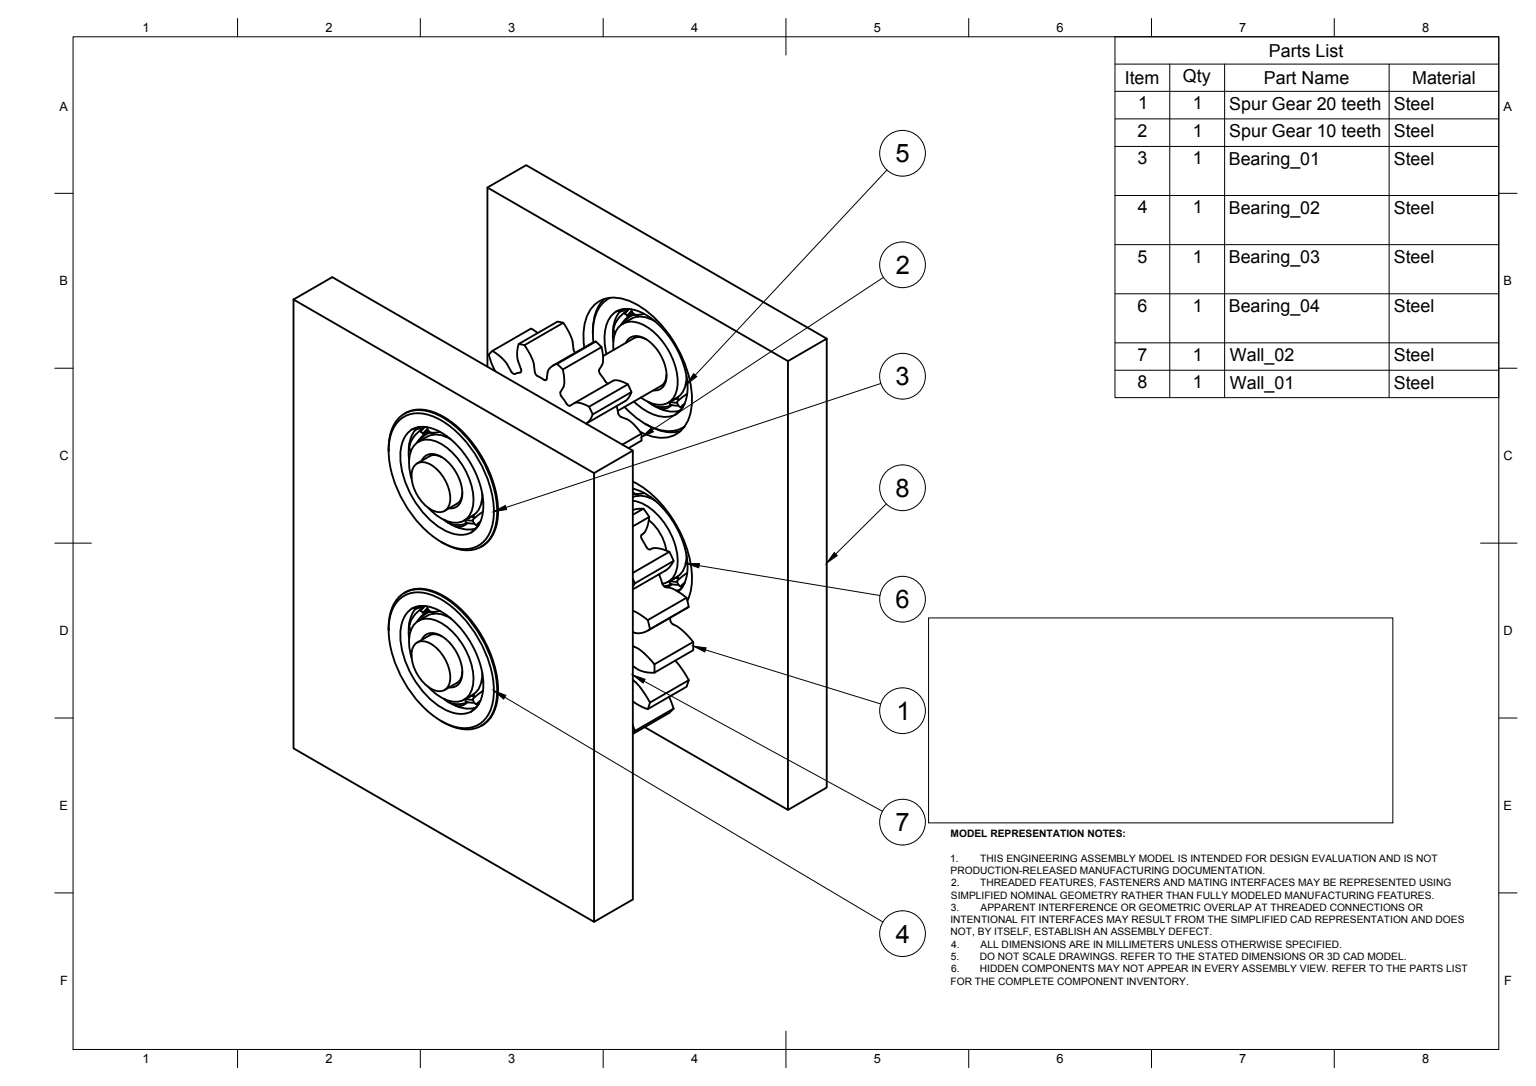
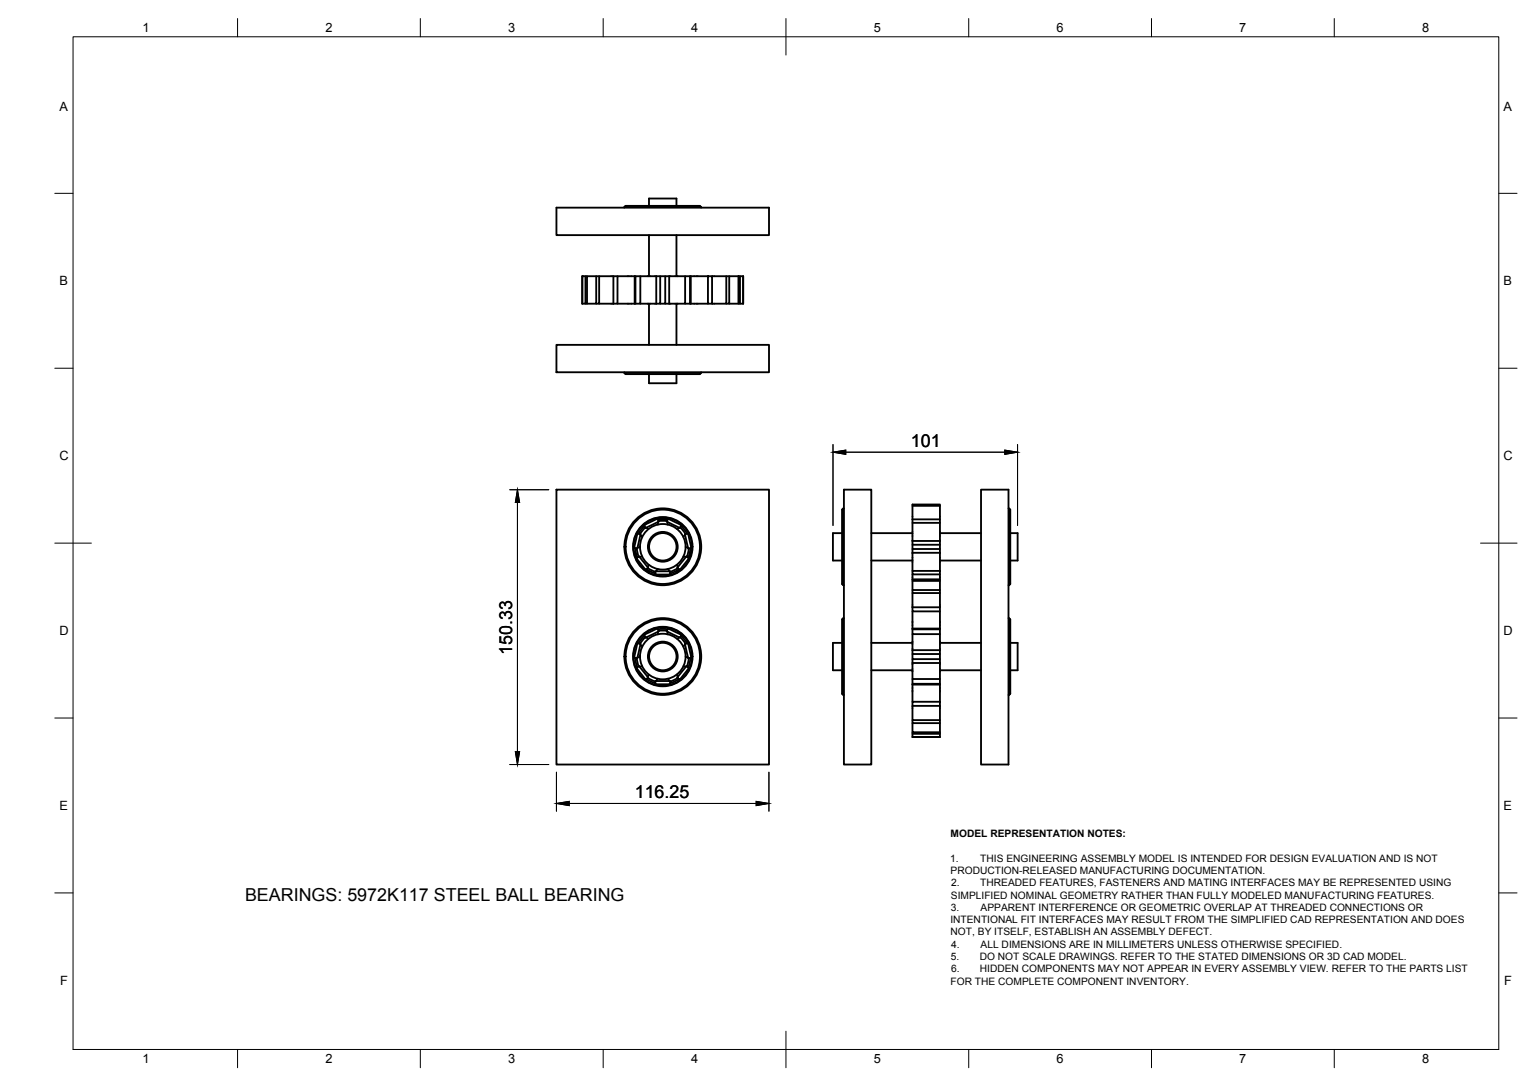
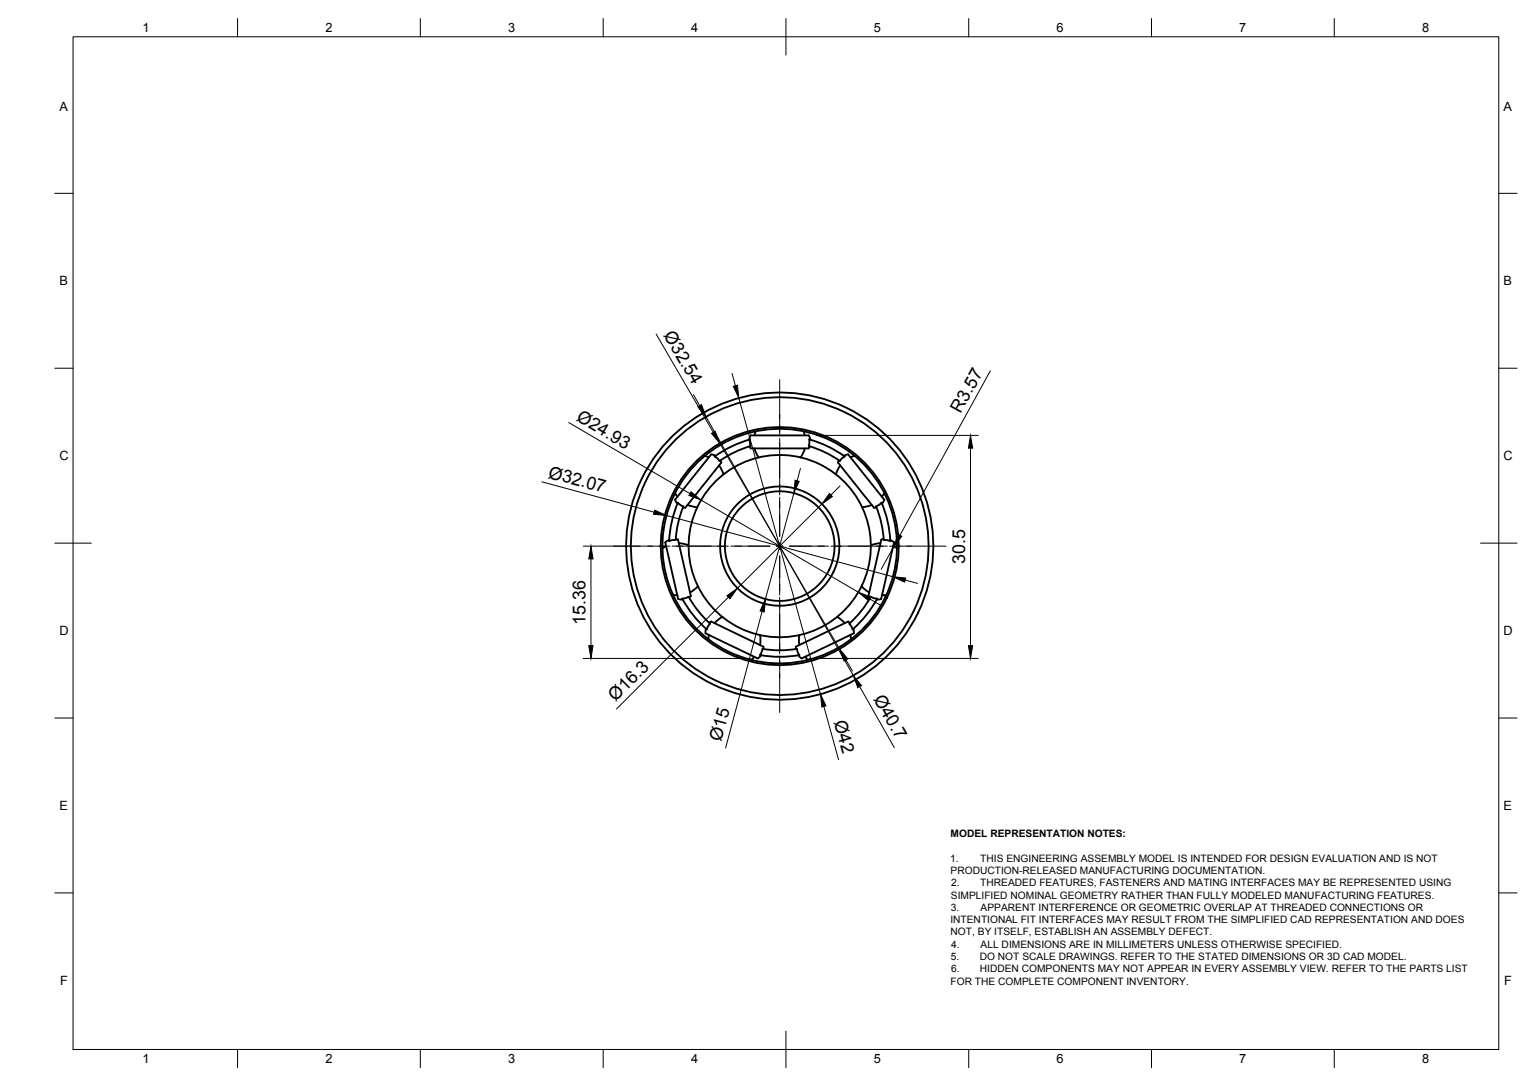
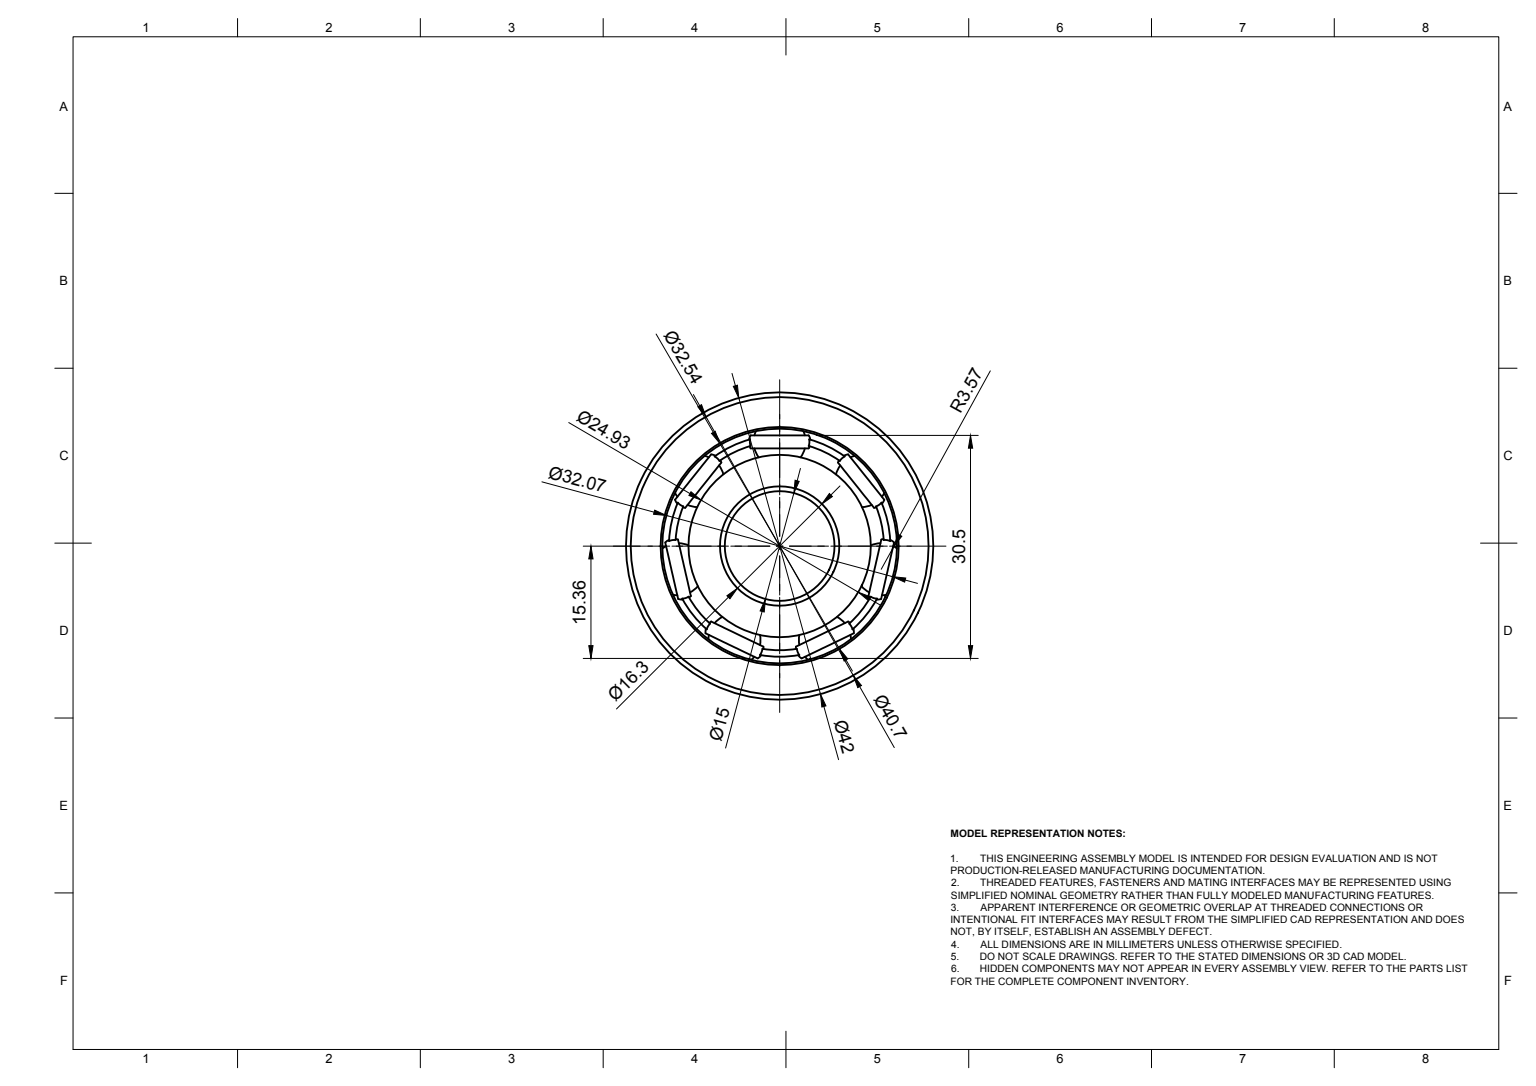
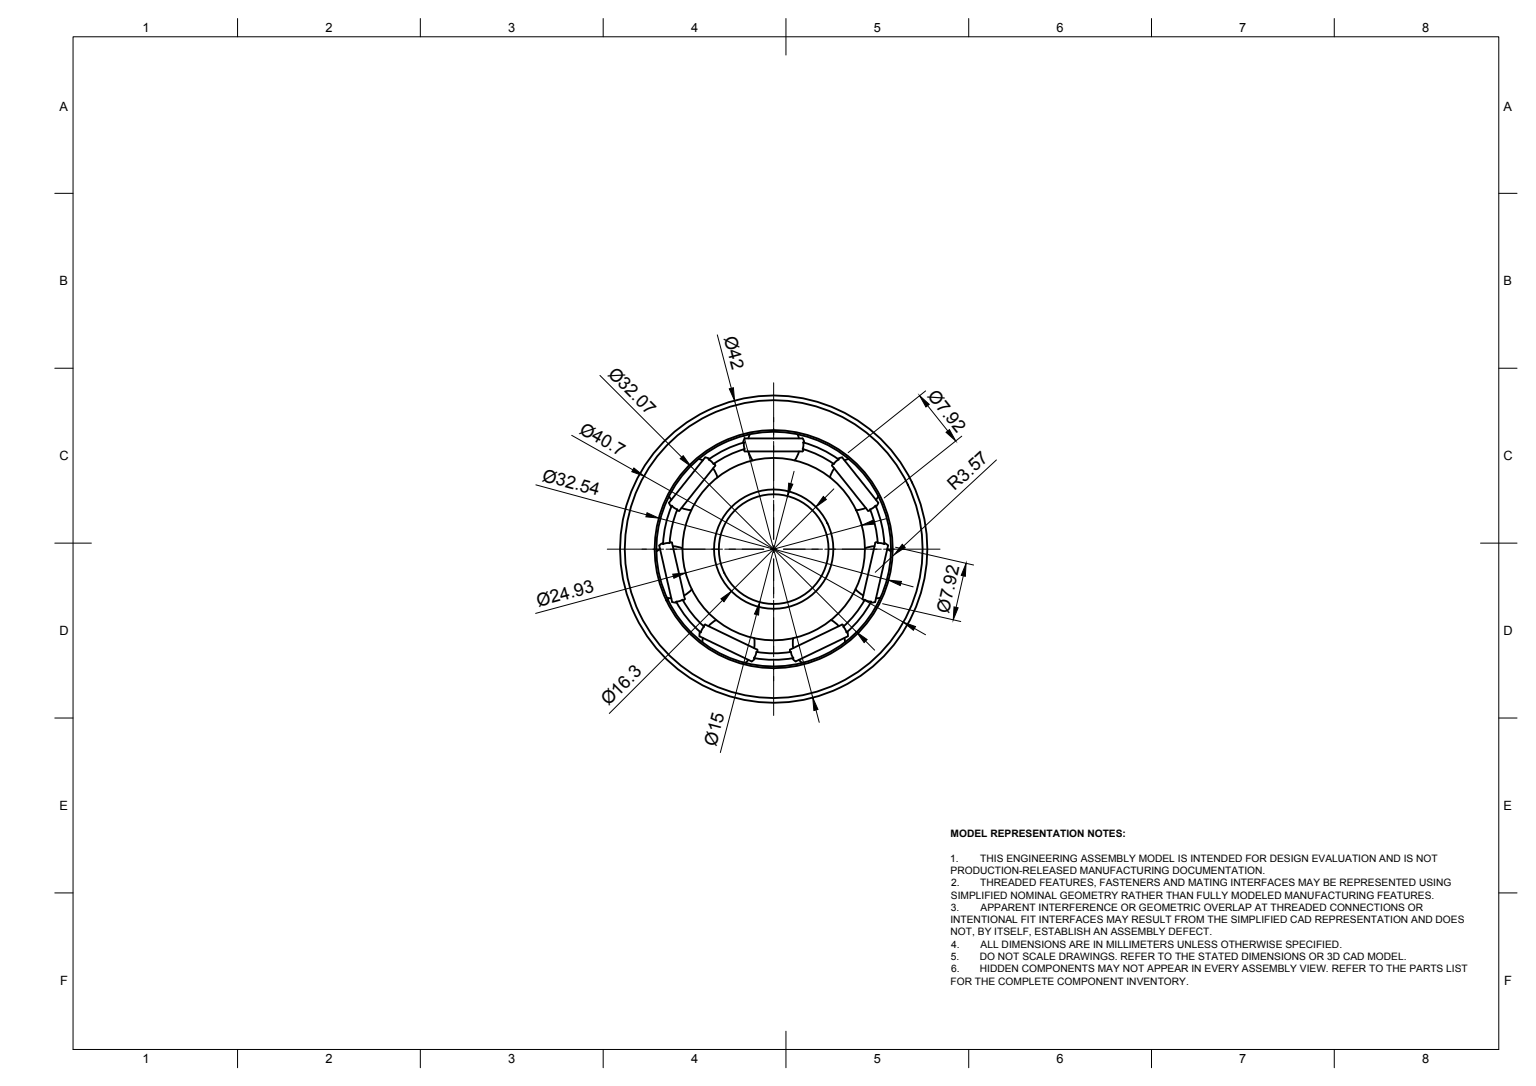
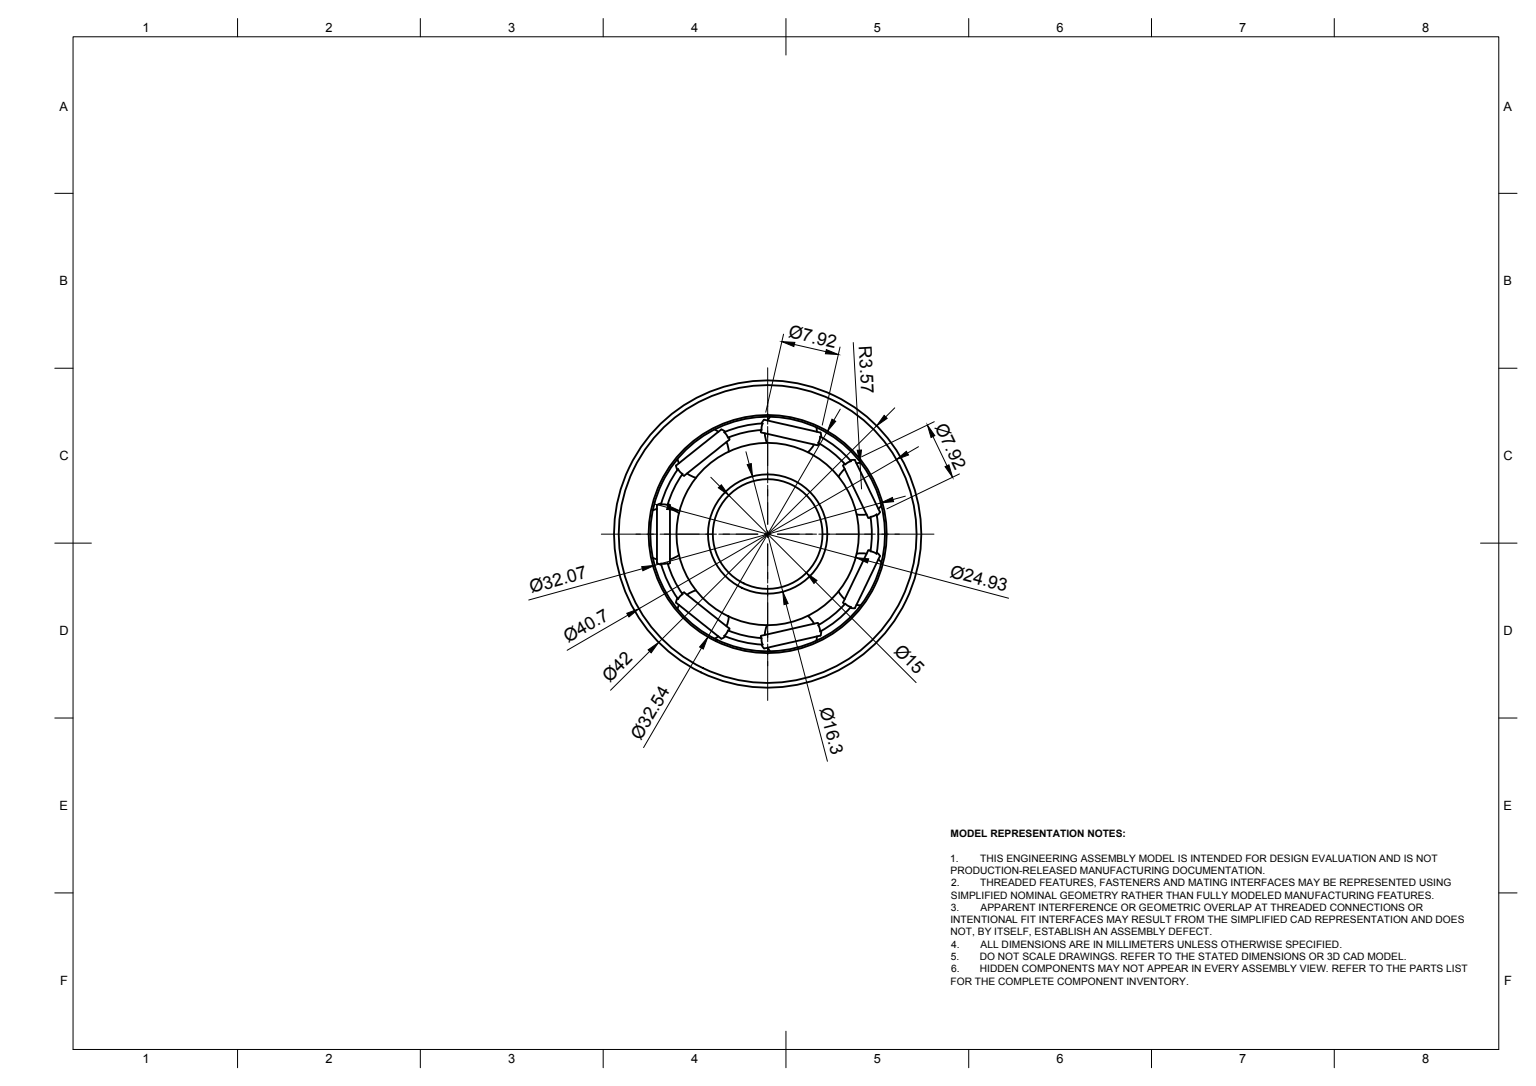
ISO-10303-21;
HEADER;
/* Generated by software containing ST-Developer
 * from STEP Tools, Inc. (www.steptools.com) 
 */

FILE_DESCRIPTION(
/* description */ (''),
/* implementation_level */ '2;1');

FILE_NAME(
/* name */ 'BR-258',
/* time_stamp */ '2026-10-05T21:54:13-07:00',
/* author */ (''),
/* organization */ (''),
/* preprocessor_version */ 'ST-DEVELOPER v20.2',
/* originating_system */ 'Autodesk Translation Framework v15.15.0.0',
/* authorisation */ '');

FILE_SCHEMA (('AUTOMOTIVE_DESIGN { 1 0 10303 214 3 1 1 }'));
ENDSEC;

DATA;
#10=MECHANICAL_DESIGN_GEOMETRIC_PRESENTATION_REPRESENTATION('',(#191,#192,
#193,#194,#195,#196,#197,#198,#199,#200,#201,#202,#203,#204,#205,#206,#207,
#208,#209,#210,#211,#212,#213,#214,#215,#216,#217,#218,#219,#220,#221,#222,
#223,#224,#225,#226,#227,#228,#229,#230,#231,#232,#233,#234),#43781);
#11=ITEM_DEFINED_TRANSFORMATION($,$,#13185,#14905);
#12=ITEM_DEFINED_TRANSFORMATION($,$,#13476,#14906);
#13=ITEM_DEFINED_TRANSFORMATION($,$,#13627,#14907);
#14=ITEM_DEFINED_TRANSFORMATION($,$,#13940,#14908);
#15=ITEM_DEFINED_TRANSFORMATION($,$,#14253,#14909);
#16=ITEM_DEFINED_TRANSFORMATION($,$,#14566,#14910);
#17=ITEM_DEFINED_TRANSFORMATION($,$,#14879,#14911);
#18=ITEM_DEFINED_TRANSFORMATION($,$,#14892,#14912);
#19=(
REPRESENTATION_RELATIONSHIP($,$,#43813,#43812)
REPRESENTATION_RELATIONSHIP_WITH_TRANSFORMATION(#11)
SHAPE_REPRESENTATION_RELATIONSHIP()
);
#20=(
REPRESENTATION_RELATIONSHIP($,$,#43814,#43812)
REPRESENTATION_RELATIONSHIP_WITH_TRANSFORMATION(#12)
SHAPE_REPRESENTATION_RELATIONSHIP()
);
#21=(
REPRESENTATION_RELATIONSHIP($,$,#43815,#43812)
REPRESENTATION_RELATIONSHIP_WITH_TRANSFORMATION(#13)
SHAPE_REPRESENTATION_RELATIONSHIP()
);
#22=(
REPRESENTATION_RELATIONSHIP($,$,#43816,#43812)
REPRESENTATION_RELATIONSHIP_WITH_TRANSFORMATION(#14)
SHAPE_REPRESENTATION_RELATIONSHIP()
);
#23=(
REPRESENTATION_RELATIONSHIP($,$,#43817,#43812)
REPRESENTATION_RELATIONSHIP_WITH_TRANSFORMATION(#15)
SHAPE_REPRESENTATION_RELATIONSHIP()
);
#24=(
REPRESENTATION_RELATIONSHIP($,$,#43818,#43812)
REPRESENTATION_RELATIONSHIP_WITH_TRANSFORMATION(#16)
SHAPE_REPRESENTATION_RELATIONSHIP()
);
#25=(
REPRESENTATION_RELATIONSHIP($,$,#43819,#43812)
REPRESENTATION_RELATIONSHIP_WITH_TRANSFORMATION(#17)
SHAPE_REPRESENTATION_RELATIONSHIP()
);
#26=(
REPRESENTATION_RELATIONSHIP($,$,#43820,#43812)
REPRESENTATION_RELATIONSHIP_WITH_TRANSFORMATION(#18)
SHAPE_REPRESENTATION_RELATIONSHIP()
);
#27=CONTEXT_DEPENDENT_SHAPE_REPRESENTATION(#19,#43804);
#28=CONTEXT_DEPENDENT_SHAPE_REPRESENTATION(#20,#43805);
#29=CONTEXT_DEPENDENT_SHAPE_REPRESENTATION(#21,#43806);
#30=CONTEXT_DEPENDENT_SHAPE_REPRESENTATION(#22,#43807);
#31=CONTEXT_DEPENDENT_SHAPE_REPRESENTATION(#23,#43808);
#32=CONTEXT_DEPENDENT_SHAPE_REPRESENTATION(#24,#43809);
#33=CONTEXT_DEPENDENT_SHAPE_REPRESENTATION(#25,#43810);
#34=CONTEXT_DEPENDENT_SHAPE_REPRESENTATION(#26,#43811);
#35=NEXT_ASSEMBLY_USAGE_OCCURRENCE('Spur Gear 20 teeth:1',
'Spur Gear 20 teeth:1','Spur Gear 20 teeth:1',#43822,#43823,
'Spur Gear 20 teeth:1');
#36=NEXT_ASSEMBLY_USAGE_OCCURRENCE('Spur Gear 10 teeth:1',
'Spur Gear 10 teeth:1','Spur Gear 10 teeth:1',#43822,#43824,
'Spur Gear 10 teeth:1');
#37=NEXT_ASSEMBLY_USAGE_OCCURRENCE('Bearing_01:1','Bearing_01:1',
'Bearing_01:1',#43822,#43825,'Bearing_01:1');
#38=NEXT_ASSEMBLY_USAGE_OCCURRENCE('Bearing_02:1','Bearing_02:1',
'Bearing_02:1',#43822,#43826,'Bearing_02:1');
#39=NEXT_ASSEMBLY_USAGE_OCCURRENCE('Bearing_03:1','Bearing_03:1',
'Bearing_03:1',#43822,#43827,'Bearing_03:1');
#40=NEXT_ASSEMBLY_USAGE_OCCURRENCE('Bearing_04:1','Bearing_04:1',
'Bearing_04:1',#43822,#43828,'Bearing_04:1');
#41=NEXT_ASSEMBLY_USAGE_OCCURRENCE('Wall_02:1','Wall_02:1','Wall_02:1',
#43822,#43829,'Wall_02:1');
#42=NEXT_ASSEMBLY_USAGE_OCCURRENCE('Wall_01:1','Wall_01:1','Wall_01:1',
#43822,#43830,'Wall_01:1');
#43=SPHERICAL_SURFACE('',#13654,3.56616156686793);
#44=SPHERICAL_SURFACE('',#13656,3.56616156686793);
#45=SPHERICAL_SURFACE('',#13658,3.56616156686793);
#46=SPHERICAL_SURFACE('',#13660,3.56616156686793);
#47=SPHERICAL_SURFACE('',#13662,3.56616156686793);
#48=SPHERICAL_SURFACE('',#13664,3.56616156686793);
#49=SPHERICAL_SURFACE('',#13666,3.56616156686793);
#50=SPHERICAL_SURFACE('',#13720,3.56616156686792);
#51=SPHERICAL_SURFACE('',#13734,3.56616156686792);
#52=SPHERICAL_SURFACE('',#13748,3.56616156686792);
#53=SPHERICAL_SURFACE('',#13762,3.56616156686792);
#54=SPHERICAL_SURFACE('',#13776,3.56616156686792);
#55=SPHERICAL_SURFACE('',#13790,3.56616156686792);
#56=SPHERICAL_SURFACE('',#13800,3.56616156686792);
#57=SPHERICAL_SURFACE('',#13967,3.56616156686793);
#58=SPHERICAL_SURFACE('',#13969,3.56616156686793);
#59=SPHERICAL_SURFACE('',#13971,3.56616156686793);
#60=SPHERICAL_SURFACE('',#13973,3.56616156686793);
#61=SPHERICAL_SURFACE('',#13975,3.56616156686793);
#62=SPHERICAL_SURFACE('',#13977,3.56616156686793);
#63=SPHERICAL_SURFACE('',#13979,3.56616156686793);
#64=SPHERICAL_SURFACE('',#14033,3.56616156686792);
#65=SPHERICAL_SURFACE('',#14047,3.56616156686792);
#66=SPHERICAL_SURFACE('',#14061,3.56616156686792);
#67=SPHERICAL_SURFACE('',#14075,3.56616156686792);
#68=SPHERICAL_SURFACE('',#14089,3.56616156686792);
#69=SPHERICAL_SURFACE('',#14103,3.56616156686792);
#70=SPHERICAL_SURFACE('',#14113,3.56616156686792);
#71=SPHERICAL_SURFACE('',#14280,3.56616156686793);
#72=SPHERICAL_SURFACE('',#14282,3.56616156686793);
#73=SPHERICAL_SURFACE('',#14284,3.56616156686793);
#74=SPHERICAL_SURFACE('',#14286,3.56616156686793);
#75=SPHERICAL_SURFACE('',#14288,3.56616156686793);
#76=SPHERICAL_SURFACE('',#14290,3.56616156686793);
#77=SPHERICAL_SURFACE('',#14292,3.56616156686793);
#78=SPHERICAL_SURFACE('',#14346,3.56616156686792);
#79=SPHERICAL_SURFACE('',#14360,3.56616156686792);
#80=SPHERICAL_SURFACE('',#14374,3.56616156686792);
#81=SPHERICAL_SURFACE('',#14388,3.56616156686792);
#82=SPHERICAL_SURFACE('',#14402,3.56616156686792);
#83=SPHERICAL_SURFACE('',#14416,3.56616156686792);
#84=SPHERICAL_SURFACE('',#14426,3.56616156686792);
#85=SPHERICAL_SURFACE('',#14593,3.56616156686793);
#86=SPHERICAL_SURFACE('',#14595,3.56616156686793);
#87=SPHERICAL_SURFACE('',#14597,3.56616156686793);
#88=SPHERICAL_SURFACE('',#14599,3.56616156686793);
#89=SPHERICAL_SURFACE('',#14601,3.56616156686793);
#90=SPHERICAL_SURFACE('',#14603,3.56616156686793);
#91=SPHERICAL_SURFACE('',#14605,3.56616156686793);
#92=SPHERICAL_SURFACE('',#14659,3.56616156686792);
#93=SPHERICAL_SURFACE('',#14673,3.56616156686792);
#94=SPHERICAL_SURFACE('',#14687,3.56616156686792);
#95=SPHERICAL_SURFACE('',#14701,3.56616156686792);
#96=SPHERICAL_SURFACE('',#14715,3.56616156686792);
#97=SPHERICAL_SURFACE('',#14729,3.56616156686792);
#98=SPHERICAL_SURFACE('',#14739,3.56616156686792);
#99=CONICAL_SURFACE('',#13643,8.14999999999999,0.785398163397436);
#100=CONICAL_SURFACE('',#13646,7.5,0.785398163397437);
#101=CONICAL_SURFACE('',#13702,20.35,0.785398163397442);
#102=CONICAL_SURFACE('',#13705,21.,0.785398163397442);
#103=CONICAL_SURFACE('',#13956,8.14999999999999,0.785398163397436);
#104=CONICAL_SURFACE('',#13959,7.5,0.785398163397437);
#105=CONICAL_SURFACE('',#14015,20.35,0.785398163397442);
#106=CONICAL_SURFACE('',#14018,21.,0.785398163397442);
#107=CONICAL_SURFACE('',#14269,8.14999999999999,0.785398163397436);
#108=CONICAL_SURFACE('',#14272,7.5,0.785398163397437);
#109=CONICAL_SURFACE('',#14328,20.35,0.785398163397442);
#110=CONICAL_SURFACE('',#14331,21.,0.785398163397442);
#111=CONICAL_SURFACE('',#14582,8.14999999999999,0.785398163397436);
#112=CONICAL_SURFACE('',#14585,7.5,0.785398163397437);
#113=CONICAL_SURFACE('',#14641,20.35,0.785398163397442);
#114=CONICAL_SURFACE('',#14644,21.,0.785398163397442);
#115=TOROIDAL_SURFACE('',#13628,14.25,3.56616156686793);
#116=TOROIDAL_SURFACE('',#13632,7.9875,0.4875);
#117=TOROIDAL_SURFACE('',#13638,7.9875,0.4875);
#118=TOROIDAL_SURFACE('',#13668,16.3271153846154,0.0585);
#119=TOROIDAL_SURFACE('',#13673,16.0931153846154,0.0585);
#120=TOROIDAL_SURFACE('',#13677,16.3271153846154,0.0585);
#121=TOROIDAL_SURFACE('',#13681,16.0931153846154,0.0585);
#122=TOROIDAL_SURFACE('',#13693,14.25,3.56616156686793);
#123=TOROIDAL_SURFACE('',#13716,2.5198520116158,1.69469015025);
#124=TOROIDAL_SURFACE('',#13730,2.5198520116158,1.69469015025);
#125=TOROIDAL_SURFACE('',#13744,2.5198520116158,1.69469015025);
#126=TOROIDAL_SURFACE('',#13758,2.5198520116158,1.69469015025);
#127=TOROIDAL_SURFACE('',#13772,2.5198520116158,1.69469015025);
#128=TOROIDAL_SURFACE('',#13786,2.5198520116158,1.69469015025);
#129=TOROIDAL_SURFACE('',#13810,2.5198520116158,1.69469015025);
#130=TOROIDAL_SURFACE('',#13941,14.25,3.56616156686793);
#131=TOROIDAL_SURFACE('',#13945,7.9875,0.4875);
#132=TOROIDAL_SURFACE('',#13951,7.9875,0.4875);
#133=TOROIDAL_SURFACE('',#13981,16.3271153846154,0.0585);
#134=TOROIDAL_SURFACE('',#13986,16.0931153846154,0.0585);
#135=TOROIDAL_SURFACE('',#13990,16.3271153846154,0.0585);
#136=TOROIDAL_SURFACE('',#13994,16.0931153846154,0.0585);
#137=TOROIDAL_SURFACE('',#14006,14.25,3.56616156686793);
#138=TOROIDAL_SURFACE('',#14029,2.5198520116158,1.69469015025);
#139=TOROIDAL_SURFACE('',#14043,2.5198520116158,1.69469015025);
#140=TOROIDAL_SURFACE('',#14057,2.5198520116158,1.69469015025);
#141=TOROIDAL_SURFACE('',#14071,2.5198520116158,1.69469015025);
#142=TOROIDAL_SURFACE('',#14085,2.5198520116158,1.69469015025);
#143=TOROIDAL_SURFACE('',#14099,2.5198520116158,1.69469015025);
#144=TOROIDAL_SURFACE('',#14123,2.5198520116158,1.69469015025);
#145=TOROIDAL_SURFACE('',#14254,14.25,3.56616156686793);
#146=TOROIDAL_SURFACE('',#14258,7.9875,0.4875);
#147=TOROIDAL_SURFACE('',#14264,7.9875,0.4875);
#148=TOROIDAL_SURFACE('',#14294,16.3271153846154,0.0585);
#149=TOROIDAL_SURFACE('',#14299,16.0931153846154,0.0585);
#150=TOROIDAL_SURFACE('',#14303,16.3271153846154,0.0585);
#151=TOROIDAL_SURFACE('',#14307,16.0931153846154,0.0585);
#152=TOROIDAL_SURFACE('',#14319,14.25,3.56616156686793);
#153=TOROIDAL_SURFACE('',#14342,2.5198520116158,1.69469015025);
#154=TOROIDAL_SURFACE('',#14356,2.5198520116158,1.69469015025);
#155=TOROIDAL_SURFACE('',#14370,2.5198520116158,1.69469015025);
#156=TOROIDAL_SURFACE('',#14384,2.5198520116158,1.69469015025);
#157=TOROIDAL_SURFACE('',#14398,2.5198520116158,1.69469015025);
#158=TOROIDAL_SURFACE('',#14412,2.5198520116158,1.69469015025);
#159=TOROIDAL_SURFACE('',#14436,2.5198520116158,1.69469015025);
#160=TOROIDAL_SURFACE('',#14567,14.25,3.56616156686793);
#161=TOROIDAL_SURFACE('',#14571,7.9875,0.4875);
#162=TOROIDAL_SURFACE('',#14577,7.9875,0.4875);
#163=TOROIDAL_SURFACE('',#14607,16.3271153846154,0.0585);
#164=TOROIDAL_SURFACE('',#14612,16.0931153846154,0.0585);
#165=TOROIDAL_SURFACE('',#14616,16.3271153846154,0.0585);
#166=TOROIDAL_SURFACE('',#14620,16.0931153846154,0.0585);
#167=TOROIDAL_SURFACE('',#14632,14.25,3.56616156686793);
#168=TOROIDAL_SURFACE('',#14655,2.5198520116158,1.69469015025);
#169=TOROIDAL_SURFACE('',#14669,2.5198520116158,1.69469015025);
#170=TOROIDAL_SURFACE('',#14683,2.5198520116158,1.69469015025);
#171=TOROIDAL_SURFACE('',#14697,2.5198520116158,1.69469015025);
#172=TOROIDAL_SURFACE('',#14711,2.5198520116158,1.69469015025);
#173=TOROIDAL_SURFACE('',#14725,2.5198520116158,1.69469015025);
#174=TOROIDAL_SURFACE('',#14749,2.5198520116158,1.69469015025);
#175=SHAPE_REPRESENTATION_RELATIONSHIP('SRR','None',#43813,#183);
#176=SHAPE_REPRESENTATION_RELATIONSHIP('SRR','None',#43814,#184);
#177=SHAPE_REPRESENTATION_RELATIONSHIP('SRR','None',#43815,#185);
#178=SHAPE_REPRESENTATION_RELATIONSHIP('SRR','None',#43816,#186);
#179=SHAPE_REPRESENTATION_RELATIONSHIP('SRR','None',#43817,#187);
#180=SHAPE_REPRESENTATION_RELATIONSHIP('SRR','None',#43818,#188);
#181=SHAPE_REPRESENTATION_RELATIONSHIP('SRR','None',#43819,#189);
#182=SHAPE_REPRESENTATION_RELATIONSHIP('SRR','None',#43820,#190);
#183=ADVANCED_BREP_SHAPE_REPRESENTATION('',(#235),#43773);
#184=ADVANCED_BREP_SHAPE_REPRESENTATION('',(#236),#43774);
#185=ADVANCED_BREP_SHAPE_REPRESENTATION('',(#237,#238,#239,#240,#241,#242,
#243,#244,#245,#246),#43775);
#186=ADVANCED_BREP_SHAPE_REPRESENTATION('',(#247,#248,#249,#250,#251,#252,
#253,#254,#255,#256),#43776);
#187=ADVANCED_BREP_SHAPE_REPRESENTATION('',(#257,#258,#259,#260,#261,#262,
#263,#264,#265,#266),#43777);
#188=ADVANCED_BREP_SHAPE_REPRESENTATION('',(#267,#268,#269,#270,#271,#272,
#273,#274,#275,#276),#43778);
#189=ADVANCED_BREP_SHAPE_REPRESENTATION('',(#277),#43779);
#190=ADVANCED_BREP_SHAPE_REPRESENTATION('',(#278),#43780);
#191=STYLED_ITEM('',(#43862),#235);
#192=STYLED_ITEM('',(#43862),#236);
#193=STYLED_ITEM('',(#43863),#237);
#194=STYLED_ITEM('',(#43863),#238);
#195=STYLED_ITEM('',(#43863),#239);
#196=STYLED_ITEM('',(#43863),#240);
#197=STYLED_ITEM('',(#43863),#241);
#198=STYLED_ITEM('',(#43863),#242);
#199=STYLED_ITEM('',(#43863),#243);
#200=STYLED_ITEM('',(#43863),#244);
#201=STYLED_ITEM('',(#43863),#245);
#202=STYLED_ITEM('',(#43863),#246);
#203=STYLED_ITEM('',(#43863),#247);
#204=STYLED_ITEM('',(#43863),#248);
#205=STYLED_ITEM('',(#43863),#249);
#206=STYLED_ITEM('',(#43863),#250);
#207=STYLED_ITEM('',(#43863),#251);
#208=STYLED_ITEM('',(#43863),#252);
#209=STYLED_ITEM('',(#43863),#253);
#210=STYLED_ITEM('',(#43863),#254);
#211=STYLED_ITEM('',(#43863),#255);
#212=STYLED_ITEM('',(#43863),#256);
#213=STYLED_ITEM('',(#43863),#257);
#214=STYLED_ITEM('',(#43863),#258);
#215=STYLED_ITEM('',(#43863),#259);
#216=STYLED_ITEM('',(#43863),#260);
#217=STYLED_ITEM('',(#43863),#261);
#218=STYLED_ITEM('',(#43863),#262);
#219=STYLED_ITEM('',(#43863),#263);
#220=STYLED_ITEM('',(#43863),#264);
#221=STYLED_ITEM('',(#43863),#265);
#222=STYLED_ITEM('',(#43863),#266);
#223=STYLED_ITEM('',(#43863),#267);
#224=STYLED_ITEM('',(#43863),#268);
#225=STYLED_ITEM('',(#43863),#269);
#226=STYLED_ITEM('',(#43863),#270);
#227=STYLED_ITEM('',(#43863),#271);
#228=STYLED_ITEM('',(#43863),#272);
#229=STYLED_ITEM('',(#43863),#273);
#230=STYLED_ITEM('',(#43863),#274);
#231=STYLED_ITEM('',(#43863),#275);
#232=STYLED_ITEM('',(#43863),#276);
#233=STYLED_ITEM('',(#43863),#277);
#234=STYLED_ITEM('',(#43863),#278);
#235=MANIFOLD_SOLID_BREP('Body1',#13051);
#236=MANIFOLD_SOLID_BREP('Body1',#13052);
#237=MANIFOLD_SOLID_BREP('Body1',#13053);
#238=MANIFOLD_SOLID_BREP('Body2',#13054);
#239=MANIFOLD_SOLID_BREP('Body3',#13055);
#240=MANIFOLD_SOLID_BREP('Body4',#13056);
#241=MANIFOLD_SOLID_BREP('Body5',#13057);
#242=MANIFOLD_SOLID_BREP('Body6',#13058);
#243=MANIFOLD_SOLID_BREP('Body7',#13059);
#244=MANIFOLD_SOLID_BREP('Body8',#13060);
#245=MANIFOLD_SOLID_BREP('Body9',#13061);
#246=MANIFOLD_SOLID_BREP('Body10',#13062);
#247=MANIFOLD_SOLID_BREP('Body1',#13063);
#248=MANIFOLD_SOLID_BREP('Body2',#13064);
#249=MANIFOLD_SOLID_BREP('Body3',#13065);
#250=MANIFOLD_SOLID_BREP('Body4',#13066);
#251=MANIFOLD_SOLID_BREP('Body5',#13067);
#252=MANIFOLD_SOLID_BREP('Body6',#13068);
#253=MANIFOLD_SOLID_BREP('Body7',#13069);
#254=MANIFOLD_SOLID_BREP('Body8',#13070);
#255=MANIFOLD_SOLID_BREP('Body9',#13071);
#256=MANIFOLD_SOLID_BREP('Body10',#13072);
#257=MANIFOLD_SOLID_BREP('Body1',#13073);
#258=MANIFOLD_SOLID_BREP('Body2',#13074);
#259=MANIFOLD_SOLID_BREP('Body3',#13075);
#260=MANIFOLD_SOLID_BREP('Body4',#13076);
#261=MANIFOLD_SOLID_BREP('Body5',#13077);
#262=MANIFOLD_SOLID_BREP('Body6',#13078);
#263=MANIFOLD_SOLID_BREP('Body7',#13079);
#264=MANIFOLD_SOLID_BREP('Body8',#13080);
#265=MANIFOLD_SOLID_BREP('Body9',#13081);
#266=MANIFOLD_SOLID_BREP('Body10',#13082);
#267=MANIFOLD_SOLID_BREP('Body1',#13083);
#268=MANIFOLD_SOLID_BREP('Body2',#13084);
#269=MANIFOLD_SOLID_BREP('Body3',#13085);
#270=MANIFOLD_SOLID_BREP('Body4',#13086);
#271=MANIFOLD_SOLID_BREP('Body5',#13087);
#272=MANIFOLD_SOLID_BREP('Body6',#13088);
#273=MANIFOLD_SOLID_BREP('Body7',#13089);
#274=MANIFOLD_SOLID_BREP('Body8',#13090);
#275=MANIFOLD_SOLID_BREP('Body9',#13091);
#276=MANIFOLD_SOLID_BREP('Body10',#13092);
#277=MANIFOLD_SOLID_BREP('Body1',#13093);
#278=MANIFOLD_SOLID_BREP('Body1',#13094);
#279=FACE_BOUND('',#2177,.T.);
#280=FACE_BOUND('',#2179,.T.);
#281=FACE_BOUND('',#2275,.T.);
#282=FACE_BOUND('',#2277,.T.);
#283=FACE_BOUND('',#2304,.T.);
#284=FACE_BOUND('',#2306,.T.);
#285=FACE_BOUND('',#2329,.T.);
#286=FACE_BOUND('',#2331,.T.);
#287=FACE_BOUND('',#2333,.T.);
#288=FACE_BOUND('',#2335,.T.);
#289=FACE_BOUND('',#2337,.T.);
#290=FACE_BOUND('',#2339,.T.);
#291=FACE_BOUND('',#2341,.T.);
#292=FACE_BOUND('',#2342,.T.);
#293=FACE_BOUND('',#2344,.T.);
#294=FACE_BOUND('',#2345,.T.);
#295=FACE_BOUND('',#2347,.T.);
#296=FACE_BOUND('',#2348,.T.);
#297=FACE_BOUND('',#2350,.T.);
#298=FACE_BOUND('',#2351,.T.);
#299=FACE_BOUND('',#2353,.T.);
#300=FACE_BOUND('',#2354,.T.);
#301=FACE_BOUND('',#2356,.T.);
#302=FACE_BOUND('',#2357,.T.);
#303=FACE_BOUND('',#2359,.T.);
#304=FACE_BOUND('',#2360,.T.);
#305=FACE_BOUND('',#2362,.T.);
#306=FACE_BOUND('',#2363,.T.);
#307=FACE_BOUND('',#2365,.T.);
#308=FACE_BOUND('',#2366,.T.);
#309=FACE_BOUND('',#2368,.T.);
#310=FACE_BOUND('',#2369,.T.);
#311=FACE_BOUND('',#2371,.T.);
#312=FACE_BOUND('',#2372,.T.);
#313=FACE_BOUND('',#2374,.T.);
#314=FACE_BOUND('',#2375,.T.);
#315=FACE_BOUND('',#2377,.T.);
#316=FACE_BOUND('',#2378,.T.);
#317=FACE_BOUND('',#2380,.T.);
#318=FACE_BOUND('',#2381,.T.);
#319=FACE_BOUND('',#2387,.T.);
#320=FACE_BOUND('',#2389,.T.);
#321=FACE_BOUND('',#2395,.T.);
#322=FACE_BOUND('',#2397,.T.);
#323=FACE_BOUND('',#2407,.T.);
#324=FACE_BOUND('',#2409,.T.);
#325=FACE_BOUND('',#2419,.T.);
#326=FACE_BOUND('',#2421,.T.);
#327=FACE_BOUND('',#2431,.T.);
#328=FACE_BOUND('',#2433,.T.);
#329=FACE_BOUND('',#2443,.T.);
#330=FACE_BOUND('',#2445,.T.);
#331=FACE_BOUND('',#2455,.T.);
#332=FACE_BOUND('',#2457,.T.);
#333=FACE_BOUND('',#2475,.T.);
#334=FACE_BOUND('',#2477,.T.);
#335=FACE_BOUND('',#2500,.T.);
#336=FACE_BOUND('',#2502,.T.);
#337=FACE_BOUND('',#2504,.T.);
#338=FACE_BOUND('',#2506,.T.);
#339=FACE_BOUND('',#2508,.T.);
#340=FACE_BOUND('',#2510,.T.);
#341=FACE_BOUND('',#2512,.T.);
#342=FACE_BOUND('',#2513,.T.);
#343=FACE_BOUND('',#2515,.T.);
#344=FACE_BOUND('',#2516,.T.);
#345=FACE_BOUND('',#2518,.T.);
#346=FACE_BOUND('',#2519,.T.);
#347=FACE_BOUND('',#2521,.T.);
#348=FACE_BOUND('',#2522,.T.);
#349=FACE_BOUND('',#2524,.T.);
#350=FACE_BOUND('',#2525,.T.);
#351=FACE_BOUND('',#2527,.T.);
#352=FACE_BOUND('',#2528,.T.);
#353=FACE_BOUND('',#2530,.T.);
#354=FACE_BOUND('',#2531,.T.);
#355=FACE_BOUND('',#2533,.T.);
#356=FACE_BOUND('',#2534,.T.);
#357=FACE_BOUND('',#2536,.T.);
#358=FACE_BOUND('',#2537,.T.);
#359=FACE_BOUND('',#2539,.T.);
#360=FACE_BOUND('',#2540,.T.);
#361=FACE_BOUND('',#2542,.T.);
#362=FACE_BOUND('',#2543,.T.);
#363=FACE_BOUND('',#2545,.T.);
#364=FACE_BOUND('',#2546,.T.);
#365=FACE_BOUND('',#2548,.T.);
#366=FACE_BOUND('',#2549,.T.);
#367=FACE_BOUND('',#2551,.T.);
#368=FACE_BOUND('',#2552,.T.);
#369=FACE_BOUND('',#2558,.T.);
#370=FACE_BOUND('',#2560,.T.);
#371=FACE_BOUND('',#2566,.T.);
#372=FACE_BOUND('',#2568,.T.);
#373=FACE_BOUND('',#2578,.T.);
#374=FACE_BOUND('',#2580,.T.);
#375=FACE_BOUND('',#2590,.T.);
#376=FACE_BOUND('',#2592,.T.);
#377=FACE_BOUND('',#2602,.T.);
#378=FACE_BOUND('',#2604,.T.);
#379=FACE_BOUND('',#2614,.T.);
#380=FACE_BOUND('',#2616,.T.);
#381=FACE_BOUND('',#2626,.T.);
#382=FACE_BOUND('',#2628,.T.);
#383=FACE_BOUND('',#2646,.T.);
#384=FACE_BOUND('',#2648,.T.);
#385=FACE_BOUND('',#2671,.T.);
#386=FACE_BOUND('',#2673,.T.);
#387=FACE_BOUND('',#2675,.T.);
#388=FACE_BOUND('',#2677,.T.);
#389=FACE_BOUND('',#2679,.T.);
#390=FACE_BOUND('',#2681,.T.);
#391=FACE_BOUND('',#2683,.T.);
#392=FACE_BOUND('',#2684,.T.);
#393=FACE_BOUND('',#2686,.T.);
#394=FACE_BOUND('',#2687,.T.);
#395=FACE_BOUND('',#2689,.T.);
#396=FACE_BOUND('',#2690,.T.);
#397=FACE_BOUND('',#2692,.T.);
#398=FACE_BOUND('',#2693,.T.);
#399=FACE_BOUND('',#2695,.T.);
#400=FACE_BOUND('',#2696,.T.);
#401=FACE_BOUND('',#2698,.T.);
#402=FACE_BOUND('',#2699,.T.);
#403=FACE_BOUND('',#2701,.T.);
#404=FACE_BOUND('',#2702,.T.);
#405=FACE_BOUND('',#2704,.T.);
#406=FACE_BOUND('',#2705,.T.);
#407=FACE_BOUND('',#2707,.T.);
#408=FACE_BOUND('',#2708,.T.);
#409=FACE_BOUND('',#2710,.T.);
#410=FACE_BOUND('',#2711,.T.);
#411=FACE_BOUND('',#2713,.T.);
#412=FACE_BOUND('',#2714,.T.);
#413=FACE_BOUND('',#2716,.T.);
#414=FACE_BOUND('',#2717,.T.);
#415=FACE_BOUND('',#2719,.T.);
#416=FACE_BOUND('',#2720,.T.);
#417=FACE_BOUND('',#2722,.T.);
#418=FACE_BOUND('',#2723,.T.);
#419=FACE_BOUND('',#2729,.T.);
#420=FACE_BOUND('',#2731,.T.);
#421=FACE_BOUND('',#2737,.T.);
#422=FACE_BOUND('',#2739,.T.);
#423=FACE_BOUND('',#2749,.T.);
#424=FACE_BOUND('',#2751,.T.);
#425=FACE_BOUND('',#2761,.T.);
#426=FACE_BOUND('',#2763,.T.);
#427=FACE_BOUND('',#2773,.T.);
#428=FACE_BOUND('',#2775,.T.);
#429=FACE_BOUND('',#2785,.T.);
#430=FACE_BOUND('',#2787,.T.);
#431=FACE_BOUND('',#2797,.T.);
#432=FACE_BOUND('',#2799,.T.);
#433=FACE_BOUND('',#2817,.T.);
#434=FACE_BOUND('',#2819,.T.);
#435=FACE_BOUND('',#2842,.T.);
#436=FACE_BOUND('',#2844,.T.);
#437=FACE_BOUND('',#2846,.T.);
#438=FACE_BOUND('',#2848,.T.);
#439=FACE_BOUND('',#2850,.T.);
#440=FACE_BOUND('',#2852,.T.);
#441=FACE_BOUND('',#2854,.T.);
#442=FACE_BOUND('',#2855,.T.);
#443=FACE_BOUND('',#2857,.T.);
#444=FACE_BOUND('',#2858,.T.);
#445=FACE_BOUND('',#2860,.T.);
#446=FACE_BOUND('',#2861,.T.);
#447=FACE_BOUND('',#2863,.T.);
#448=FACE_BOUND('',#2864,.T.);
#449=FACE_BOUND('',#2866,.T.);
#450=FACE_BOUND('',#2867,.T.);
#451=FACE_BOUND('',#2869,.T.);
#452=FACE_BOUND('',#2870,.T.);
#453=FACE_BOUND('',#2872,.T.);
#454=FACE_BOUND('',#2873,.T.);
#455=FACE_BOUND('',#2875,.T.);
#456=FACE_BOUND('',#2876,.T.);
#457=FACE_BOUND('',#2878,.T.);
#458=FACE_BOUND('',#2879,.T.);
#459=FACE_BOUND('',#2881,.T.);
#460=FACE_BOUND('',#2882,.T.);
#461=FACE_BOUND('',#2884,.T.);
#462=FACE_BOUND('',#2885,.T.);
#463=FACE_BOUND('',#2887,.T.);
#464=FACE_BOUND('',#2888,.T.);
#465=FACE_BOUND('',#2890,.T.);
#466=FACE_BOUND('',#2891,.T.);
#467=FACE_BOUND('',#2893,.T.);
#468=FACE_BOUND('',#2894,.T.);
#469=FACE_BOUND('',#2900,.T.);
#470=FACE_BOUND('',#2902,.T.);
#471=FACE_BOUND('',#2908,.T.);
#472=FACE_BOUND('',#2910,.T.);
#473=FACE_BOUND('',#2920,.T.);
#474=FACE_BOUND('',#2922,.T.);
#475=FACE_BOUND('',#2932,.T.);
#476=FACE_BOUND('',#2934,.T.);
#477=FACE_BOUND('',#2944,.T.);
#478=FACE_BOUND('',#2946,.T.);
#479=FACE_BOUND('',#2956,.T.);
#480=FACE_BOUND('',#2958,.T.);
#481=FACE_BOUND('',#2968,.T.);
#482=FACE_BOUND('',#2970,.T.);
#483=FACE_BOUND('',#2981,.T.);
#484=FACE_BOUND('',#2982,.T.);
#485=FACE_BOUND('',#2985,.T.);
#486=FACE_BOUND('',#2986,.T.);
#487=FACE_BOUND('',#2994,.T.);
#488=FACE_BOUND('',#2995,.T.);
#489=FACE_BOUND('',#3001,.T.);
#490=FACE_BOUND('',#3002,.T.);
#491=B_SPLINE_CURVE_WITH_KNOTS('',5,(#19556,#19557,#19558,#19559,#19560,
#19561,#19562,#19563,#19564,#19565,#19566,#19567,#19568,#19569,#19570,#19571,
#19572,#19573,#19574,#19575,#19576,#19577,#19578,#19579,#19580,#19581,#19582,
#19583,#19584,#19585,#19586,#19587,#19588,#19589,#19590,#19591,#19592,#19593,
#19594,#19595,#19596,#19597,#19598,#19599,#19600,#19601,#19602,#19603,#19604,
#19605,#19606,#19607,#19608,#19609,#19610,#19611,#19612,#19613,#19614,#19615,
#19616,#19617,#19618,#19619,#19620,#19621,#19622,#19623,#19624,#19625,#19626,
#19627,#19628,#19629),.UNSPECIFIED.,.F.,.F.,(6,1,1,1,1,1,1,1,1,1,1,1,1,
1,1,1,1,1,1,1,1,1,1,1,1,1,1,1,1,1,1,1,1,1,1,1,1,1,1,1,1,1,1,1,1,1,1,1,1,
1,1,1,1,1,1,1,1,1,1,1,1,1,1,1,1,1,1,1,1,6),(0.,0.0142857142857143,0.0285714285714286,
0.0428571428571429,0.0571428571428571,0.0714285714285714,0.0857142857142857,
0.1,0.114285714285714,0.128571428571429,0.142857142857143,0.157142857142857,
0.171428571428571,0.185714285714286,0.2,0.214285714285714,0.228571428571429,
0.242857142857143,0.257142857142857,0.271428571428571,0.285714285714286,
0.3,0.314285714285714,0.328571428571429,0.342857142857143,0.357142857142857,
0.371428571428571,0.385714285714286,0.4,0.414285714285714,0.428571428571429,
0.442857142857143,0.457142857142857,0.471428571428572,0.485714285714286,
0.5,0.514285714285714,0.528571428571429,0.542857142857143,0.557142857142857,
0.571428571428571,0.585714285714286,0.6,0.614285714285714,0.628571428571428,
0.642857142857142,0.657142857142857,0.671428571428571,0.685714285714285,
0.699999999999999,0.714285714285714,0.728571428571428,0.742857142857142,
0.757142857142856,0.771428571428571,0.785714285714285,0.799999999999999,
0.814285714285713,0.828571428571428,0.842857142857142,0.857142857142856,
0.87142857142857,0.885714285714284,0.899999999999999,0.914285714285713,
0.928571428571427,0.942857142857141,0.957142857142856,0.97142857142857,
1.),.UNSPECIFIED.);
#492=B_SPLINE_CURVE_WITH_KNOTS('',5,(#19631,#19632,#19633,#19634,#19635,
#19636,#19637,#19638,#19639,#19640,#19641,#19642,#19643,#19644,#19645,#19646,
#19647,#19648,#19649,#19650,#19651,#19652,#19653,#19654,#19655,#19656,#19657,
#19658,#19659,#19660,#19661,#19662,#19663,#19664,#19665,#19666,#19667,#19668,
#19669,#19670,#19671,#19672,#19673,#19674,#19675,#19676,#19677,#19678,#19679,
#19680,#19681,#19682,#19683,#19684,#19685,#19686,#19687,#19688,#19689,#19690,
#19691,#19692,#19693,#19694,#19695,#19696,#19697,#19698,#19699,#19700,#19701,
#19702,#19703,#19704,#19705),.UNSPECIFIED.,.F.,.F.,(6,1,1,1,1,1,1,1,1,1,
1,1,1,1,1,1,1,1,1,1,1,1,1,1,1,1,1,1,1,1,1,1,1,1,1,1,1,1,1,1,1,1,1,1,1,1,
1,1,1,1,1,1,1,1,1,1,1,1,1,1,1,1,1,1,1,1,1,1,1,1,6),(-1.,-0.985714285714284,
-0.97142857142857,-0.957142857142856,-0.942857142857141,-0.928571428571427,
-0.914285714285713,-0.899999999999999,-0.885714285714284,-0.87142857142857,
-0.857142857142856,-0.842857142857142,-0.828571428571428,-0.814285714285713,
-0.799999999999999,-0.785714285714285,-0.771428571428571,-0.757142857142856,
-0.742857142857142,-0.728571428571428,-0.714285714285714,-0.699999999999999,
-0.685714285714285,-0.671428571428571,-0.657142857142857,-0.642857142857142,
-0.628571428571428,-0.614285714285714,-0.6,-0.585714285714286,-0.571428571428571,
-0.557142857142857,-0.542857142857143,-0.528571428571429,-0.514285714285714,
-0.5,-0.485714285714286,-0.471428571428572,-0.457142857142857,-0.442857142857143,
-0.428571428571429,-0.414285714285714,-0.4,-0.385714285714286,-0.371428571428571,
-0.357142857142857,-0.342857142857143,-0.328571428571429,-0.314285714285714,
-0.3,-0.285714285714286,-0.271428571428571,-0.257142857142857,-0.242857142857143,
-0.228571428571429,-0.214285714285714,-0.2,-0.185714285714286,-0.171428571428571,
-0.157142857142857,-0.142857142857143,-0.128571428571429,-0.114285714285714,
-0.1,-0.0857142857142857,-0.0714285714285714,-0.0571428571428571,-0.0428571428571429,
-0.0285714285714286,-0.0142857142857143,0.),.UNSPECIFIED.);
#493=B_SPLINE_CURVE_WITH_KNOTS('',5,(#19863,#19864,#19865,#19866,#19867,
#19868,#19869,#19870,#19871,#19872,#19873,#19874,#19875,#19876,#19877,#19878,
#19879,#19880,#19881,#19882,#19883,#19884,#19885,#19886,#19887,#19888,#19889,
#19890,#19891,#19892,#19893,#19894,#19895,#19896,#19897,#19898,#19899,#19900,
#19901,#19902,#19903,#19904,#19905,#19906,#19907,#19908,#19909,#19910,#19911,
#19912,#19913,#19914,#19915,#19916,#19917,#19918,#19919,#19920,#19921,#19922,
#19923,#19924,#19925,#19926,#19927,#19928,#19929,#19930,#19931,#19932,#19933,
#19934,#19935,#19936),.UNSPECIFIED.,.F.,.F.,(6,1,1,1,1,1,1,1,1,1,1,1,1,
1,1,1,1,1,1,1,1,1,1,1,1,1,1,1,1,1,1,1,1,1,1,1,1,1,1,1,1,1,1,1,1,1,1,1,1,
1,1,1,1,1,1,1,1,1,1,1,1,1,1,1,1,1,1,1,1,6),(0.,0.0142857142857143,0.0285714285714286,
0.0428571428571429,0.0571428571428571,0.0714285714285714,0.0857142857142857,
0.1,0.114285714285714,0.128571428571429,0.142857142857143,0.157142857142857,
0.171428571428571,0.185714285714286,0.2,0.214285714285714,0.228571428571429,
0.242857142857143,0.257142857142857,0.271428571428571,0.285714285714286,
0.3,0.314285714285714,0.328571428571429,0.342857142857143,0.357142857142857,
0.371428571428571,0.385714285714286,0.4,0.414285714285714,0.428571428571429,
0.442857142857143,0.457142857142857,0.471428571428572,0.485714285714286,
0.5,0.514285714285714,0.528571428571429,0.542857142857143,0.557142857142857,
0.571428571428571,0.585714285714286,0.6,0.614285714285714,0.628571428571428,
0.642857142857142,0.657142857142857,0.671428571428571,0.685714285714285,
0.699999999999999,0.714285714285714,0.728571428571428,0.742857142857142,
0.757142857142856,0.771428571428571,0.785714285714285,0.799999999999999,
0.814285714285713,0.828571428571428,0.842857142857142,0.857142857142856,
0.87142857142857,0.885714285714284,0.899999999999999,0.914285714285713,
0.928571428571427,0.942857142857141,0.957142857142856,0.97142857142857,
1.),.UNSPECIFIED.);
#494=B_SPLINE_CURVE_WITH_KNOTS('',5,(#19937,#19938,#19939,#19940,#19941,
#19942,#19943,#19944,#19945,#19946,#19947,#19948,#19949,#19950,#19951,#19952,
#19953,#19954,#19955,#19956,#19957,#19958,#19959,#19960,#19961,#19962,#19963,
#19964,#19965,#19966,#19967,#19968,#19969,#19970,#19971,#19972,#19973,#19974,
#19975,#19976,#19977,#19978,#19979,#19980,#19981,#19982,#19983,#19984,#19985,
#19986,#19987,#19988,#19989,#19990,#19991,#19992,#19993,#19994,#19995,#19996,
#19997,#19998,#19999,#20000,#20001,#20002,#20003,#20004,#20005,#20006,#20007,
#20008,#20009,#20010),.UNSPECIFIED.,.F.,.F.,(6,1,1,1,1,1,1,1,1,1,1,1,1,
1,1,1,1,1,1,1,1,1,1,1,1,1,1,1,1,1,1,1,1,1,1,1,1,1,1,1,1,1,1,1,1,1,1,1,1,
1,1,1,1,1,1,1,1,1,1,1,1,1,1,1,1,1,1,1,1,6),(0.,0.0142857142857143,0.0285714285714286,
0.0428571428571429,0.0571428571428571,0.0714285714285714,0.0857142857142857,
0.1,0.114285714285714,0.128571428571429,0.142857142857143,0.157142857142857,
0.171428571428571,0.185714285714286,0.2,0.214285714285714,0.228571428571429,
0.242857142857143,0.257142857142857,0.271428571428571,0.285714285714286,
0.3,0.314285714285714,0.328571428571429,0.342857142857143,0.357142857142857,
0.371428571428571,0.385714285714286,0.4,0.414285714285714,0.428571428571429,
0.442857142857143,0.457142857142857,0.471428571428572,0.485714285714286,
0.5,0.514285714285714,0.528571428571429,0.542857142857143,0.557142857142857,
0.571428571428571,0.585714285714286,0.6,0.614285714285714,0.628571428571428,
0.642857142857142,0.657142857142857,0.671428571428571,0.685714285714285,
0.699999999999999,0.714285714285714,0.728571428571428,0.742857142857142,
0.757142857142856,0.771428571428571,0.785714285714285,0.799999999999999,
0.814285714285713,0.828571428571428,0.842857142857142,0.857142857142856,
0.87142857142857,0.885714285714284,0.899999999999999,0.914285714285713,
0.928571428571427,0.942857142857141,0.957142857142856,0.97142857142857,
1.),.UNSPECIFIED.);
#495=B_SPLINE_CURVE_WITH_KNOTS('',5,(#20162,#20163,#20164,#20165,#20166,
#20167,#20168,#20169,#20170,#20171,#20172,#20173,#20174,#20175,#20176,#20177,
#20178,#20179,#20180,#20181,#20182,#20183,#20184,#20185,#20186,#20187,#20188,
#20189,#20190,#20191,#20192,#20193,#20194,#20195,#20196,#20197,#20198,#20199,
#20200,#20201,#20202,#20203,#20204,#20205,#20206,#20207,#20208,#20209,#20210,
#20211,#20212,#20213,#20214,#20215,#20216,#20217,#20218,#20219,#20220,#20221,
#20222,#20223,#20224,#20225,#20226,#20227,#20228,#20229,#20230,#20231,#20232,
#20233,#20234,#20235),.UNSPECIFIED.,.F.,.F.,(6,1,1,1,1,1,1,1,1,1,1,1,1,
1,1,1,1,1,1,1,1,1,1,1,1,1,1,1,1,1,1,1,1,1,1,1,1,1,1,1,1,1,1,1,1,1,1,1,1,
1,1,1,1,1,1,1,1,1,1,1,1,1,1,1,1,1,1,1,1,6),(0.,0.0142857142857143,0.0285714285714286,
0.0428571428571429,0.0571428571428571,0.0714285714285714,0.0857142857142857,
0.1,0.114285714285714,0.128571428571429,0.142857142857143,0.157142857142857,
0.171428571428571,0.185714285714286,0.2,0.214285714285714,0.228571428571429,
0.242857142857143,0.257142857142857,0.271428571428571,0.285714285714286,
0.3,0.314285714285714,0.328571428571429,0.342857142857143,0.357142857142857,
0.371428571428571,0.385714285714286,0.4,0.414285714285714,0.428571428571429,
0.442857142857143,0.457142857142857,0.471428571428572,0.485714285714286,
0.5,0.514285714285714,0.528571428571429,0.542857142857143,0.557142857142857,
0.571428571428571,0.585714285714286,0.6,0.614285714285714,0.628571428571428,
0.642857142857142,0.657142857142857,0.671428571428571,0.685714285714285,
0.699999999999999,0.714285714285714,0.728571428571428,0.742857142857142,
0.757142857142856,0.771428571428571,0.785714285714285,0.799999999999999,
0.814285714285713,0.828571428571428,0.842857142857142,0.857142857142856,
0.87142857142857,0.885714285714284,0.899999999999999,0.914285714285713,
0.928571428571427,0.942857142857141,0.957142857142856,0.97142857142857,
1.),.UNSPECIFIED.);
#496=B_SPLINE_CURVE_WITH_KNOTS('',5,(#20237,#20238,#20239,#20240,#20241,
#20242,#20243,#20244,#20245,#20246,#20247,#20248,#20249,#20250,#20251,#20252,
#20253,#20254,#20255,#20256,#20257,#20258,#20259,#20260,#20261,#20262,#20263,
#20264,#20265,#20266,#20267,#20268,#20269,#20270,#20271,#20272,#20273,#20274,
#20275,#20276,#20277,#20278,#20279,#20280,#20281,#20282,#20283,#20284,#20285,
#20286,#20287,#20288,#20289,#20290,#20291,#20292,#20293,#20294,#20295,#20296,
#20297,#20298,#20299,#20300,#20301,#20302,#20303,#20304,#20305,#20306,#20307,
#20308,#20309,#20310,#20311),.UNSPECIFIED.,.F.,.F.,(6,1,1,1,1,1,1,1,1,1,
1,1,1,1,1,1,1,1,1,1,1,1,1,1,1,1,1,1,1,1,1,1,1,1,1,1,1,1,1,1,1,1,1,1,1,1,
1,1,1,1,1,1,1,1,1,1,1,1,1,1,1,1,1,1,1,1,1,1,1,1,6),(-1.,-0.985714285714284,
-0.97142857142857,-0.957142857142856,-0.942857142857141,-0.928571428571427,
-0.914285714285713,-0.899999999999999,-0.885714285714284,-0.87142857142857,
-0.857142857142856,-0.842857142857142,-0.828571428571428,-0.814285714285713,
-0.799999999999999,-0.785714285714285,-0.771428571428571,-0.757142857142856,
-0.742857142857142,-0.728571428571428,-0.714285714285714,-0.699999999999999,
-0.685714285714285,-0.671428571428571,-0.657142857142857,-0.642857142857142,
-0.628571428571428,-0.614285714285714,-0.6,-0.585714285714286,-0.571428571428571,
-0.557142857142857,-0.542857142857143,-0.528571428571429,-0.514285714285714,
-0.5,-0.485714285714286,-0.471428571428572,-0.457142857142857,-0.442857142857143,
-0.428571428571429,-0.414285714285714,-0.4,-0.385714285714286,-0.371428571428571,
-0.357142857142857,-0.342857142857143,-0.328571428571429,-0.314285714285714,
-0.3,-0.285714285714286,-0.271428571428571,-0.257142857142857,-0.242857142857143,
-0.228571428571429,-0.214285714285714,-0.2,-0.185714285714286,-0.171428571428571,
-0.157142857142857,-0.142857142857143,-0.128571428571429,-0.114285714285714,
-0.1,-0.0857142857142857,-0.0714285714285714,-0.0571428571428571,-0.0428571428571429,
-0.0285714285714286,-0.0142857142857143,0.),.UNSPECIFIED.);
#497=B_SPLINE_CURVE_WITH_KNOTS('',5,(#20469,#20470,#20471,#20472,#20473,
#20474,#20475,#20476,#20477,#20478,#20479,#20480,#20481,#20482,#20483,#20484,
#20485,#20486,#20487,#20488,#20489,#20490,#20491,#20492,#20493,#20494,#20495,
#20496,#20497,#20498,#20499,#20500,#20501,#20502,#20503,#20504,#20505,#20506,
#20507,#20508,#20509,#20510,#20511,#20512,#20513,#20514,#20515,#20516,#20517,
#20518,#20519,#20520,#20521,#20522,#20523,#20524,#20525,#20526,#20527,#20528,
#20529,#20530,#20531,#20532,#20533,#20534,#20535,#20536,#20537,#20538,#20539,
#20540,#20541,#20542),.UNSPECIFIED.,.F.,.F.,(6,1,1,1,1,1,1,1,1,1,1,1,1,
1,1,1,1,1,1,1,1,1,1,1,1,1,1,1,1,1,1,1,1,1,1,1,1,1,1,1,1,1,1,1,1,1,1,1,1,
1,1,1,1,1,1,1,1,1,1,1,1,1,1,1,1,1,1,1,1,6),(0.,0.0142857142857143,0.0285714285714286,
0.0428571428571429,0.0571428571428571,0.0714285714285714,0.0857142857142857,
0.1,0.114285714285714,0.128571428571429,0.142857142857143,0.157142857142857,
0.171428571428571,0.185714285714286,0.2,0.214285714285714,0.228571428571429,
0.242857142857143,0.257142857142857,0.271428571428571,0.285714285714286,
0.3,0.314285714285714,0.328571428571429,0.342857142857143,0.357142857142857,
0.371428571428571,0.385714285714286,0.4,0.414285714285714,0.428571428571429,
0.442857142857143,0.457142857142857,0.471428571428572,0.485714285714286,
0.5,0.514285714285714,0.528571428571429,0.542857142857143,0.557142857142857,
0.571428571428571,0.585714285714286,0.6,0.614285714285714,0.628571428571428,
0.642857142857142,0.657142857142857,0.671428571428571,0.685714285714285,
0.699999999999999,0.714285714285714,0.728571428571428,0.742857142857142,
0.757142857142856,0.771428571428571,0.785714285714285,0.799999999999999,
0.814285714285713,0.828571428571428,0.842857142857142,0.857142857142856,
0.87142857142857,0.885714285714284,0.899999999999999,0.914285714285713,
0.928571428571427,0.942857142857141,0.957142857142856,0.97142857142857,
1.),.UNSPECIFIED.);
#498=B_SPLINE_CURVE_WITH_KNOTS('',5,(#20543,#20544,#20545,#20546,#20547,
#20548,#20549,#20550,#20551,#20552,#20553,#20554,#20555,#20556,#20557,#20558,
#20559,#20560,#20561,#20562,#20563,#20564,#20565,#20566,#20567,#20568,#20569,
#20570,#20571,#20572,#20573,#20574,#20575,#20576,#20577,#20578,#20579,#20580,
#20581,#20582,#20583,#20584,#20585,#20586,#20587,#20588,#20589,#20590,#20591,
#20592,#20593,#20594,#20595,#20596,#20597,#20598,#20599,#20600,#20601,#20602,
#20603,#20604,#20605,#20606,#20607,#20608,#20609,#20610,#20611,#20612,#20613,
#20614,#20615,#20616),.UNSPECIFIED.,.F.,.F.,(6,1,1,1,1,1,1,1,1,1,1,1,1,
1,1,1,1,1,1,1,1,1,1,1,1,1,1,1,1,1,1,1,1,1,1,1,1,1,1,1,1,1,1,1,1,1,1,1,1,
1,1,1,1,1,1,1,1,1,1,1,1,1,1,1,1,1,1,1,1,6),(0.,0.0142857142857143,0.0285714285714286,
0.0428571428571429,0.0571428571428571,0.0714285714285714,0.0857142857142857,
0.1,0.114285714285714,0.128571428571429,0.142857142857143,0.157142857142857,
0.171428571428571,0.185714285714286,0.2,0.214285714285714,0.228571428571429,
0.242857142857143,0.257142857142857,0.271428571428571,0.285714285714286,
0.3,0.314285714285714,0.328571428571429,0.342857142857143,0.357142857142857,
0.371428571428571,0.385714285714286,0.4,0.414285714285714,0.428571428571429,
0.442857142857143,0.457142857142857,0.471428571428572,0.485714285714286,
0.5,0.514285714285714,0.528571428571429,0.542857142857143,0.557142857142857,
0.571428571428571,0.585714285714286,0.6,0.614285714285714,0.628571428571428,
0.642857142857142,0.657142857142857,0.671428571428571,0.685714285714285,
0.699999999999999,0.714285714285714,0.728571428571428,0.742857142857142,
0.757142857142856,0.771428571428571,0.785714285714285,0.799999999999999,
0.814285714285713,0.828571428571428,0.842857142857142,0.857142857142856,
0.87142857142857,0.885714285714284,0.899999999999999,0.914285714285713,
0.928571428571427,0.942857142857141,0.957142857142856,0.97142857142857,
1.),.UNSPECIFIED.);
#499=B_SPLINE_CURVE_WITH_KNOTS('',5,(#20768,#20769,#20770,#20771,#20772,
#20773,#20774,#20775,#20776,#20777,#20778,#20779,#20780,#20781,#20782,#20783,
#20784,#20785,#20786,#20787,#20788,#20789,#20790,#20791,#20792,#20793,#20794,
#20795,#20796,#20797,#20798,#20799,#20800,#20801,#20802,#20803,#20804,#20805,
#20806,#20807,#20808,#20809,#20810,#20811,#20812,#20813,#20814,#20815,#20816,
#20817,#20818,#20819,#20820,#20821,#20822,#20823,#20824,#20825,#20826,#20827,
#20828,#20829,#20830,#20831,#20832,#20833,#20834,#20835,#20836,#20837,#20838,
#20839,#20840,#20841),.UNSPECIFIED.,.F.,.F.,(6,1,1,1,1,1,1,1,1,1,1,1,1,
1,1,1,1,1,1,1,1,1,1,1,1,1,1,1,1,1,1,1,1,1,1,1,1,1,1,1,1,1,1,1,1,1,1,1,1,
1,1,1,1,1,1,1,1,1,1,1,1,1,1,1,1,1,1,1,1,6),(0.,0.0142857142857143,0.0285714285714286,
0.0428571428571429,0.0571428571428571,0.0714285714285714,0.0857142857142857,
0.1,0.114285714285714,0.128571428571429,0.142857142857143,0.157142857142857,
0.171428571428571,0.185714285714286,0.2,0.214285714285714,0.228571428571429,
0.242857142857143,0.257142857142857,0.271428571428571,0.285714285714286,
0.3,0.314285714285714,0.328571428571429,0.342857142857143,0.357142857142857,
0.371428571428571,0.385714285714286,0.4,0.414285714285714,0.428571428571429,
0.442857142857143,0.457142857142857,0.471428571428572,0.485714285714286,
0.5,0.514285714285714,0.528571428571429,0.542857142857143,0.557142857142857,
0.571428571428571,0.585714285714286,0.6,0.614285714285714,0.628571428571428,
0.642857142857142,0.657142857142857,0.671428571428571,0.685714285714285,
0.699999999999999,0.714285714285714,0.728571428571428,0.742857142857142,
0.757142857142856,0.771428571428571,0.785714285714285,0.799999999999999,
0.814285714285713,0.828571428571428,0.842857142857142,0.857142857142856,
0.87142857142857,0.885714285714284,0.899999999999999,0.914285714285713,
0.928571428571427,0.942857142857141,0.957142857142856,0.97142857142857,
1.),.UNSPECIFIED.);
#500=B_SPLINE_CURVE_WITH_KNOTS('',5,(#20843,#20844,#20845,#20846,#20847,
#20848,#20849,#20850,#20851,#20852,#20853,#20854,#20855,#20856,#20857,#20858,
#20859,#20860,#20861,#20862,#20863,#20864,#20865,#20866,#20867,#20868,#20869,
#20870,#20871,#20872,#20873,#20874,#20875,#20876,#20877,#20878,#20879,#20880,
#20881,#20882,#20883,#20884,#20885,#20886,#20887,#20888,#20889,#20890,#20891,
#20892,#20893,#20894,#20895,#20896,#20897,#20898,#20899,#20900,#20901,#20902,
#20903,#20904,#20905,#20906,#20907,#20908,#20909,#20910,#20911,#20912,#20913,
#20914,#20915,#20916,#20917),.UNSPECIFIED.,.F.,.F.,(6,1,1,1,1,1,1,1,1,1,
1,1,1,1,1,1,1,1,1,1,1,1,1,1,1,1,1,1,1,1,1,1,1,1,1,1,1,1,1,1,1,1,1,1,1,1,
1,1,1,1,1,1,1,1,1,1,1,1,1,1,1,1,1,1,1,1,1,1,1,1,6),(-1.,-0.985714285714284,
-0.97142857142857,-0.957142857142856,-0.942857142857141,-0.928571428571427,
-0.914285714285713,-0.899999999999999,-0.885714285714284,-0.87142857142857,
-0.857142857142856,-0.842857142857142,-0.828571428571428,-0.814285714285713,
-0.799999999999999,-0.785714285714285,-0.771428571428571,-0.757142857142856,
-0.742857142857142,-0.728571428571428,-0.714285714285714,-0.699999999999999,
-0.685714285714285,-0.671428571428571,-0.657142857142857,-0.642857142857142,
-0.628571428571428,-0.614285714285714,-0.6,-0.585714285714286,-0.571428571428571,
-0.557142857142857,-0.542857142857143,-0.528571428571429,-0.514285714285714,
-0.5,-0.485714285714286,-0.471428571428572,-0.457142857142857,-0.442857142857143,
-0.428571428571429,-0.414285714285714,-0.4,-0.385714285714286,-0.371428571428571,
-0.357142857142857,-0.342857142857143,-0.328571428571429,-0.314285714285714,
-0.3,-0.285714285714286,-0.271428571428571,-0.257142857142857,-0.242857142857143,
-0.228571428571429,-0.214285714285714,-0.2,-0.185714285714286,-0.171428571428571,
-0.157142857142857,-0.142857142857143,-0.128571428571429,-0.114285714285714,
-0.1,-0.0857142857142857,-0.0714285714285714,-0.0571428571428571,-0.0428571428571429,
-0.0285714285714286,-0.0142857142857143,0.),.UNSPECIFIED.);
#501=B_SPLINE_CURVE_WITH_KNOTS('',5,(#21075,#21076,#21077,#21078,#21079,
#21080,#21081,#21082,#21083,#21084,#21085,#21086,#21087,#21088,#21089,#21090,
#21091,#21092,#21093,#21094,#21095,#21096,#21097,#21098,#21099,#21100,#21101,
#21102,#21103,#21104,#21105,#21106,#21107,#21108,#21109,#21110,#21111,#21112,
#21113,#21114,#21115,#21116,#21117,#21118,#21119,#21120,#21121,#21122,#21123,
#21124,#21125,#21126,#21127,#21128,#21129,#21130,#21131,#21132,#21133,#21134,
#21135,#21136,#21137,#21138,#21139,#21140,#21141,#21142,#21143,#21144,#21145,
#21146,#21147,#21148),.UNSPECIFIED.,.F.,.F.,(6,1,1,1,1,1,1,1,1,1,1,1,1,
1,1,1,1,1,1,1,1,1,1,1,1,1,1,1,1,1,1,1,1,1,1,1,1,1,1,1,1,1,1,1,1,1,1,1,1,
1,1,1,1,1,1,1,1,1,1,1,1,1,1,1,1,1,1,1,1,6),(0.,0.0142857142857143,0.0285714285714286,
0.0428571428571429,0.0571428571428571,0.0714285714285714,0.0857142857142857,
0.1,0.114285714285714,0.128571428571429,0.142857142857143,0.157142857142857,
0.171428571428571,0.185714285714286,0.2,0.214285714285714,0.228571428571429,
0.242857142857143,0.257142857142857,0.271428571428571,0.285714285714286,
0.3,0.314285714285714,0.328571428571429,0.342857142857143,0.357142857142857,
0.371428571428571,0.385714285714286,0.4,0.414285714285714,0.428571428571429,
0.442857142857143,0.457142857142857,0.471428571428572,0.485714285714286,
0.5,0.514285714285714,0.528571428571429,0.542857142857143,0.557142857142857,
0.571428571428571,0.585714285714286,0.6,0.614285714285714,0.628571428571428,
0.642857142857142,0.657142857142857,0.671428571428571,0.685714285714285,
0.699999999999999,0.714285714285714,0.728571428571428,0.742857142857142,
0.757142857142856,0.771428571428571,0.785714285714285,0.799999999999999,
0.814285714285713,0.828571428571428,0.842857142857142,0.857142857142856,
0.87142857142857,0.885714285714284,0.899999999999999,0.914285714285713,
0.928571428571427,0.942857142857141,0.957142857142856,0.97142857142857,
1.),.UNSPECIFIED.);
#502=B_SPLINE_CURVE_WITH_KNOTS('',5,(#21149,#21150,#21151,#21152,#21153,
#21154,#21155,#21156,#21157,#21158,#21159,#21160,#21161,#21162,#21163,#21164,
#21165,#21166,#21167,#21168,#21169,#21170,#21171,#21172,#21173,#21174,#21175,
#21176,#21177,#21178,#21179,#21180,#21181,#21182,#21183,#21184,#21185,#21186,
#21187,#21188,#21189,#21190,#21191,#21192,#21193,#21194,#21195,#21196,#21197,
#21198,#21199,#21200,#21201,#21202,#21203,#21204,#21205,#21206,#21207,#21208,
#21209,#21210,#21211,#21212,#21213,#21214,#21215,#21216,#21217,#21218,#21219,
#21220,#21221,#21222),.UNSPECIFIED.,.F.,.F.,(6,1,1,1,1,1,1,1,1,1,1,1,1,
1,1,1,1,1,1,1,1,1,1,1,1,1,1,1,1,1,1,1,1,1,1,1,1,1,1,1,1,1,1,1,1,1,1,1,1,
1,1,1,1,1,1,1,1,1,1,1,1,1,1,1,1,1,1,1,1,6),(0.,0.0142857142857143,0.0285714285714286,
0.0428571428571429,0.0571428571428571,0.0714285714285714,0.0857142857142857,
0.1,0.114285714285714,0.128571428571429,0.142857142857143,0.157142857142857,
0.171428571428571,0.185714285714286,0.2,0.214285714285714,0.228571428571429,
0.242857142857143,0.257142857142857,0.271428571428571,0.285714285714286,
0.3,0.314285714285714,0.328571428571429,0.342857142857143,0.357142857142857,
0.371428571428571,0.385714285714286,0.4,0.414285714285714,0.428571428571429,
0.442857142857143,0.457142857142857,0.471428571428572,0.485714285714286,
0.5,0.514285714285714,0.528571428571429,0.542857142857143,0.557142857142857,
0.571428571428571,0.585714285714286,0.6,0.614285714285714,0.628571428571428,
0.642857142857142,0.657142857142857,0.671428571428571,0.685714285714285,
0.699999999999999,0.714285714285714,0.728571428571428,0.742857142857142,
0.757142857142856,0.771428571428571,0.785714285714285,0.799999999999999,
0.814285714285713,0.828571428571428,0.842857142857142,0.857142857142856,
0.87142857142857,0.885714285714284,0.899999999999999,0.914285714285713,
0.928571428571427,0.942857142857141,0.957142857142856,0.97142857142857,
1.),.UNSPECIFIED.);
#503=B_SPLINE_CURVE_WITH_KNOTS('',5,(#21374,#21375,#21376,#21377,#21378,
#21379,#21380,#21381,#21382,#21383,#21384,#21385,#21386,#21387,#21388,#21389,
#21390,#21391,#21392,#21393,#21394,#21395,#21396,#21397,#21398,#21399,#21400,
#21401,#21402,#21403,#21404,#21405,#21406,#21407,#21408,#21409,#21410,#21411,
#21412,#21413,#21414,#21415,#21416,#21417,#21418,#21419,#21420,#21421,#21422,
#21423,#21424,#21425,#21426,#21427,#21428,#21429,#21430,#21431,#21432,#21433,
#21434,#21435,#21436,#21437,#21438,#21439,#21440,#21441,#21442,#21443,#21444,
#21445,#21446,#21447),.UNSPECIFIED.,.F.,.F.,(6,1,1,1,1,1,1,1,1,1,1,1,1,
1,1,1,1,1,1,1,1,1,1,1,1,1,1,1,1,1,1,1,1,1,1,1,1,1,1,1,1,1,1,1,1,1,1,1,1,
1,1,1,1,1,1,1,1,1,1,1,1,1,1,1,1,1,1,1,1,6),(0.,0.0142857142857143,0.0285714285714286,
0.0428571428571429,0.0571428571428571,0.0714285714285714,0.0857142857142857,
0.1,0.114285714285714,0.128571428571429,0.142857142857143,0.157142857142857,
0.171428571428571,0.185714285714286,0.2,0.214285714285714,0.228571428571429,
0.242857142857143,0.257142857142857,0.271428571428571,0.285714285714286,
0.3,0.314285714285714,0.328571428571429,0.342857142857143,0.357142857142857,
0.371428571428571,0.385714285714286,0.4,0.414285714285714,0.428571428571429,
0.442857142857143,0.457142857142857,0.471428571428572,0.485714285714286,
0.5,0.514285714285714,0.528571428571429,0.542857142857143,0.557142857142857,
0.571428571428571,0.585714285714286,0.6,0.614285714285714,0.628571428571428,
0.642857142857142,0.657142857142857,0.671428571428571,0.685714285714285,
0.699999999999999,0.714285714285714,0.728571428571428,0.742857142857142,
0.757142857142856,0.771428571428571,0.785714285714285,0.799999999999999,
0.814285714285713,0.828571428571428,0.842857142857142,0.857142857142856,
0.87142857142857,0.885714285714284,0.899999999999999,0.914285714285713,
0.928571428571427,0.942857142857141,0.957142857142856,0.97142857142857,
1.),.UNSPECIFIED.);
#504=B_SPLINE_CURVE_WITH_KNOTS('',5,(#21449,#21450,#21451,#21452,#21453,
#21454,#21455,#21456,#21457,#21458,#21459,#21460,#21461,#21462,#21463,#21464,
#21465,#21466,#21467,#21468,#21469,#21470,#21471,#21472,#21473,#21474,#21475,
#21476,#21477,#21478,#21479,#21480,#21481,#21482,#21483,#21484,#21485,#21486,
#21487,#21488,#21489,#21490,#21491,#21492,#21493,#21494,#21495,#21496,#21497,
#21498,#21499,#21500,#21501,#21502,#21503,#21504,#21505,#21506,#21507,#21508,
#21509,#21510,#21511,#21512,#21513,#21514,#21515,#21516,#21517,#21518,#21519,
#21520,#21521,#21522,#21523),.UNSPECIFIED.,.F.,.F.,(6,1,1,1,1,1,1,1,1,1,
1,1,1,1,1,1,1,1,1,1,1,1,1,1,1,1,1,1,1,1,1,1,1,1,1,1,1,1,1,1,1,1,1,1,1,1,
1,1,1,1,1,1,1,1,1,1,1,1,1,1,1,1,1,1,1,1,1,1,1,1,6),(-1.,-0.985714285714284,
-0.97142857142857,-0.957142857142856,-0.942857142857141,-0.928571428571427,
-0.914285714285713,-0.899999999999999,-0.885714285714284,-0.87142857142857,
-0.857142857142856,-0.842857142857142,-0.828571428571428,-0.814285714285713,
-0.799999999999999,-0.785714285714285,-0.771428571428571,-0.757142857142856,
-0.742857142857142,-0.728571428571428,-0.714285714285714,-0.699999999999999,
-0.685714285714285,-0.671428571428571,-0.657142857142857,-0.642857142857142,
-0.628571428571428,-0.614285714285714,-0.6,-0.585714285714286,-0.571428571428571,
-0.557142857142857,-0.542857142857143,-0.528571428571429,-0.514285714285714,
-0.5,-0.485714285714286,-0.471428571428572,-0.457142857142857,-0.442857142857143,
-0.428571428571429,-0.414285714285714,-0.4,-0.385714285714286,-0.371428571428571,
-0.357142857142857,-0.342857142857143,-0.328571428571429,-0.314285714285714,
-0.3,-0.285714285714286,-0.271428571428571,-0.257142857142857,-0.242857142857143,
-0.228571428571429,-0.214285714285714,-0.2,-0.185714285714286,-0.171428571428571,
-0.157142857142857,-0.142857142857143,-0.128571428571429,-0.114285714285714,
-0.1,-0.0857142857142857,-0.0714285714285714,-0.0571428571428571,-0.0428571428571429,
-0.0285714285714286,-0.0142857142857143,0.),.UNSPECIFIED.);
#505=B_SPLINE_CURVE_WITH_KNOTS('',5,(#21681,#21682,#21683,#21684,#21685,
#21686,#21687,#21688,#21689,#21690,#21691,#21692,#21693,#21694,#21695,#21696,
#21697,#21698,#21699,#21700,#21701,#21702,#21703,#21704,#21705,#21706,#21707,
#21708,#21709,#21710,#21711,#21712,#21713,#21714,#21715,#21716,#21717,#21718,
#21719,#21720,#21721,#21722,#21723,#21724,#21725,#21726,#21727,#21728,#21729,
#21730,#21731,#21732,#21733,#21734,#21735,#21736,#21737,#21738,#21739,#21740,
#21741,#21742,#21743,#21744,#21745,#21746,#21747,#21748,#21749,#21750,#21751,
#21752,#21753,#21754),.UNSPECIFIED.,.F.,.F.,(6,1,1,1,1,1,1,1,1,1,1,1,1,
1,1,1,1,1,1,1,1,1,1,1,1,1,1,1,1,1,1,1,1,1,1,1,1,1,1,1,1,1,1,1,1,1,1,1,1,
1,1,1,1,1,1,1,1,1,1,1,1,1,1,1,1,1,1,1,1,6),(0.,0.0142857142857143,0.0285714285714286,
0.0428571428571429,0.0571428571428571,0.0714285714285714,0.0857142857142857,
0.1,0.114285714285714,0.128571428571429,0.142857142857143,0.157142857142857,
0.171428571428571,0.185714285714286,0.2,0.214285714285714,0.228571428571429,
0.242857142857143,0.257142857142857,0.271428571428571,0.285714285714286,
0.3,0.314285714285714,0.328571428571429,0.342857142857143,0.357142857142857,
0.371428571428571,0.385714285714286,0.4,0.414285714285714,0.428571428571429,
0.442857142857143,0.457142857142857,0.471428571428572,0.485714285714286,
0.5,0.514285714285714,0.528571428571429,0.542857142857143,0.557142857142857,
0.571428571428571,0.585714285714286,0.6,0.614285714285714,0.628571428571428,
0.642857142857142,0.657142857142857,0.671428571428571,0.685714285714285,
0.699999999999999,0.714285714285714,0.728571428571428,0.742857142857142,
0.757142857142856,0.771428571428571,0.785714285714285,0.799999999999999,
0.814285714285713,0.828571428571428,0.842857142857142,0.857142857142856,
0.87142857142857,0.885714285714284,0.899999999999999,0.914285714285713,
0.928571428571427,0.942857142857141,0.957142857142856,0.97142857142857,
1.),.UNSPECIFIED.);
#506=B_SPLINE_CURVE_WITH_KNOTS('',5,(#21755,#21756,#21757,#21758,#21759,
#21760,#21761,#21762,#21763,#21764,#21765,#21766,#21767,#21768,#21769,#21770,
#21771,#21772,#21773,#21774,#21775,#21776,#21777,#21778,#21779,#21780,#21781,
#21782,#21783,#21784,#21785,#21786,#21787,#21788,#21789,#21790,#21791,#21792,
#21793,#21794,#21795,#21796,#21797,#21798,#21799,#21800,#21801,#21802,#21803,
#21804,#21805,#21806,#21807,#21808,#21809,#21810,#21811,#21812,#21813,#21814,
#21815,#21816,#21817,#21818,#21819,#21820,#21821,#21822,#21823,#21824,#21825,
#21826,#21827,#21828),.UNSPECIFIED.,.F.,.F.,(6,1,1,1,1,1,1,1,1,1,1,1,1,
1,1,1,1,1,1,1,1,1,1,1,1,1,1,1,1,1,1,1,1,1,1,1,1,1,1,1,1,1,1,1,1,1,1,1,1,
1,1,1,1,1,1,1,1,1,1,1,1,1,1,1,1,1,1,1,1,6),(0.,0.0142857142857143,0.0285714285714286,
0.0428571428571429,0.0571428571428571,0.0714285714285714,0.0857142857142857,
0.1,0.114285714285714,0.128571428571429,0.142857142857143,0.157142857142857,
0.171428571428571,0.185714285714286,0.2,0.214285714285714,0.228571428571429,
0.242857142857143,0.257142857142857,0.271428571428571,0.285714285714286,
0.3,0.314285714285714,0.328571428571429,0.342857142857143,0.357142857142857,
0.371428571428571,0.385714285714286,0.4,0.414285714285714,0.428571428571429,
0.442857142857143,0.457142857142857,0.471428571428572,0.485714285714286,
0.5,0.514285714285714,0.528571428571429,0.542857142857143,0.557142857142857,
0.571428571428571,0.585714285714286,0.6,0.614285714285714,0.628571428571428,
0.642857142857142,0.657142857142857,0.671428571428571,0.685714285714285,
0.699999999999999,0.714285714285714,0.728571428571428,0.742857142857142,
0.757142857142856,0.771428571428571,0.785714285714285,0.799999999999999,
0.814285714285713,0.828571428571428,0.842857142857142,0.857142857142856,
0.87142857142857,0.885714285714284,0.899999999999999,0.914285714285713,
0.928571428571427,0.942857142857141,0.957142857142856,0.97142857142857,
1.),.UNSPECIFIED.);
#507=B_SPLINE_CURVE_WITH_KNOTS('',5,(#21980,#21981,#21982,#21983,#21984,
#21985,#21986,#21987,#21988,#21989,#21990,#21991,#21992,#21993,#21994,#21995,
#21996,#21997,#21998,#21999,#22000,#22001,#22002,#22003,#22004,#22005,#22006,
#22007,#22008,#22009,#22010,#22011,#22012,#22013,#22014,#22015,#22016,#22017,
#22018,#22019,#22020,#22021,#22022,#22023,#22024,#22025,#22026,#22027,#22028,
#22029,#22030,#22031,#22032,#22033,#22034,#22035,#22036,#22037,#22038,#22039,
#22040,#22041,#22042,#22043,#22044,#22045,#22046,#22047,#22048,#22049,#22050,
#22051,#22052,#22053),.UNSPECIFIED.,.F.,.F.,(6,1,1,1,1,1,1,1,1,1,1,1,1,
1,1,1,1,1,1,1,1,1,1,1,1,1,1,1,1,1,1,1,1,1,1,1,1,1,1,1,1,1,1,1,1,1,1,1,1,
1,1,1,1,1,1,1,1,1,1,1,1,1,1,1,1,1,1,1,1,6),(0.,0.0142857142857143,0.0285714285714286,
0.0428571428571429,0.0571428571428571,0.0714285714285714,0.0857142857142857,
0.1,0.114285714285714,0.128571428571429,0.142857142857143,0.157142857142857,
0.171428571428571,0.185714285714286,0.2,0.214285714285714,0.228571428571429,
0.242857142857143,0.257142857142857,0.271428571428571,0.285714285714286,
0.3,0.314285714285714,0.328571428571429,0.342857142857143,0.357142857142857,
0.371428571428571,0.385714285714286,0.4,0.414285714285714,0.428571428571429,
0.442857142857143,0.457142857142857,0.471428571428572,0.485714285714286,
0.5,0.514285714285714,0.528571428571429,0.542857142857143,0.557142857142857,
0.571428571428571,0.585714285714286,0.6,0.614285714285714,0.628571428571428,
0.642857142857142,0.657142857142857,0.671428571428571,0.685714285714285,
0.699999999999999,0.714285714285714,0.728571428571428,0.742857142857142,
0.757142857142856,0.771428571428571,0.785714285714285,0.799999999999999,
0.814285714285713,0.828571428571428,0.842857142857142,0.857142857142856,
0.87142857142857,0.885714285714284,0.899999999999999,0.914285714285713,
0.928571428571427,0.942857142857141,0.957142857142856,0.97142857142857,
1.),.UNSPECIFIED.);
#508=B_SPLINE_CURVE_WITH_KNOTS('',5,(#22055,#22056,#22057,#22058,#22059,
#22060,#22061,#22062,#22063,#22064,#22065,#22066,#22067,#22068,#22069,#22070,
#22071,#22072,#22073,#22074,#22075,#22076,#22077,#22078,#22079,#22080,#22081,
#22082,#22083,#22084,#22085,#22086,#22087,#22088,#22089,#22090,#22091,#22092,
#22093,#22094,#22095,#22096,#22097,#22098,#22099,#22100,#22101,#22102,#22103,
#22104,#22105,#22106,#22107,#22108,#22109,#22110,#22111,#22112,#22113,#22114,
#22115,#22116,#22117,#22118,#22119,#22120,#22121,#22122,#22123,#22124,#22125,
#22126,#22127,#22128,#22129),.UNSPECIFIED.,.F.,.F.,(6,1,1,1,1,1,1,1,1,1,
1,1,1,1,1,1,1,1,1,1,1,1,1,1,1,1,1,1,1,1,1,1,1,1,1,1,1,1,1,1,1,1,1,1,1,1,
1,1,1,1,1,1,1,1,1,1,1,1,1,1,1,1,1,1,1,1,1,1,1,1,6),(-1.,-0.985714285714284,
-0.97142857142857,-0.957142857142856,-0.942857142857141,-0.928571428571427,
-0.914285714285713,-0.899999999999999,-0.885714285714284,-0.87142857142857,
-0.857142857142856,-0.842857142857142,-0.828571428571428,-0.814285714285713,
-0.799999999999999,-0.785714285714285,-0.771428571428571,-0.757142857142856,
-0.742857142857142,-0.728571428571428,-0.714285714285714,-0.699999999999999,
-0.685714285714285,-0.671428571428571,-0.657142857142857,-0.642857142857142,
-0.628571428571428,-0.614285714285714,-0.6,-0.585714285714286,-0.571428571428571,
-0.557142857142857,-0.542857142857143,-0.528571428571429,-0.514285714285714,
-0.5,-0.485714285714286,-0.471428571428572,-0.457142857142857,-0.442857142857143,
-0.428571428571429,-0.414285714285714,-0.4,-0.385714285714286,-0.371428571428571,
-0.357142857142857,-0.342857142857143,-0.328571428571429,-0.314285714285714,
-0.3,-0.285714285714286,-0.271428571428571,-0.257142857142857,-0.242857142857143,
-0.228571428571429,-0.214285714285714,-0.2,-0.185714285714286,-0.171428571428571,
-0.157142857142857,-0.142857142857143,-0.128571428571429,-0.114285714285714,
-0.1,-0.0857142857142857,-0.0714285714285714,-0.0571428571428571,-0.0428571428571429,
-0.0285714285714286,-0.0142857142857143,0.),.UNSPECIFIED.);
#509=B_SPLINE_CURVE_WITH_KNOTS('',5,(#22287,#22288,#22289,#22290,#22291,
#22292,#22293,#22294,#22295,#22296,#22297,#22298,#22299,#22300,#22301,#22302,
#22303,#22304,#22305,#22306,#22307,#22308,#22309,#22310,#22311,#22312,#22313,
#22314,#22315,#22316,#22317,#22318,#22319,#22320,#22321,#22322,#22323,#22324,
#22325,#22326,#22327,#22328,#22329,#22330,#22331,#22332,#22333,#22334,#22335,
#22336,#22337,#22338,#22339,#22340,#22341,#22342,#22343,#22344,#22345,#22346,
#22347,#22348,#22349,#22350,#22351,#22352,#22353,#22354,#22355,#22356,#22357,
#22358,#22359,#22360),.UNSPECIFIED.,.F.,.F.,(6,1,1,1,1,1,1,1,1,1,1,1,1,
1,1,1,1,1,1,1,1,1,1,1,1,1,1,1,1,1,1,1,1,1,1,1,1,1,1,1,1,1,1,1,1,1,1,1,1,
1,1,1,1,1,1,1,1,1,1,1,1,1,1,1,1,1,1,1,1,6),(0.,0.0142857142857143,0.0285714285714286,
0.0428571428571429,0.0571428571428571,0.0714285714285714,0.0857142857142857,
0.1,0.114285714285714,0.128571428571429,0.142857142857143,0.157142857142857,
0.171428571428571,0.185714285714286,0.2,0.214285714285714,0.228571428571429,
0.242857142857143,0.257142857142857,0.271428571428571,0.285714285714286,
0.3,0.314285714285714,0.328571428571429,0.342857142857143,0.357142857142857,
0.371428571428571,0.385714285714286,0.4,0.414285714285714,0.428571428571429,
0.442857142857143,0.457142857142857,0.471428571428572,0.485714285714286,
0.5,0.514285714285714,0.528571428571429,0.542857142857143,0.557142857142857,
0.571428571428571,0.585714285714286,0.6,0.614285714285714,0.628571428571428,
0.642857142857142,0.657142857142857,0.671428571428571,0.685714285714285,
0.699999999999999,0.714285714285714,0.728571428571428,0.742857142857142,
0.757142857142856,0.771428571428571,0.785714285714285,0.799999999999999,
0.814285714285713,0.828571428571428,0.842857142857142,0.857142857142856,
0.87142857142857,0.885714285714284,0.899999999999999,0.914285714285713,
0.928571428571427,0.942857142857141,0.957142857142856,0.97142857142857,
1.),.UNSPECIFIED.);
#510=B_SPLINE_CURVE_WITH_KNOTS('',5,(#22361,#22362,#22363,#22364,#22365,
#22366,#22367,#22368,#22369,#22370,#22371,#22372,#22373,#22374,#22375,#22376,
#22377,#22378,#22379,#22380,#22381,#22382,#22383,#22384,#22385,#22386,#22387,
#22388,#22389,#22390,#22391,#22392,#22393,#22394,#22395,#22396,#22397,#22398,
#22399,#22400,#22401,#22402,#22403,#22404,#22405,#22406,#22407,#22408,#22409,
#22410,#22411,#22412,#22413,#22414,#22415,#22416,#22417,#22418,#22419,#22420,
#22421,#22422,#22423,#22424,#22425,#22426,#22427,#22428,#22429,#22430,#22431,
#22432,#22433,#22434),.UNSPECIFIED.,.F.,.F.,(6,1,1,1,1,1,1,1,1,1,1,1,1,
1,1,1,1,1,1,1,1,1,1,1,1,1,1,1,1,1,1,1,1,1,1,1,1,1,1,1,1,1,1,1,1,1,1,1,1,
1,1,1,1,1,1,1,1,1,1,1,1,1,1,1,1,1,1,1,1,6),(0.,0.0142857142857143,0.0285714285714286,
0.0428571428571429,0.0571428571428571,0.0714285714285714,0.0857142857142857,
0.1,0.114285714285714,0.128571428571429,0.142857142857143,0.157142857142857,
0.171428571428571,0.185714285714286,0.2,0.214285714285714,0.228571428571429,
0.242857142857143,0.257142857142857,0.271428571428571,0.285714285714286,
0.3,0.314285714285714,0.328571428571429,0.342857142857143,0.357142857142857,
0.371428571428571,0.385714285714286,0.4,0.414285714285714,0.428571428571429,
0.442857142857143,0.457142857142857,0.471428571428572,0.485714285714286,
0.5,0.514285714285714,0.528571428571429,0.542857142857143,0.557142857142857,
0.571428571428571,0.585714285714286,0.6,0.614285714285714,0.628571428571428,
0.642857142857142,0.657142857142857,0.671428571428571,0.685714285714285,
0.699999999999999,0.714285714285714,0.728571428571428,0.742857142857142,
0.757142857142856,0.771428571428571,0.785714285714285,0.799999999999999,
0.814285714285713,0.828571428571428,0.842857142857142,0.857142857142856,
0.87142857142857,0.885714285714284,0.899999999999999,0.914285714285713,
0.928571428571427,0.942857142857141,0.957142857142856,0.97142857142857,
1.),.UNSPECIFIED.);
#511=B_SPLINE_CURVE_WITH_KNOTS('',5,(#22586,#22587,#22588,#22589,#22590,
#22591,#22592,#22593,#22594,#22595,#22596,#22597,#22598,#22599,#22600,#22601,
#22602,#22603,#22604,#22605,#22606,#22607,#22608,#22609,#22610,#22611,#22612,
#22613,#22614,#22615,#22616,#22617,#22618,#22619,#22620,#22621,#22622,#22623,
#22624,#22625,#22626,#22627,#22628,#22629,#22630,#22631,#22632,#22633,#22634,
#22635,#22636,#22637,#22638,#22639,#22640,#22641,#22642,#22643,#22644,#22645,
#22646,#22647,#22648,#22649,#22650,#22651,#22652,#22653,#22654,#22655,#22656,
#22657,#22658,#22659),.UNSPECIFIED.,.F.,.F.,(6,1,1,1,1,1,1,1,1,1,1,1,1,
1,1,1,1,1,1,1,1,1,1,1,1,1,1,1,1,1,1,1,1,1,1,1,1,1,1,1,1,1,1,1,1,1,1,1,1,
1,1,1,1,1,1,1,1,1,1,1,1,1,1,1,1,1,1,1,1,6),(0.,0.0142857142857143,0.0285714285714286,
0.0428571428571429,0.0571428571428571,0.0714285714285714,0.0857142857142857,
0.1,0.114285714285714,0.128571428571429,0.142857142857143,0.157142857142857,
0.171428571428571,0.185714285714286,0.2,0.214285714285714,0.228571428571429,
0.242857142857143,0.257142857142857,0.271428571428571,0.285714285714286,
0.3,0.314285714285714,0.328571428571429,0.342857142857143,0.357142857142857,
0.371428571428571,0.385714285714286,0.4,0.414285714285714,0.428571428571429,
0.442857142857143,0.457142857142857,0.471428571428572,0.485714285714286,
0.5,0.514285714285714,0.528571428571429,0.542857142857143,0.557142857142857,
0.571428571428571,0.585714285714286,0.6,0.614285714285714,0.628571428571428,
0.642857142857142,0.657142857142857,0.671428571428571,0.685714285714285,
0.699999999999999,0.714285714285714,0.728571428571428,0.742857142857142,
0.757142857142856,0.771428571428571,0.785714285714285,0.799999999999999,
0.814285714285713,0.828571428571428,0.842857142857142,0.857142857142856,
0.87142857142857,0.885714285714284,0.899999999999999,0.914285714285713,
0.928571428571427,0.942857142857141,0.957142857142856,0.97142857142857,
1.),.UNSPECIFIED.);
#512=B_SPLINE_CURVE_WITH_KNOTS('',5,(#22661,#22662,#22663,#22664,#22665,
#22666,#22667,#22668,#22669,#22670,#22671,#22672,#22673,#22674,#22675,#22676,
#22677,#22678,#22679,#22680,#22681,#22682,#22683,#22684,#22685,#22686,#22687,
#22688,#22689,#22690,#22691,#22692,#22693,#22694,#22695,#22696,#22697,#22698,
#22699,#22700,#22701,#22702,#22703,#22704,#22705,#22706,#22707,#22708,#22709,
#22710,#22711,#22712,#22713,#22714,#22715,#22716,#22717,#22718,#22719,#22720,
#22721,#22722,#22723,#22724,#22725,#22726,#22727,#22728,#22729,#22730,#22731,
#22732,#22733,#22734,#22735),.UNSPECIFIED.,.F.,.F.,(6,1,1,1,1,1,1,1,1,1,
1,1,1,1,1,1,1,1,1,1,1,1,1,1,1,1,1,1,1,1,1,1,1,1,1,1,1,1,1,1,1,1,1,1,1,1,
1,1,1,1,1,1,1,1,1,1,1,1,1,1,1,1,1,1,1,1,1,1,1,1,6),(-1.,-0.985714285714284,
-0.97142857142857,-0.957142857142856,-0.942857142857141,-0.928571428571427,
-0.914285714285713,-0.899999999999999,-0.885714285714284,-0.87142857142857,
-0.857142857142856,-0.842857142857142,-0.828571428571428,-0.814285714285713,
-0.799999999999999,-0.785714285714285,-0.771428571428571,-0.757142857142856,
-0.742857142857142,-0.728571428571428,-0.714285714285714,-0.699999999999999,
-0.685714285714285,-0.671428571428571,-0.657142857142857,-0.642857142857142,
-0.628571428571428,-0.614285714285714,-0.6,-0.585714285714286,-0.571428571428571,
-0.557142857142857,-0.542857142857143,-0.528571428571429,-0.514285714285714,
-0.5,-0.485714285714286,-0.471428571428572,-0.457142857142857,-0.442857142857143,
-0.428571428571429,-0.414285714285714,-0.4,-0.385714285714286,-0.371428571428571,
-0.357142857142857,-0.342857142857143,-0.328571428571429,-0.314285714285714,
-0.3,-0.285714285714286,-0.271428571428571,-0.257142857142857,-0.242857142857143,
-0.228571428571429,-0.214285714285714,-0.2,-0.185714285714286,-0.171428571428571,
-0.157142857142857,-0.142857142857143,-0.128571428571429,-0.114285714285714,
-0.1,-0.0857142857142857,-0.0714285714285714,-0.0571428571428571,-0.0428571428571429,
-0.0285714285714286,-0.0142857142857143,0.),.UNSPECIFIED.);
#513=B_SPLINE_CURVE_WITH_KNOTS('',5,(#22893,#22894,#22895,#22896,#22897,
#22898,#22899,#22900,#22901,#22902,#22903,#22904,#22905,#22906,#22907,#22908,
#22909,#22910,#22911,#22912,#22913,#22914,#22915,#22916,#22917,#22918,#22919,
#22920,#22921,#22922,#22923,#22924,#22925,#22926,#22927,#22928,#22929,#22930,
#22931,#22932,#22933,#22934,#22935,#22936,#22937,#22938,#22939,#22940,#22941,
#22942,#22943,#22944,#22945,#22946,#22947,#22948,#22949,#22950,#22951,#22952,
#22953,#22954,#22955,#22956,#22957,#22958,#22959,#22960,#22961,#22962,#22963,
#22964,#22965,#22966),.UNSPECIFIED.,.F.,.F.,(6,1,1,1,1,1,1,1,1,1,1,1,1,
1,1,1,1,1,1,1,1,1,1,1,1,1,1,1,1,1,1,1,1,1,1,1,1,1,1,1,1,1,1,1,1,1,1,1,1,
1,1,1,1,1,1,1,1,1,1,1,1,1,1,1,1,1,1,1,1,6),(0.,0.0142857142857143,0.0285714285714286,
0.0428571428571429,0.0571428571428571,0.0714285714285714,0.0857142857142857,
0.1,0.114285714285714,0.128571428571429,0.142857142857143,0.157142857142857,
0.171428571428571,0.185714285714286,0.2,0.214285714285714,0.228571428571429,
0.242857142857143,0.257142857142857,0.271428571428571,0.285714285714286,
0.3,0.314285714285714,0.328571428571429,0.342857142857143,0.357142857142857,
0.371428571428571,0.385714285714286,0.4,0.414285714285714,0.428571428571429,
0.442857142857143,0.457142857142857,0.471428571428572,0.485714285714286,
0.5,0.514285714285714,0.528571428571429,0.542857142857143,0.557142857142857,
0.571428571428571,0.585714285714286,0.6,0.614285714285714,0.628571428571428,
0.642857142857142,0.657142857142857,0.671428571428571,0.685714285714285,
0.699999999999999,0.714285714285714,0.728571428571428,0.742857142857142,
0.757142857142856,0.771428571428571,0.785714285714285,0.799999999999999,
0.814285714285713,0.828571428571428,0.842857142857142,0.857142857142856,
0.87142857142857,0.885714285714284,0.899999999999999,0.914285714285713,
0.928571428571427,0.942857142857141,0.957142857142856,0.97142857142857,
1.),.UNSPECIFIED.);
#514=B_SPLINE_CURVE_WITH_KNOTS('',5,(#22967,#22968,#22969,#22970,#22971,
#22972,#22973,#22974,#22975,#22976,#22977,#22978,#22979,#22980,#22981,#22982,
#22983,#22984,#22985,#22986,#22987,#22988,#22989,#22990,#22991,#22992,#22993,
#22994,#22995,#22996,#22997,#22998,#22999,#23000,#23001,#23002,#23003,#23004,
#23005,#23006,#23007,#23008,#23009,#23010,#23011,#23012,#23013,#23014,#23015,
#23016,#23017,#23018,#23019,#23020,#23021,#23022,#23023,#23024,#23025,#23026,
#23027,#23028,#23029,#23030,#23031,#23032,#23033,#23034,#23035,#23036,#23037,
#23038,#23039,#23040),.UNSPECIFIED.,.F.,.F.,(6,1,1,1,1,1,1,1,1,1,1,1,1,
1,1,1,1,1,1,1,1,1,1,1,1,1,1,1,1,1,1,1,1,1,1,1,1,1,1,1,1,1,1,1,1,1,1,1,1,
1,1,1,1,1,1,1,1,1,1,1,1,1,1,1,1,1,1,1,1,6),(0.,0.0142857142857143,0.0285714285714286,
0.0428571428571429,0.0571428571428571,0.0714285714285714,0.0857142857142857,
0.1,0.114285714285714,0.128571428571429,0.142857142857143,0.157142857142857,
0.171428571428571,0.185714285714286,0.2,0.214285714285714,0.228571428571429,
0.242857142857143,0.257142857142857,0.271428571428571,0.285714285714286,
0.3,0.314285714285714,0.328571428571429,0.342857142857143,0.357142857142857,
0.371428571428571,0.385714285714286,0.4,0.414285714285714,0.428571428571429,
0.442857142857143,0.457142857142857,0.471428571428572,0.485714285714286,
0.5,0.514285714285714,0.528571428571429,0.542857142857143,0.557142857142857,
0.571428571428571,0.585714285714286,0.6,0.614285714285714,0.628571428571428,
0.642857142857142,0.657142857142857,0.671428571428571,0.685714285714285,
0.699999999999999,0.714285714285714,0.728571428571428,0.742857142857142,
0.757142857142856,0.771428571428571,0.785714285714285,0.799999999999999,
0.814285714285713,0.828571428571428,0.842857142857142,0.857142857142856,
0.87142857142857,0.885714285714284,0.899999999999999,0.914285714285713,
0.928571428571427,0.942857142857141,0.957142857142856,0.97142857142857,
1.),.UNSPECIFIED.);
#515=B_SPLINE_CURVE_WITH_KNOTS('',5,(#23192,#23193,#23194,#23195,#23196,
#23197,#23198,#23199,#23200,#23201,#23202,#23203,#23204,#23205,#23206,#23207,
#23208,#23209,#23210,#23211,#23212,#23213,#23214,#23215,#23216,#23217,#23218,
#23219,#23220,#23221,#23222,#23223,#23224,#23225,#23226,#23227,#23228,#23229,
#23230,#23231,#23232,#23233,#23234,#23235,#23236,#23237,#23238,#23239,#23240,
#23241,#23242,#23243,#23244,#23245,#23246,#23247,#23248,#23249,#23250,#23251,
#23252,#23253,#23254,#23255,#23256,#23257,#23258,#23259,#23260,#23261,#23262,
#23263,#23264,#23265),.UNSPECIFIED.,.F.,.F.,(6,1,1,1,1,1,1,1,1,1,1,1,1,
1,1,1,1,1,1,1,1,1,1,1,1,1,1,1,1,1,1,1,1,1,1,1,1,1,1,1,1,1,1,1,1,1,1,1,1,
1,1,1,1,1,1,1,1,1,1,1,1,1,1,1,1,1,1,1,1,6),(0.,0.0142857142857143,0.0285714285714286,
0.0428571428571429,0.0571428571428571,0.0714285714285714,0.0857142857142857,
0.1,0.114285714285714,0.128571428571429,0.142857142857143,0.157142857142857,
0.171428571428571,0.185714285714286,0.2,0.214285714285714,0.228571428571429,
0.242857142857143,0.257142857142857,0.271428571428571,0.285714285714286,
0.3,0.314285714285714,0.328571428571429,0.342857142857143,0.357142857142857,
0.371428571428571,0.385714285714286,0.4,0.414285714285714,0.428571428571429,
0.442857142857143,0.457142857142857,0.471428571428572,0.485714285714286,
0.5,0.514285714285714,0.528571428571429,0.542857142857143,0.557142857142857,
0.571428571428571,0.585714285714286,0.6,0.614285714285714,0.628571428571428,
0.642857142857142,0.657142857142857,0.671428571428571,0.685714285714285,
0.699999999999999,0.714285714285714,0.728571428571428,0.742857142857142,
0.757142857142856,0.771428571428571,0.785714285714285,0.799999999999999,
0.814285714285713,0.828571428571428,0.842857142857142,0.857142857142856,
0.87142857142857,0.885714285714284,0.899999999999999,0.914285714285713,
0.928571428571427,0.942857142857141,0.957142857142856,0.97142857142857,
1.),.UNSPECIFIED.);
#516=B_SPLINE_CURVE_WITH_KNOTS('',5,(#23267,#23268,#23269,#23270,#23271,
#23272,#23273,#23274,#23275,#23276,#23277,#23278,#23279,#23280,#23281,#23282,
#23283,#23284,#23285,#23286,#23287,#23288,#23289,#23290,#23291,#23292,#23293,
#23294,#23295,#23296,#23297,#23298,#23299,#23300,#23301,#23302,#23303,#23304,
#23305,#23306,#23307,#23308,#23309,#23310,#23311,#23312,#23313,#23314,#23315,
#23316,#23317,#23318,#23319,#23320,#23321,#23322,#23323,#23324,#23325,#23326,
#23327,#23328,#23329,#23330,#23331,#23332,#23333,#23334,#23335,#23336,#23337,
#23338,#23339,#23340,#23341),.UNSPECIFIED.,.F.,.F.,(6,1,1,1,1,1,1,1,1,1,
1,1,1,1,1,1,1,1,1,1,1,1,1,1,1,1,1,1,1,1,1,1,1,1,1,1,1,1,1,1,1,1,1,1,1,1,
1,1,1,1,1,1,1,1,1,1,1,1,1,1,1,1,1,1,1,1,1,1,1,1,6),(-1.,-0.985714285714284,
-0.97142857142857,-0.957142857142856,-0.942857142857141,-0.928571428571427,
-0.914285714285713,-0.899999999999999,-0.885714285714284,-0.87142857142857,
-0.857142857142856,-0.842857142857142,-0.828571428571428,-0.814285714285713,
-0.799999999999999,-0.785714285714285,-0.771428571428571,-0.757142857142856,
-0.742857142857142,-0.728571428571428,-0.714285714285714,-0.699999999999999,
-0.685714285714285,-0.671428571428571,-0.657142857142857,-0.642857142857142,
-0.628571428571428,-0.614285714285714,-0.6,-0.585714285714286,-0.571428571428571,
-0.557142857142857,-0.542857142857143,-0.528571428571429,-0.514285714285714,
-0.5,-0.485714285714286,-0.471428571428572,-0.457142857142857,-0.442857142857143,
-0.428571428571429,-0.414285714285714,-0.4,-0.385714285714286,-0.371428571428571,
-0.357142857142857,-0.342857142857143,-0.328571428571429,-0.314285714285714,
-0.3,-0.285714285714286,-0.271428571428571,-0.257142857142857,-0.242857142857143,
-0.228571428571429,-0.214285714285714,-0.2,-0.185714285714286,-0.171428571428571,
-0.157142857142857,-0.142857142857143,-0.128571428571429,-0.114285714285714,
-0.1,-0.0857142857142857,-0.0714285714285714,-0.0571428571428571,-0.0428571428571429,
-0.0285714285714286,-0.0142857142857143,0.),.UNSPECIFIED.);
#517=B_SPLINE_CURVE_WITH_KNOTS('',5,(#23499,#23500,#23501,#23502,#23503,
#23504,#23505,#23506,#23507,#23508,#23509,#23510,#23511,#23512,#23513,#23514,
#23515,#23516,#23517,#23518,#23519,#23520,#23521,#23522,#23523,#23524,#23525,
#23526,#23527,#23528,#23529,#23530,#23531,#23532,#23533,#23534,#23535,#23536,
#23537,#23538,#23539,#23540,#23541,#23542,#23543,#23544,#23545,#23546,#23547,
#23548,#23549,#23550,#23551,#23552,#23553,#23554,#23555,#23556,#23557,#23558,
#23559,#23560,#23561,#23562,#23563,#23564,#23565,#23566,#23567,#23568,#23569,
#23570,#23571,#23572),.UNSPECIFIED.,.F.,.F.,(6,1,1,1,1,1,1,1,1,1,1,1,1,
1,1,1,1,1,1,1,1,1,1,1,1,1,1,1,1,1,1,1,1,1,1,1,1,1,1,1,1,1,1,1,1,1,1,1,1,
1,1,1,1,1,1,1,1,1,1,1,1,1,1,1,1,1,1,1,1,6),(0.,0.0142857142857143,0.0285714285714286,
0.0428571428571429,0.0571428571428571,0.0714285714285714,0.0857142857142857,
0.1,0.114285714285714,0.128571428571429,0.142857142857143,0.157142857142857,
0.171428571428571,0.185714285714286,0.2,0.214285714285714,0.228571428571429,
0.242857142857143,0.257142857142857,0.271428571428571,0.285714285714286,
0.3,0.314285714285714,0.328571428571429,0.342857142857143,0.357142857142857,
0.371428571428571,0.385714285714286,0.4,0.414285714285714,0.428571428571429,
0.442857142857143,0.457142857142857,0.471428571428572,0.485714285714286,
0.5,0.514285714285714,0.528571428571429,0.542857142857143,0.557142857142857,
0.571428571428571,0.585714285714286,0.6,0.614285714285714,0.628571428571428,
0.642857142857142,0.657142857142857,0.671428571428571,0.685714285714285,
0.699999999999999,0.714285714285714,0.728571428571428,0.742857142857142,
0.757142857142856,0.771428571428571,0.785714285714285,0.799999999999999,
0.814285714285713,0.828571428571428,0.842857142857142,0.857142857142856,
0.87142857142857,0.885714285714284,0.899999999999999,0.914285714285713,
0.928571428571427,0.942857142857141,0.957142857142856,0.97142857142857,
1.),.UNSPECIFIED.);
#518=B_SPLINE_CURVE_WITH_KNOTS('',5,(#23573,#23574,#23575,#23576,#23577,
#23578,#23579,#23580,#23581,#23582,#23583,#23584,#23585,#23586,#23587,#23588,
#23589,#23590,#23591,#23592,#23593,#23594,#23595,#23596,#23597,#23598,#23599,
#23600,#23601,#23602,#23603,#23604,#23605,#23606,#23607,#23608,#23609,#23610,
#23611,#23612,#23613,#23614,#23615,#23616,#23617,#23618,#23619,#23620,#23621,
#23622,#23623,#23624,#23625,#23626,#23627,#23628,#23629,#23630,#23631,#23632,
#23633,#23634,#23635,#23636,#23637,#23638,#23639,#23640,#23641,#23642,#23643,
#23644,#23645,#23646),.UNSPECIFIED.,.F.,.F.,(6,1,1,1,1,1,1,1,1,1,1,1,1,
1,1,1,1,1,1,1,1,1,1,1,1,1,1,1,1,1,1,1,1,1,1,1,1,1,1,1,1,1,1,1,1,1,1,1,1,
1,1,1,1,1,1,1,1,1,1,1,1,1,1,1,1,1,1,1,1,6),(0.,0.0142857142857143,0.0285714285714286,
0.0428571428571429,0.0571428571428571,0.0714285714285714,0.0857142857142857,
0.1,0.114285714285714,0.128571428571429,0.142857142857143,0.157142857142857,
0.171428571428571,0.185714285714286,0.2,0.214285714285714,0.228571428571429,
0.242857142857143,0.257142857142857,0.271428571428571,0.285714285714286,
0.3,0.314285714285714,0.328571428571429,0.342857142857143,0.357142857142857,
0.371428571428571,0.385714285714286,0.4,0.414285714285714,0.428571428571429,
0.442857142857143,0.457142857142857,0.471428571428572,0.485714285714286,
0.5,0.514285714285714,0.528571428571429,0.542857142857143,0.557142857142857,
0.571428571428571,0.585714285714286,0.6,0.614285714285714,0.628571428571428,
0.642857142857142,0.657142857142857,0.671428571428571,0.685714285714285,
0.699999999999999,0.714285714285714,0.728571428571428,0.742857142857142,
0.757142857142856,0.771428571428571,0.785714285714285,0.799999999999999,
0.814285714285713,0.828571428571428,0.842857142857142,0.857142857142856,
0.87142857142857,0.885714285714284,0.899999999999999,0.914285714285713,
0.928571428571427,0.942857142857141,0.957142857142856,0.97142857142857,
1.),.UNSPECIFIED.);
#519=B_SPLINE_CURVE_WITH_KNOTS('',5,(#23798,#23799,#23800,#23801,#23802,
#23803,#23804,#23805,#23806,#23807,#23808,#23809,#23810,#23811,#23812,#23813,
#23814,#23815,#23816,#23817,#23818,#23819,#23820,#23821,#23822,#23823,#23824,
#23825,#23826,#23827,#23828,#23829,#23830,#23831,#23832,#23833,#23834,#23835,
#23836,#23837,#23838,#23839,#23840,#23841,#23842,#23843,#23844,#23845,#23846,
#23847,#23848,#23849,#23850,#23851,#23852,#23853,#23854,#23855,#23856,#23857,
#23858,#23859,#23860,#23861,#23862,#23863,#23864,#23865,#23866,#23867,#23868,
#23869,#23870,#23871),.UNSPECIFIED.,.F.,.F.,(6,1,1,1,1,1,1,1,1,1,1,1,1,
1,1,1,1,1,1,1,1,1,1,1,1,1,1,1,1,1,1,1,1,1,1,1,1,1,1,1,1,1,1,1,1,1,1,1,1,
1,1,1,1,1,1,1,1,1,1,1,1,1,1,1,1,1,1,1,1,6),(0.,0.0142857142857143,0.0285714285714286,
0.0428571428571429,0.0571428571428571,0.0714285714285714,0.0857142857142857,
0.1,0.114285714285714,0.128571428571429,0.142857142857143,0.157142857142857,
0.171428571428571,0.185714285714286,0.2,0.214285714285714,0.228571428571429,
0.242857142857143,0.257142857142857,0.271428571428571,0.285714285714286,
0.3,0.314285714285714,0.328571428571429,0.342857142857143,0.357142857142857,
0.371428571428571,0.385714285714286,0.4,0.414285714285714,0.428571428571429,
0.442857142857143,0.457142857142857,0.471428571428572,0.485714285714286,
0.5,0.514285714285714,0.528571428571429,0.542857142857143,0.557142857142857,
0.571428571428571,0.585714285714286,0.6,0.614285714285714,0.628571428571428,
0.642857142857142,0.657142857142857,0.671428571428571,0.685714285714285,
0.699999999999999,0.714285714285714,0.728571428571428,0.742857142857142,
0.757142857142856,0.771428571428571,0.785714285714285,0.799999999999999,
0.814285714285713,0.828571428571428,0.842857142857142,0.857142857142856,
0.87142857142857,0.885714285714284,0.899999999999999,0.914285714285713,
0.928571428571427,0.942857142857141,0.957142857142856,0.97142857142857,
1.),.UNSPECIFIED.);
#520=B_SPLINE_CURVE_WITH_KNOTS('',5,(#23873,#23874,#23875,#23876,#23877,
#23878,#23879,#23880,#23881,#23882,#23883,#23884,#23885,#23886,#23887,#23888,
#23889,#23890,#23891,#23892,#23893,#23894,#23895,#23896,#23897,#23898,#23899,
#23900,#23901,#23902,#23903,#23904,#23905,#23906,#23907,#23908,#23909,#23910,
#23911,#23912,#23913,#23914,#23915,#23916,#23917,#23918,#23919,#23920,#23921,
#23922,#23923,#23924,#23925,#23926,#23927,#23928,#23929,#23930,#23931,#23932,
#23933,#23934,#23935,#23936,#23937,#23938,#23939,#23940,#23941,#23942,#23943,
#23944,#23945,#23946,#23947),.UNSPECIFIED.,.F.,.F.,(6,1,1,1,1,1,1,1,1,1,
1,1,1,1,1,1,1,1,1,1,1,1,1,1,1,1,1,1,1,1,1,1,1,1,1,1,1,1,1,1,1,1,1,1,1,1,
1,1,1,1,1,1,1,1,1,1,1,1,1,1,1,1,1,1,1,1,1,1,1,1,6),(-1.,-0.985714285714284,
-0.97142857142857,-0.957142857142856,-0.942857142857141,-0.928571428571427,
-0.914285714285713,-0.899999999999999,-0.885714285714284,-0.87142857142857,
-0.857142857142856,-0.842857142857142,-0.828571428571428,-0.814285714285713,
-0.799999999999999,-0.785714285714285,-0.771428571428571,-0.757142857142856,
-0.742857142857142,-0.728571428571428,-0.714285714285714,-0.699999999999999,
-0.685714285714285,-0.671428571428571,-0.657142857142857,-0.642857142857142,
-0.628571428571428,-0.614285714285714,-0.6,-0.585714285714286,-0.571428571428571,
-0.557142857142857,-0.542857142857143,-0.528571428571429,-0.514285714285714,
-0.5,-0.485714285714286,-0.471428571428572,-0.457142857142857,-0.442857142857143,
-0.428571428571429,-0.414285714285714,-0.4,-0.385714285714286,-0.371428571428571,
-0.357142857142857,-0.342857142857143,-0.328571428571429,-0.314285714285714,
-0.3,-0.285714285714286,-0.271428571428571,-0.257142857142857,-0.242857142857143,
-0.228571428571429,-0.214285714285714,-0.2,-0.185714285714286,-0.171428571428571,
-0.157142857142857,-0.142857142857143,-0.128571428571429,-0.114285714285714,
-0.1,-0.0857142857142857,-0.0714285714285714,-0.0571428571428571,-0.0428571428571429,
-0.0285714285714286,-0.0142857142857143,0.),.UNSPECIFIED.);
#521=B_SPLINE_CURVE_WITH_KNOTS('',5,(#24105,#24106,#24107,#24108,#24109,
#24110,#24111,#24112,#24113,#24114,#24115,#24116,#24117,#24118,#24119,#24120,
#24121,#24122,#24123,#24124,#24125,#24126,#24127,#24128,#24129,#24130,#24131,
#24132,#24133,#24134,#24135,#24136,#24137,#24138,#24139,#24140,#24141,#24142,
#24143,#24144,#24145,#24146,#24147,#24148,#24149,#24150,#24151,#24152,#24153,
#24154,#24155,#24156,#24157,#24158,#24159,#24160,#24161,#24162,#24163,#24164,
#24165,#24166,#24167,#24168,#24169,#24170,#24171,#24172,#24173,#24174,#24175,
#24176,#24177,#24178),.UNSPECIFIED.,.F.,.F.,(6,1,1,1,1,1,1,1,1,1,1,1,1,
1,1,1,1,1,1,1,1,1,1,1,1,1,1,1,1,1,1,1,1,1,1,1,1,1,1,1,1,1,1,1,1,1,1,1,1,
1,1,1,1,1,1,1,1,1,1,1,1,1,1,1,1,1,1,1,1,6),(0.,0.0142857142857143,0.0285714285714286,
0.0428571428571429,0.0571428571428571,0.0714285714285714,0.0857142857142857,
0.1,0.114285714285714,0.128571428571429,0.142857142857143,0.157142857142857,
0.171428571428571,0.185714285714286,0.2,0.214285714285714,0.228571428571429,
0.242857142857143,0.257142857142857,0.271428571428571,0.285714285714286,
0.3,0.314285714285714,0.328571428571429,0.342857142857143,0.357142857142857,
0.371428571428571,0.385714285714286,0.4,0.414285714285714,0.428571428571429,
0.442857142857143,0.457142857142857,0.471428571428572,0.485714285714286,
0.5,0.514285714285714,0.528571428571429,0.542857142857143,0.557142857142857,
0.571428571428571,0.585714285714286,0.6,0.614285714285714,0.628571428571428,
0.642857142857142,0.657142857142857,0.671428571428571,0.685714285714285,
0.699999999999999,0.714285714285714,0.728571428571428,0.742857142857142,
0.757142857142856,0.771428571428571,0.785714285714285,0.799999999999999,
0.814285714285713,0.828571428571428,0.842857142857142,0.857142857142856,
0.87142857142857,0.885714285714284,0.899999999999999,0.914285714285713,
0.928571428571427,0.942857142857141,0.957142857142856,0.97142857142857,
1.),.UNSPECIFIED.);
#522=B_SPLINE_CURVE_WITH_KNOTS('',5,(#24179,#24180,#24181,#24182,#24183,
#24184,#24185,#24186,#24187,#24188,#24189,#24190,#24191,#24192,#24193,#24194,
#24195,#24196,#24197,#24198,#24199,#24200,#24201,#24202,#24203,#24204,#24205,
#24206,#24207,#24208,#24209,#24210,#24211,#24212,#24213,#24214,#24215,#24216,
#24217,#24218,#24219,#24220,#24221,#24222,#24223,#24224,#24225,#24226,#24227,
#24228,#24229,#24230,#24231,#24232,#24233,#24234,#24235,#24236,#24237,#24238,
#24239,#24240,#24241,#24242,#24243,#24244,#24245,#24246,#24247,#24248,#24249,
#24250,#24251,#24252),.UNSPECIFIED.,.F.,.F.,(6,1,1,1,1,1,1,1,1,1,1,1,1,
1,1,1,1,1,1,1,1,1,1,1,1,1,1,1,1,1,1,1,1,1,1,1,1,1,1,1,1,1,1,1,1,1,1,1,1,
1,1,1,1,1,1,1,1,1,1,1,1,1,1,1,1,1,1,1,1,6),(0.,0.0142857142857143,0.0285714285714286,
0.0428571428571429,0.0571428571428571,0.0714285714285714,0.0857142857142857,
0.1,0.114285714285714,0.128571428571429,0.142857142857143,0.157142857142857,
0.171428571428571,0.185714285714286,0.2,0.214285714285714,0.228571428571429,
0.242857142857143,0.257142857142857,0.271428571428571,0.285714285714286,
0.3,0.314285714285714,0.328571428571429,0.342857142857143,0.357142857142857,
0.371428571428571,0.385714285714286,0.4,0.414285714285714,0.428571428571429,
0.442857142857143,0.457142857142857,0.471428571428572,0.485714285714286,
0.5,0.514285714285714,0.528571428571429,0.542857142857143,0.557142857142857,
0.571428571428571,0.585714285714286,0.6,0.614285714285714,0.628571428571428,
0.642857142857142,0.657142857142857,0.671428571428571,0.685714285714285,
0.699999999999999,0.714285714285714,0.728571428571428,0.742857142857142,
0.757142857142856,0.771428571428571,0.785714285714285,0.799999999999999,
0.814285714285713,0.828571428571428,0.842857142857142,0.857142857142856,
0.87142857142857,0.885714285714284,0.899999999999999,0.914285714285713,
0.928571428571427,0.942857142857141,0.957142857142856,0.97142857142857,
1.),.UNSPECIFIED.);
#523=B_SPLINE_CURVE_WITH_KNOTS('',5,(#24404,#24405,#24406,#24407,#24408,
#24409,#24410,#24411,#24412,#24413,#24414,#24415,#24416,#24417,#24418,#24419,
#24420,#24421,#24422,#24423,#24424,#24425,#24426,#24427,#24428,#24429,#24430,
#24431,#24432,#24433,#24434,#24435,#24436,#24437,#24438,#24439,#24440,#24441,
#24442,#24443,#24444,#24445,#24446,#24447,#24448,#24449,#24450,#24451,#24452,
#24453,#24454,#24455,#24456,#24457,#24458,#24459,#24460,#24461,#24462,#24463,
#24464,#24465,#24466,#24467,#24468,#24469,#24470,#24471,#24472,#24473,#24474,
#24475,#24476,#24477),.UNSPECIFIED.,.F.,.F.,(6,1,1,1,1,1,1,1,1,1,1,1,1,
1,1,1,1,1,1,1,1,1,1,1,1,1,1,1,1,1,1,1,1,1,1,1,1,1,1,1,1,1,1,1,1,1,1,1,1,
1,1,1,1,1,1,1,1,1,1,1,1,1,1,1,1,1,1,1,1,6),(0.,0.0142857142857143,0.0285714285714286,
0.0428571428571429,0.0571428571428571,0.0714285714285714,0.0857142857142857,
0.1,0.114285714285714,0.128571428571429,0.142857142857143,0.157142857142857,
0.171428571428571,0.185714285714286,0.2,0.214285714285714,0.228571428571429,
0.242857142857143,0.257142857142857,0.271428571428571,0.285714285714286,
0.3,0.314285714285714,0.328571428571429,0.342857142857143,0.357142857142857,
0.371428571428571,0.385714285714286,0.4,0.414285714285714,0.428571428571429,
0.442857142857143,0.457142857142857,0.471428571428572,0.485714285714286,
0.5,0.514285714285714,0.528571428571429,0.542857142857143,0.557142857142857,
0.571428571428571,0.585714285714286,0.6,0.614285714285714,0.628571428571428,
0.642857142857142,0.657142857142857,0.671428571428571,0.685714285714285,
0.699999999999999,0.714285714285714,0.728571428571428,0.742857142857142,
0.757142857142856,0.771428571428571,0.785714285714285,0.799999999999999,
0.814285714285713,0.828571428571428,0.842857142857142,0.857142857142856,
0.87142857142857,0.885714285714284,0.899999999999999,0.914285714285713,
0.928571428571427,0.942857142857141,0.957142857142856,0.97142857142857,
1.),.UNSPECIFIED.);
#524=B_SPLINE_CURVE_WITH_KNOTS('',5,(#24479,#24480,#24481,#24482,#24483,
#24484,#24485,#24486,#24487,#24488,#24489,#24490,#24491,#24492,#24493,#24494,
#24495,#24496,#24497,#24498,#24499,#24500,#24501,#24502,#24503,#24504,#24505,
#24506,#24507,#24508,#24509,#24510,#24511,#24512,#24513,#24514,#24515,#24516,
#24517,#24518,#24519,#24520,#24521,#24522,#24523,#24524,#24525,#24526,#24527,
#24528,#24529,#24530,#24531,#24532,#24533,#24534,#24535,#24536,#24537,#24538,
#24539,#24540,#24541,#24542,#24543,#24544,#24545,#24546,#24547,#24548,#24549,
#24550,#24551,#24552,#24553),.UNSPECIFIED.,.F.,.F.,(6,1,1,1,1,1,1,1,1,1,
1,1,1,1,1,1,1,1,1,1,1,1,1,1,1,1,1,1,1,1,1,1,1,1,1,1,1,1,1,1,1,1,1,1,1,1,
1,1,1,1,1,1,1,1,1,1,1,1,1,1,1,1,1,1,1,1,1,1,1,1,6),(-1.,-0.985714285714284,
-0.97142857142857,-0.957142857142856,-0.942857142857141,-0.928571428571427,
-0.914285714285713,-0.899999999999999,-0.885714285714284,-0.87142857142857,
-0.857142857142856,-0.842857142857142,-0.828571428571428,-0.814285714285713,
-0.799999999999999,-0.785714285714285,-0.771428571428571,-0.757142857142856,
-0.742857142857142,-0.728571428571428,-0.714285714285714,-0.699999999999999,
-0.685714285714285,-0.671428571428571,-0.657142857142857,-0.642857142857142,
-0.628571428571428,-0.614285714285714,-0.6,-0.585714285714286,-0.571428571428571,
-0.557142857142857,-0.542857142857143,-0.528571428571429,-0.514285714285714,
-0.5,-0.485714285714286,-0.471428571428572,-0.457142857142857,-0.442857142857143,
-0.428571428571429,-0.414285714285714,-0.4,-0.385714285714286,-0.371428571428571,
-0.357142857142857,-0.342857142857143,-0.328571428571429,-0.314285714285714,
-0.3,-0.285714285714286,-0.271428571428571,-0.257142857142857,-0.242857142857143,
-0.228571428571429,-0.214285714285714,-0.2,-0.185714285714286,-0.171428571428571,
-0.157142857142857,-0.142857142857143,-0.128571428571429,-0.114285714285714,
-0.1,-0.0857142857142857,-0.0714285714285714,-0.0571428571428571,-0.0428571428571429,
-0.0285714285714286,-0.0142857142857143,0.),.UNSPECIFIED.);
#525=B_SPLINE_CURVE_WITH_KNOTS('',5,(#24711,#24712,#24713,#24714,#24715,
#24716,#24717,#24718,#24719,#24720,#24721,#24722,#24723,#24724,#24725,#24726,
#24727,#24728,#24729,#24730,#24731,#24732,#24733,#24734,#24735,#24736,#24737,
#24738,#24739,#24740,#24741,#24742,#24743,#24744,#24745,#24746,#24747,#24748,
#24749,#24750,#24751,#24752,#24753,#24754,#24755,#24756,#24757,#24758,#24759,
#24760,#24761,#24762,#24763,#24764,#24765,#24766,#24767,#24768,#24769,#24770,
#24771,#24772,#24773,#24774,#24775,#24776,#24777,#24778,#24779,#24780,#24781,
#24782,#24783,#24784),.UNSPECIFIED.,.F.,.F.,(6,1,1,1,1,1,1,1,1,1,1,1,1,
1,1,1,1,1,1,1,1,1,1,1,1,1,1,1,1,1,1,1,1,1,1,1,1,1,1,1,1,1,1,1,1,1,1,1,1,
1,1,1,1,1,1,1,1,1,1,1,1,1,1,1,1,1,1,1,1,6),(0.,0.0142857142857143,0.0285714285714286,
0.0428571428571429,0.0571428571428571,0.0714285714285714,0.0857142857142857,
0.1,0.114285714285714,0.128571428571429,0.142857142857143,0.157142857142857,
0.171428571428571,0.185714285714286,0.2,0.214285714285714,0.228571428571429,
0.242857142857143,0.257142857142857,0.271428571428571,0.285714285714286,
0.3,0.314285714285714,0.328571428571429,0.342857142857143,0.357142857142857,
0.371428571428571,0.385714285714286,0.4,0.414285714285714,0.428571428571429,
0.442857142857143,0.457142857142857,0.471428571428572,0.485714285714286,
0.5,0.514285714285714,0.528571428571429,0.542857142857143,0.557142857142857,
0.571428571428571,0.585714285714286,0.6,0.614285714285714,0.628571428571428,
0.642857142857142,0.657142857142857,0.671428571428571,0.685714285714285,
0.699999999999999,0.714285714285714,0.728571428571428,0.742857142857142,
0.757142857142856,0.771428571428571,0.785714285714285,0.799999999999999,
0.814285714285713,0.828571428571428,0.842857142857142,0.857142857142856,
0.87142857142857,0.885714285714284,0.899999999999999,0.914285714285713,
0.928571428571427,0.942857142857141,0.957142857142856,0.97142857142857,
1.),.UNSPECIFIED.);
#526=B_SPLINE_CURVE_WITH_KNOTS('',5,(#24785,#24786,#24787,#24788,#24789,
#24790,#24791,#24792,#24793,#24794,#24795,#24796,#24797,#24798,#24799,#24800,
#24801,#24802,#24803,#24804,#24805,#24806,#24807,#24808,#24809,#24810,#24811,
#24812,#24813,#24814,#24815,#24816,#24817,#24818,#24819,#24820,#24821,#24822,
#24823,#24824,#24825,#24826,#24827,#24828,#24829,#24830,#24831,#24832,#24833,
#24834,#24835,#24836,#24837,#24838,#24839,#24840,#24841,#24842,#24843,#24844,
#24845,#24846,#24847,#24848,#24849,#24850,#24851,#24852,#24853,#24854,#24855,
#24856,#24857,#24858),.UNSPECIFIED.,.F.,.F.,(6,1,1,1,1,1,1,1,1,1,1,1,1,
1,1,1,1,1,1,1,1,1,1,1,1,1,1,1,1,1,1,1,1,1,1,1,1,1,1,1,1,1,1,1,1,1,1,1,1,
1,1,1,1,1,1,1,1,1,1,1,1,1,1,1,1,1,1,1,1,6),(0.,0.0142857142857143,0.0285714285714286,
0.0428571428571429,0.0571428571428571,0.0714285714285714,0.0857142857142857,
0.1,0.114285714285714,0.128571428571429,0.142857142857143,0.157142857142857,
0.171428571428571,0.185714285714286,0.2,0.214285714285714,0.228571428571429,
0.242857142857143,0.257142857142857,0.271428571428571,0.285714285714286,
0.3,0.314285714285714,0.328571428571429,0.342857142857143,0.357142857142857,
0.371428571428571,0.385714285714286,0.4,0.414285714285714,0.428571428571429,
0.442857142857143,0.457142857142857,0.471428571428572,0.485714285714286,
0.5,0.514285714285714,0.528571428571429,0.542857142857143,0.557142857142857,
0.571428571428571,0.585714285714286,0.6,0.614285714285714,0.628571428571428,
0.642857142857142,0.657142857142857,0.671428571428571,0.685714285714285,
0.699999999999999,0.714285714285714,0.728571428571428,0.742857142857142,
0.757142857142856,0.771428571428571,0.785714285714285,0.799999999999999,
0.814285714285713,0.828571428571428,0.842857142857142,0.857142857142856,
0.87142857142857,0.885714285714284,0.899999999999999,0.914285714285713,
0.928571428571427,0.942857142857141,0.957142857142856,0.97142857142857,
1.),.UNSPECIFIED.);
#527=B_SPLINE_CURVE_WITH_KNOTS('',5,(#25010,#25011,#25012,#25013,#25014,
#25015,#25016,#25017,#25018,#25019,#25020,#25021,#25022,#25023,#25024,#25025,
#25026,#25027,#25028,#25029,#25030,#25031,#25032,#25033,#25034,#25035,#25036,
#25037,#25038,#25039,#25040,#25041,#25042,#25043,#25044,#25045,#25046,#25047,
#25048,#25049,#25050,#25051,#25052,#25053,#25054,#25055,#25056,#25057,#25058,
#25059,#25060,#25061,#25062,#25063,#25064,#25065,#25066,#25067,#25068,#25069,
#25070,#25071,#25072,#25073,#25074,#25075,#25076,#25077,#25078,#25079,#25080,
#25081,#25082,#25083),.UNSPECIFIED.,.F.,.F.,(6,1,1,1,1,1,1,1,1,1,1,1,1,
1,1,1,1,1,1,1,1,1,1,1,1,1,1,1,1,1,1,1,1,1,1,1,1,1,1,1,1,1,1,1,1,1,1,1,1,
1,1,1,1,1,1,1,1,1,1,1,1,1,1,1,1,1,1,1,1,6),(0.,0.0142857142857143,0.0285714285714286,
0.0428571428571429,0.0571428571428571,0.0714285714285714,0.0857142857142857,
0.1,0.114285714285714,0.128571428571429,0.142857142857143,0.157142857142857,
0.171428571428571,0.185714285714286,0.2,0.214285714285714,0.228571428571429,
0.242857142857143,0.257142857142857,0.271428571428571,0.285714285714286,
0.3,0.314285714285714,0.328571428571429,0.342857142857143,0.357142857142857,
0.371428571428571,0.385714285714286,0.4,0.414285714285714,0.428571428571429,
0.442857142857143,0.457142857142857,0.471428571428572,0.485714285714286,
0.5,0.514285714285714,0.528571428571429,0.542857142857143,0.557142857142857,
0.571428571428571,0.585714285714286,0.6,0.614285714285714,0.628571428571428,
0.642857142857142,0.657142857142857,0.671428571428571,0.685714285714285,
0.699999999999999,0.714285714285714,0.728571428571428,0.742857142857142,
0.757142857142856,0.771428571428571,0.785714285714285,0.799999999999999,
0.814285714285713,0.828571428571428,0.842857142857142,0.857142857142856,
0.87142857142857,0.885714285714284,0.899999999999999,0.914285714285713,
0.928571428571427,0.942857142857141,0.957142857142856,0.97142857142857,
1.),.UNSPECIFIED.);
#528=B_SPLINE_CURVE_WITH_KNOTS('',5,(#25085,#25086,#25087,#25088,#25089,
#25090,#25091,#25092,#25093,#25094,#25095,#25096,#25097,#25098,#25099,#25100,
#25101,#25102,#25103,#25104,#25105,#25106,#25107,#25108,#25109,#25110,#25111,
#25112,#25113,#25114,#25115,#25116,#25117,#25118,#25119,#25120,#25121,#25122,
#25123,#25124,#25125,#25126,#25127,#25128,#25129,#25130,#25131,#25132,#25133,
#25134,#25135,#25136,#25137,#25138,#25139,#25140,#25141,#25142,#25143,#25144,
#25145,#25146,#25147,#25148,#25149,#25150,#25151,#25152,#25153,#25154,#25155,
#25156,#25157,#25158,#25159),.UNSPECIFIED.,.F.,.F.,(6,1,1,1,1,1,1,1,1,1,
1,1,1,1,1,1,1,1,1,1,1,1,1,1,1,1,1,1,1,1,1,1,1,1,1,1,1,1,1,1,1,1,1,1,1,1,
1,1,1,1,1,1,1,1,1,1,1,1,1,1,1,1,1,1,1,1,1,1,1,1,6),(-1.,-0.985714285714284,
-0.97142857142857,-0.957142857142856,-0.942857142857141,-0.928571428571427,
-0.914285714285713,-0.899999999999999,-0.885714285714284,-0.87142857142857,
-0.857142857142856,-0.842857142857142,-0.828571428571428,-0.814285714285713,
-0.799999999999999,-0.785714285714285,-0.771428571428571,-0.757142857142856,
-0.742857142857142,-0.728571428571428,-0.714285714285714,-0.699999999999999,
-0.685714285714285,-0.671428571428571,-0.657142857142857,-0.642857142857142,
-0.628571428571428,-0.614285714285714,-0.6,-0.585714285714286,-0.571428571428571,
-0.557142857142857,-0.542857142857143,-0.528571428571429,-0.514285714285714,
-0.5,-0.485714285714286,-0.471428571428572,-0.457142857142857,-0.442857142857143,
-0.428571428571429,-0.414285714285714,-0.4,-0.385714285714286,-0.371428571428571,
-0.357142857142857,-0.342857142857143,-0.328571428571429,-0.314285714285714,
-0.3,-0.285714285714286,-0.271428571428571,-0.257142857142857,-0.242857142857143,
-0.228571428571429,-0.214285714285714,-0.2,-0.185714285714286,-0.171428571428571,
-0.157142857142857,-0.142857142857143,-0.128571428571429,-0.114285714285714,
-0.1,-0.0857142857142857,-0.0714285714285714,-0.0571428571428571,-0.0428571428571429,
-0.0285714285714286,-0.0142857142857143,0.),.UNSPECIFIED.);
#529=B_SPLINE_CURVE_WITH_KNOTS('',5,(#25317,#25318,#25319,#25320,#25321,
#25322,#25323,#25324,#25325,#25326,#25327,#25328,#25329,#25330,#25331,#25332,
#25333,#25334,#25335,#25336,#25337,#25338,#25339,#25340,#25341,#25342,#25343,
#25344,#25345,#25346,#25347,#25348,#25349,#25350,#25351,#25352,#25353,#25354,
#25355,#25356,#25357,#25358,#25359,#25360,#25361,#25362,#25363,#25364,#25365,
#25366,#25367,#25368,#25369,#25370,#25371,#25372,#25373,#25374,#25375,#25376,
#25377,#25378,#25379,#25380,#25381,#25382,#25383,#25384,#25385,#25386,#25387,
#25388,#25389,#25390),.UNSPECIFIED.,.F.,.F.,(6,1,1,1,1,1,1,1,1,1,1,1,1,
1,1,1,1,1,1,1,1,1,1,1,1,1,1,1,1,1,1,1,1,1,1,1,1,1,1,1,1,1,1,1,1,1,1,1,1,
1,1,1,1,1,1,1,1,1,1,1,1,1,1,1,1,1,1,1,1,6),(0.,0.0142857142857143,0.0285714285714286,
0.0428571428571429,0.0571428571428571,0.0714285714285714,0.0857142857142857,
0.1,0.114285714285714,0.128571428571429,0.142857142857143,0.157142857142857,
0.171428571428571,0.185714285714286,0.2,0.214285714285714,0.228571428571429,
0.242857142857143,0.257142857142857,0.271428571428571,0.285714285714286,
0.3,0.314285714285714,0.328571428571429,0.342857142857143,0.357142857142857,
0.371428571428571,0.385714285714286,0.4,0.414285714285714,0.428571428571429,
0.442857142857143,0.457142857142857,0.471428571428572,0.485714285714286,
0.5,0.514285714285714,0.528571428571429,0.542857142857143,0.557142857142857,
0.571428571428571,0.585714285714286,0.6,0.614285714285714,0.628571428571428,
0.642857142857142,0.657142857142857,0.671428571428571,0.685714285714285,
0.699999999999999,0.714285714285714,0.728571428571428,0.742857142857142,
0.757142857142856,0.771428571428571,0.785714285714285,0.799999999999999,
0.814285714285713,0.828571428571428,0.842857142857142,0.857142857142856,
0.87142857142857,0.885714285714284,0.899999999999999,0.914285714285713,
0.928571428571427,0.942857142857141,0.957142857142856,0.97142857142857,
1.),.UNSPECIFIED.);
#530=B_SPLINE_CURVE_WITH_KNOTS('',5,(#25391,#25392,#25393,#25394,#25395,
#25396,#25397,#25398,#25399,#25400,#25401,#25402,#25403,#25404,#25405,#25406,
#25407,#25408,#25409,#25410,#25411,#25412,#25413,#25414,#25415,#25416,#25417,
#25418,#25419,#25420,#25421,#25422,#25423,#25424,#25425,#25426,#25427,#25428,
#25429,#25430,#25431,#25432,#25433,#25434,#25435,#25436,#25437,#25438,#25439,
#25440,#25441,#25442,#25443,#25444,#25445,#25446,#25447,#25448,#25449,#25450,
#25451,#25452,#25453,#25454,#25455,#25456,#25457,#25458,#25459,#25460,#25461,
#25462,#25463,#25464),.UNSPECIFIED.,.F.,.F.,(6,1,1,1,1,1,1,1,1,1,1,1,1,
1,1,1,1,1,1,1,1,1,1,1,1,1,1,1,1,1,1,1,1,1,1,1,1,1,1,1,1,1,1,1,1,1,1,1,1,
1,1,1,1,1,1,1,1,1,1,1,1,1,1,1,1,1,1,1,1,6),(0.,0.0142857142857143,0.0285714285714286,
0.0428571428571429,0.0571428571428571,0.0714285714285714,0.0857142857142857,
0.1,0.114285714285714,0.128571428571429,0.142857142857143,0.157142857142857,
0.171428571428571,0.185714285714286,0.2,0.214285714285714,0.228571428571429,
0.242857142857143,0.257142857142857,0.271428571428571,0.285714285714286,
0.3,0.314285714285714,0.328571428571429,0.342857142857143,0.357142857142857,
0.371428571428571,0.385714285714286,0.4,0.414285714285714,0.428571428571429,
0.442857142857143,0.457142857142857,0.471428571428572,0.485714285714286,
0.5,0.514285714285714,0.528571428571429,0.542857142857143,0.557142857142857,
0.571428571428571,0.585714285714286,0.6,0.614285714285714,0.628571428571428,
0.642857142857142,0.657142857142857,0.671428571428571,0.685714285714285,
0.699999999999999,0.714285714285714,0.728571428571428,0.742857142857142,
0.757142857142856,0.771428571428571,0.785714285714285,0.799999999999999,
0.814285714285713,0.828571428571428,0.842857142857142,0.857142857142856,
0.87142857142857,0.885714285714284,0.899999999999999,0.914285714285713,
0.928571428571427,0.942857142857141,0.957142857142856,0.97142857142857,
1.),.UNSPECIFIED.);
#531=B_SPLINE_CURVE_WITH_KNOTS('',5,(#25616,#25617,#25618,#25619,#25620,
#25621,#25622,#25623,#25624,#25625,#25626,#25627,#25628,#25629,#25630,#25631,
#25632,#25633,#25634,#25635,#25636,#25637,#25638,#25639,#25640,#25641,#25642,
#25643,#25644,#25645,#25646,#25647,#25648,#25649,#25650,#25651,#25652,#25653,
#25654,#25655,#25656,#25657,#25658,#25659,#25660,#25661,#25662,#25663,#25664,
#25665,#25666,#25667,#25668,#25669,#25670,#25671,#25672,#25673,#25674,#25675,
#25676,#25677,#25678,#25679,#25680,#25681,#25682,#25683,#25684,#25685,#25686,
#25687,#25688,#25689),.UNSPECIFIED.,.F.,.F.,(6,1,1,1,1,1,1,1,1,1,1,1,1,
1,1,1,1,1,1,1,1,1,1,1,1,1,1,1,1,1,1,1,1,1,1,1,1,1,1,1,1,1,1,1,1,1,1,1,1,
1,1,1,1,1,1,1,1,1,1,1,1,1,1,1,1,1,1,1,1,6),(0.,0.0142857142857143,0.0285714285714286,
0.0428571428571429,0.0571428571428571,0.0714285714285714,0.0857142857142857,
0.1,0.114285714285714,0.128571428571429,0.142857142857143,0.157142857142857,
0.171428571428571,0.185714285714286,0.2,0.214285714285714,0.228571428571429,
0.242857142857143,0.257142857142857,0.271428571428571,0.285714285714286,
0.3,0.314285714285714,0.328571428571429,0.342857142857143,0.357142857142857,
0.371428571428571,0.385714285714286,0.4,0.414285714285714,0.428571428571429,
0.442857142857143,0.457142857142857,0.471428571428572,0.485714285714286,
0.5,0.514285714285714,0.528571428571429,0.542857142857143,0.557142857142857,
0.571428571428571,0.585714285714286,0.6,0.614285714285714,0.628571428571428,
0.642857142857142,0.657142857142857,0.671428571428571,0.685714285714285,
0.699999999999999,0.714285714285714,0.728571428571428,0.742857142857142,
0.757142857142856,0.771428571428571,0.785714285714285,0.799999999999999,
0.814285714285713,0.828571428571428,0.842857142857142,0.857142857142856,
0.87142857142857,0.885714285714284,0.899999999999999,0.914285714285713,
0.928571428571427,0.942857142857141,0.957142857142856,0.97142857142857,
1.),.UNSPECIFIED.);
#532=B_SPLINE_CURVE_WITH_KNOTS('',5,(#25691,#25692,#25693,#25694,#25695,
#25696,#25697,#25698,#25699,#25700,#25701,#25702,#25703,#25704,#25705,#25706,
#25707,#25708,#25709,#25710,#25711,#25712,#25713,#25714,#25715,#25716,#25717,
#25718,#25719,#25720,#25721,#25722,#25723,#25724,#25725,#25726,#25727,#25728,
#25729,#25730,#25731,#25732,#25733,#25734,#25735,#25736,#25737,#25738,#25739,
#25740,#25741,#25742,#25743,#25744,#25745,#25746,#25747,#25748,#25749,#25750,
#25751,#25752,#25753,#25754,#25755,#25756,#25757,#25758,#25759,#25760,#25761,
#25762,#25763,#25764,#25765),.UNSPECIFIED.,.F.,.F.,(6,1,1,1,1,1,1,1,1,1,
1,1,1,1,1,1,1,1,1,1,1,1,1,1,1,1,1,1,1,1,1,1,1,1,1,1,1,1,1,1,1,1,1,1,1,1,
1,1,1,1,1,1,1,1,1,1,1,1,1,1,1,1,1,1,1,1,1,1,1,1,6),(-1.,-0.985714285714284,
-0.97142857142857,-0.957142857142856,-0.942857142857141,-0.928571428571427,
-0.914285714285713,-0.899999999999999,-0.885714285714284,-0.87142857142857,
-0.857142857142856,-0.842857142857142,-0.828571428571428,-0.814285714285713,
-0.799999999999999,-0.785714285714285,-0.771428571428571,-0.757142857142856,
-0.742857142857142,-0.728571428571428,-0.714285714285714,-0.699999999999999,
-0.685714285714285,-0.671428571428571,-0.657142857142857,-0.642857142857142,
-0.628571428571428,-0.614285714285714,-0.6,-0.585714285714286,-0.571428571428571,
-0.557142857142857,-0.542857142857143,-0.528571428571429,-0.514285714285714,
-0.5,-0.485714285714286,-0.471428571428572,-0.457142857142857,-0.442857142857143,
-0.428571428571429,-0.414285714285714,-0.4,-0.385714285714286,-0.371428571428571,
-0.357142857142857,-0.342857142857143,-0.328571428571429,-0.314285714285714,
-0.3,-0.285714285714286,-0.271428571428571,-0.257142857142857,-0.242857142857143,
-0.228571428571429,-0.214285714285714,-0.2,-0.185714285714286,-0.171428571428571,
-0.157142857142857,-0.142857142857143,-0.128571428571429,-0.114285714285714,
-0.1,-0.0857142857142857,-0.0714285714285714,-0.0571428571428571,-0.0428571428571429,
-0.0285714285714286,-0.0142857142857143,0.),.UNSPECIFIED.);
#533=B_SPLINE_CURVE_WITH_KNOTS('',5,(#25923,#25924,#25925,#25926,#25927,
#25928,#25929,#25930,#25931,#25932,#25933,#25934,#25935,#25936,#25937,#25938,
#25939,#25940,#25941,#25942,#25943,#25944,#25945,#25946,#25947,#25948,#25949,
#25950,#25951,#25952,#25953,#25954,#25955,#25956,#25957,#25958,#25959,#25960,
#25961,#25962,#25963,#25964,#25965,#25966,#25967,#25968,#25969,#25970,#25971,
#25972,#25973,#25974,#25975,#25976,#25977,#25978,#25979,#25980,#25981,#25982,
#25983,#25984,#25985,#25986,#25987,#25988,#25989,#25990,#25991,#25992,#25993,
#25994,#25995,#25996),.UNSPECIFIED.,.F.,.F.,(6,1,1,1,1,1,1,1,1,1,1,1,1,
1,1,1,1,1,1,1,1,1,1,1,1,1,1,1,1,1,1,1,1,1,1,1,1,1,1,1,1,1,1,1,1,1,1,1,1,
1,1,1,1,1,1,1,1,1,1,1,1,1,1,1,1,1,1,1,1,6),(0.,0.0142857142857143,0.0285714285714286,
0.0428571428571429,0.0571428571428571,0.0714285714285714,0.0857142857142857,
0.1,0.114285714285714,0.128571428571429,0.142857142857143,0.157142857142857,
0.171428571428571,0.185714285714286,0.2,0.214285714285714,0.228571428571429,
0.242857142857143,0.257142857142857,0.271428571428571,0.285714285714286,
0.3,0.314285714285714,0.328571428571429,0.342857142857143,0.357142857142857,
0.371428571428571,0.385714285714286,0.4,0.414285714285714,0.428571428571429,
0.442857142857143,0.457142857142857,0.471428571428572,0.485714285714286,
0.5,0.514285714285714,0.528571428571429,0.542857142857143,0.557142857142857,
0.571428571428571,0.585714285714286,0.6,0.614285714285714,0.628571428571428,
0.642857142857142,0.657142857142857,0.671428571428571,0.685714285714285,
0.699999999999999,0.714285714285714,0.728571428571428,0.742857142857142,
0.757142857142856,0.771428571428571,0.785714285714285,0.799999999999999,
0.814285714285713,0.828571428571428,0.842857142857142,0.857142857142856,
0.87142857142857,0.885714285714284,0.899999999999999,0.914285714285713,
0.928571428571427,0.942857142857141,0.957142857142856,0.97142857142857,
1.),.UNSPECIFIED.);
#534=B_SPLINE_CURVE_WITH_KNOTS('',5,(#25997,#25998,#25999,#26000,#26001,
#26002,#26003,#26004,#26005,#26006,#26007,#26008,#26009,#26010,#26011,#26012,
#26013,#26014,#26015,#26016,#26017,#26018,#26019,#26020,#26021,#26022,#26023,
#26024,#26025,#26026,#26027,#26028,#26029,#26030,#26031,#26032,#26033,#26034,
#26035,#26036,#26037,#26038,#26039,#26040,#26041,#26042,#26043,#26044,#26045,
#26046,#26047,#26048,#26049,#26050,#26051,#26052,#26053,#26054,#26055,#26056,
#26057,#26058,#26059,#26060,#26061,#26062,#26063,#26064,#26065,#26066,#26067,
#26068,#26069,#26070),.UNSPECIFIED.,.F.,.F.,(6,1,1,1,1,1,1,1,1,1,1,1,1,
1,1,1,1,1,1,1,1,1,1,1,1,1,1,1,1,1,1,1,1,1,1,1,1,1,1,1,1,1,1,1,1,1,1,1,1,
1,1,1,1,1,1,1,1,1,1,1,1,1,1,1,1,1,1,1,1,6),(0.,0.0142857142857143,0.0285714285714286,
0.0428571428571429,0.0571428571428571,0.0714285714285714,0.0857142857142857,
0.1,0.114285714285714,0.128571428571429,0.142857142857143,0.157142857142857,
0.171428571428571,0.185714285714286,0.2,0.214285714285714,0.228571428571429,
0.242857142857143,0.257142857142857,0.271428571428571,0.285714285714286,
0.3,0.314285714285714,0.328571428571429,0.342857142857143,0.357142857142857,
0.371428571428571,0.385714285714286,0.4,0.414285714285714,0.428571428571429,
0.442857142857143,0.457142857142857,0.471428571428572,0.485714285714286,
0.5,0.514285714285714,0.528571428571429,0.542857142857143,0.557142857142857,
0.571428571428571,0.585714285714286,0.6,0.614285714285714,0.628571428571428,
0.642857142857142,0.657142857142857,0.671428571428571,0.685714285714285,
0.699999999999999,0.714285714285714,0.728571428571428,0.742857142857142,
0.757142857142856,0.771428571428571,0.785714285714285,0.799999999999999,
0.814285714285713,0.828571428571428,0.842857142857142,0.857142857142856,
0.87142857142857,0.885714285714284,0.899999999999999,0.914285714285713,
0.928571428571427,0.942857142857141,0.957142857142856,0.97142857142857,
1.),.UNSPECIFIED.);
#535=B_SPLINE_CURVE_WITH_KNOTS('',5,(#26222,#26223,#26224,#26225,#26226,
#26227,#26228,#26229,#26230,#26231,#26232,#26233,#26234,#26235,#26236,#26237,
#26238,#26239,#26240,#26241,#26242,#26243,#26244,#26245,#26246,#26247,#26248,
#26249,#26250,#26251,#26252,#26253,#26254,#26255,#26256,#26257,#26258,#26259,
#26260,#26261,#26262,#26263,#26264,#26265,#26266,#26267,#26268,#26269,#26270,
#26271,#26272,#26273,#26274,#26275,#26276,#26277,#26278,#26279,#26280,#26281,
#26282,#26283,#26284,#26285,#26286,#26287,#26288,#26289,#26290,#26291,#26292,
#26293,#26294,#26295),.UNSPECIFIED.,.F.,.F.,(6,1,1,1,1,1,1,1,1,1,1,1,1,
1,1,1,1,1,1,1,1,1,1,1,1,1,1,1,1,1,1,1,1,1,1,1,1,1,1,1,1,1,1,1,1,1,1,1,1,
1,1,1,1,1,1,1,1,1,1,1,1,1,1,1,1,1,1,1,1,6),(0.,0.0142857142857143,0.0285714285714286,
0.0428571428571429,0.0571428571428571,0.0714285714285714,0.0857142857142857,
0.1,0.114285714285714,0.128571428571429,0.142857142857143,0.157142857142857,
0.171428571428571,0.185714285714286,0.2,0.214285714285714,0.228571428571429,
0.242857142857143,0.257142857142857,0.271428571428571,0.285714285714286,
0.3,0.314285714285714,0.328571428571429,0.342857142857143,0.357142857142857,
0.371428571428571,0.385714285714286,0.4,0.414285714285714,0.428571428571429,
0.442857142857143,0.457142857142857,0.471428571428572,0.485714285714286,
0.5,0.514285714285714,0.528571428571429,0.542857142857143,0.557142857142857,
0.571428571428571,0.585714285714286,0.6,0.614285714285714,0.628571428571428,
0.642857142857142,0.657142857142857,0.671428571428571,0.685714285714285,
0.699999999999999,0.714285714285714,0.728571428571428,0.742857142857142,
0.757142857142856,0.771428571428571,0.785714285714285,0.799999999999999,
0.814285714285713,0.828571428571428,0.842857142857142,0.857142857142856,
0.87142857142857,0.885714285714284,0.899999999999999,0.914285714285713,
0.928571428571427,0.942857142857141,0.957142857142856,0.97142857142857,
1.),.UNSPECIFIED.);
#536=B_SPLINE_CURVE_WITH_KNOTS('',5,(#26297,#26298,#26299,#26300,#26301,
#26302,#26303,#26304,#26305,#26306,#26307,#26308,#26309,#26310,#26311,#26312,
#26313,#26314,#26315,#26316,#26317,#26318,#26319,#26320,#26321,#26322,#26323,
#26324,#26325,#26326,#26327,#26328,#26329,#26330,#26331,#26332,#26333,#26334,
#26335,#26336,#26337,#26338,#26339,#26340,#26341,#26342,#26343,#26344,#26345,
#26346,#26347,#26348,#26349,#26350,#26351,#26352,#26353,#26354,#26355,#26356,
#26357,#26358,#26359,#26360,#26361,#26362,#26363,#26364,#26365,#26366,#26367,
#26368,#26369,#26370,#26371),.UNSPECIFIED.,.F.,.F.,(6,1,1,1,1,1,1,1,1,1,
1,1,1,1,1,1,1,1,1,1,1,1,1,1,1,1,1,1,1,1,1,1,1,1,1,1,1,1,1,1,1,1,1,1,1,1,
1,1,1,1,1,1,1,1,1,1,1,1,1,1,1,1,1,1,1,1,1,1,1,1,6),(-1.,-0.985714285714284,
-0.97142857142857,-0.957142857142856,-0.942857142857141,-0.928571428571427,
-0.914285714285713,-0.899999999999999,-0.885714285714284,-0.87142857142857,
-0.857142857142856,-0.842857142857142,-0.828571428571428,-0.814285714285713,
-0.799999999999999,-0.785714285714285,-0.771428571428571,-0.757142857142856,
-0.742857142857142,-0.728571428571428,-0.714285714285714,-0.699999999999999,
-0.685714285714285,-0.671428571428571,-0.657142857142857,-0.642857142857142,
-0.628571428571428,-0.614285714285714,-0.6,-0.585714285714286,-0.571428571428571,
-0.557142857142857,-0.542857142857143,-0.528571428571429,-0.514285714285714,
-0.5,-0.485714285714286,-0.471428571428572,-0.457142857142857,-0.442857142857143,
-0.428571428571429,-0.414285714285714,-0.4,-0.385714285714286,-0.371428571428571,
-0.357142857142857,-0.342857142857143,-0.328571428571429,-0.314285714285714,
-0.3,-0.285714285714286,-0.271428571428571,-0.257142857142857,-0.242857142857143,
-0.228571428571429,-0.214285714285714,-0.2,-0.185714285714286,-0.171428571428571,
-0.157142857142857,-0.142857142857143,-0.128571428571429,-0.114285714285714,
-0.1,-0.0857142857142857,-0.0714285714285714,-0.0571428571428571,-0.0428571428571429,
-0.0285714285714286,-0.0142857142857143,0.),.UNSPECIFIED.);
#537=B_SPLINE_CURVE_WITH_KNOTS('',5,(#26529,#26530,#26531,#26532,#26533,
#26534,#26535,#26536,#26537,#26538,#26539,#26540,#26541,#26542,#26543,#26544,
#26545,#26546,#26547,#26548,#26549,#26550,#26551,#26552,#26553,#26554,#26555,
#26556,#26557,#26558,#26559,#26560,#26561,#26562,#26563,#26564,#26565,#26566,
#26567,#26568,#26569,#26570,#26571,#26572,#26573,#26574,#26575,#26576,#26577,
#26578,#26579,#26580,#26581,#26582,#26583,#26584,#26585,#26586,#26587,#26588,
#26589,#26590,#26591,#26592,#26593,#26594,#26595,#26596,#26597,#26598,#26599,
#26600,#26601,#26602),.UNSPECIFIED.,.F.,.F.,(6,1,1,1,1,1,1,1,1,1,1,1,1,
1,1,1,1,1,1,1,1,1,1,1,1,1,1,1,1,1,1,1,1,1,1,1,1,1,1,1,1,1,1,1,1,1,1,1,1,
1,1,1,1,1,1,1,1,1,1,1,1,1,1,1,1,1,1,1,1,6),(0.,0.0142857142857143,0.0285714285714286,
0.0428571428571429,0.0571428571428571,0.0714285714285714,0.0857142857142857,
0.1,0.114285714285714,0.128571428571429,0.142857142857143,0.157142857142857,
0.171428571428571,0.185714285714286,0.2,0.214285714285714,0.228571428571429,
0.242857142857143,0.257142857142857,0.271428571428571,0.285714285714286,
0.3,0.314285714285714,0.328571428571429,0.342857142857143,0.357142857142857,
0.371428571428571,0.385714285714286,0.4,0.414285714285714,0.428571428571429,
0.442857142857143,0.457142857142857,0.471428571428572,0.485714285714286,
0.5,0.514285714285714,0.528571428571429,0.542857142857143,0.557142857142857,
0.571428571428571,0.585714285714286,0.6,0.614285714285714,0.628571428571428,
0.642857142857142,0.657142857142857,0.671428571428571,0.685714285714285,
0.699999999999999,0.714285714285714,0.728571428571428,0.742857142857142,
0.757142857142856,0.771428571428571,0.785714285714285,0.799999999999999,
0.814285714285713,0.828571428571428,0.842857142857142,0.857142857142856,
0.87142857142857,0.885714285714284,0.899999999999999,0.914285714285713,
0.928571428571427,0.942857142857141,0.957142857142856,0.97142857142857,
1.),.UNSPECIFIED.);
#538=B_SPLINE_CURVE_WITH_KNOTS('',5,(#26603,#26604,#26605,#26606,#26607,
#26608,#26609,#26610,#26611,#26612,#26613,#26614,#26615,#26616,#26617,#26618,
#26619,#26620,#26621,#26622,#26623,#26624,#26625,#26626,#26627,#26628,#26629,
#26630,#26631,#26632,#26633,#26634,#26635,#26636,#26637,#26638,#26639,#26640,
#26641,#26642,#26643,#26644,#26645,#26646,#26647,#26648,#26649,#26650,#26651,
#26652,#26653,#26654,#26655,#26656,#26657,#26658,#26659,#26660,#26661,#26662,
#26663,#26664,#26665,#26666,#26667,#26668,#26669,#26670,#26671,#26672,#26673,
#26674,#26675,#26676),.UNSPECIFIED.,.F.,.F.,(6,1,1,1,1,1,1,1,1,1,1,1,1,
1,1,1,1,1,1,1,1,1,1,1,1,1,1,1,1,1,1,1,1,1,1,1,1,1,1,1,1,1,1,1,1,1,1,1,1,
1,1,1,1,1,1,1,1,1,1,1,1,1,1,1,1,1,1,1,1,6),(0.,0.0142857142857143,0.0285714285714286,
0.0428571428571429,0.0571428571428571,0.0714285714285714,0.0857142857142857,
0.1,0.114285714285714,0.128571428571429,0.142857142857143,0.157142857142857,
0.171428571428571,0.185714285714286,0.2,0.214285714285714,0.228571428571429,
0.242857142857143,0.257142857142857,0.271428571428571,0.285714285714286,
0.3,0.314285714285714,0.328571428571429,0.342857142857143,0.357142857142857,
0.371428571428571,0.385714285714286,0.4,0.414285714285714,0.428571428571429,
0.442857142857143,0.457142857142857,0.471428571428572,0.485714285714286,
0.5,0.514285714285714,0.528571428571429,0.542857142857143,0.557142857142857,
0.571428571428571,0.585714285714286,0.6,0.614285714285714,0.628571428571428,
0.642857142857142,0.657142857142857,0.671428571428571,0.685714285714285,
0.699999999999999,0.714285714285714,0.728571428571428,0.742857142857142,
0.757142857142856,0.771428571428571,0.785714285714285,0.799999999999999,
0.814285714285713,0.828571428571428,0.842857142857142,0.857142857142856,
0.87142857142857,0.885714285714284,0.899999999999999,0.914285714285713,
0.928571428571427,0.942857142857141,0.957142857142856,0.97142857142857,
1.),.UNSPECIFIED.);
#539=B_SPLINE_CURVE_WITH_KNOTS('',5,(#26828,#26829,#26830,#26831,#26832,
#26833,#26834,#26835,#26836,#26837,#26838,#26839,#26840,#26841,#26842,#26843,
#26844,#26845,#26846,#26847,#26848,#26849,#26850,#26851,#26852,#26853,#26854,
#26855,#26856,#26857,#26858,#26859,#26860,#26861,#26862,#26863,#26864,#26865,
#26866,#26867,#26868,#26869,#26870,#26871,#26872,#26873,#26874,#26875,#26876,
#26877,#26878,#26879,#26880,#26881,#26882,#26883,#26884,#26885,#26886,#26887,
#26888,#26889,#26890,#26891,#26892,#26893,#26894,#26895,#26896,#26897,#26898,
#26899,#26900,#26901),.UNSPECIFIED.,.F.,.F.,(6,1,1,1,1,1,1,1,1,1,1,1,1,
1,1,1,1,1,1,1,1,1,1,1,1,1,1,1,1,1,1,1,1,1,1,1,1,1,1,1,1,1,1,1,1,1,1,1,1,
1,1,1,1,1,1,1,1,1,1,1,1,1,1,1,1,1,1,1,1,6),(0.,0.0142857142857143,0.0285714285714286,
0.0428571428571429,0.0571428571428571,0.0714285714285714,0.0857142857142857,
0.1,0.114285714285714,0.128571428571429,0.142857142857143,0.157142857142857,
0.171428571428571,0.185714285714286,0.2,0.214285714285714,0.228571428571429,
0.242857142857143,0.257142857142857,0.271428571428571,0.285714285714286,
0.3,0.314285714285714,0.328571428571429,0.342857142857143,0.357142857142857,
0.371428571428571,0.385714285714286,0.4,0.414285714285714,0.428571428571429,
0.442857142857143,0.457142857142857,0.471428571428572,0.485714285714286,
0.5,0.514285714285714,0.528571428571429,0.542857142857143,0.557142857142857,
0.571428571428571,0.585714285714286,0.6,0.614285714285714,0.628571428571428,
0.642857142857142,0.657142857142857,0.671428571428571,0.685714285714285,
0.699999999999999,0.714285714285714,0.728571428571428,0.742857142857142,
0.757142857142856,0.771428571428571,0.785714285714285,0.799999999999999,
0.814285714285713,0.828571428571428,0.842857142857142,0.857142857142856,
0.87142857142857,0.885714285714284,0.899999999999999,0.914285714285713,
0.928571428571427,0.942857142857141,0.957142857142856,0.97142857142857,
1.),.UNSPECIFIED.);
#540=B_SPLINE_CURVE_WITH_KNOTS('',5,(#26903,#26904,#26905,#26906,#26907,
#26908,#26909,#26910,#26911,#26912,#26913,#26914,#26915,#26916,#26917,#26918,
#26919,#26920,#26921,#26922,#26923,#26924,#26925,#26926,#26927,#26928,#26929,
#26930,#26931,#26932,#26933,#26934,#26935,#26936,#26937,#26938,#26939,#26940,
#26941,#26942,#26943,#26944,#26945,#26946,#26947,#26948,#26949,#26950,#26951,
#26952,#26953,#26954,#26955,#26956,#26957,#26958,#26959,#26960,#26961,#26962,
#26963,#26964,#26965,#26966,#26967,#26968,#26969,#26970,#26971,#26972,#26973,
#26974,#26975,#26976,#26977),.UNSPECIFIED.,.F.,.F.,(6,1,1,1,1,1,1,1,1,1,
1,1,1,1,1,1,1,1,1,1,1,1,1,1,1,1,1,1,1,1,1,1,1,1,1,1,1,1,1,1,1,1,1,1,1,1,
1,1,1,1,1,1,1,1,1,1,1,1,1,1,1,1,1,1,1,1,1,1,1,1,6),(-1.,-0.985714285714284,
-0.97142857142857,-0.957142857142856,-0.942857142857141,-0.928571428571427,
-0.914285714285713,-0.899999999999999,-0.885714285714284,-0.87142857142857,
-0.857142857142856,-0.842857142857142,-0.828571428571428,-0.814285714285713,
-0.799999999999999,-0.785714285714285,-0.771428571428571,-0.757142857142856,
-0.742857142857142,-0.728571428571428,-0.714285714285714,-0.699999999999999,
-0.685714285714285,-0.671428571428571,-0.657142857142857,-0.642857142857142,
-0.628571428571428,-0.614285714285714,-0.6,-0.585714285714286,-0.571428571428571,
-0.557142857142857,-0.542857142857143,-0.528571428571429,-0.514285714285714,
-0.5,-0.485714285714286,-0.471428571428572,-0.457142857142857,-0.442857142857143,
-0.428571428571429,-0.414285714285714,-0.4,-0.385714285714286,-0.371428571428571,
-0.357142857142857,-0.342857142857143,-0.328571428571429,-0.314285714285714,
-0.3,-0.285714285714286,-0.271428571428571,-0.257142857142857,-0.242857142857143,
-0.228571428571429,-0.214285714285714,-0.2,-0.185714285714286,-0.171428571428571,
-0.157142857142857,-0.142857142857143,-0.128571428571429,-0.114285714285714,
-0.1,-0.0857142857142857,-0.0714285714285714,-0.0571428571428571,-0.0428571428571429,
-0.0285714285714286,-0.0142857142857143,0.),.UNSPECIFIED.);
#541=B_SPLINE_CURVE_WITH_KNOTS('',5,(#27135,#27136,#27137,#27138,#27139,
#27140,#27141,#27142,#27143,#27144,#27145,#27146,#27147,#27148,#27149,#27150,
#27151,#27152,#27153,#27154,#27155,#27156,#27157,#27158,#27159,#27160,#27161,
#27162,#27163,#27164,#27165,#27166,#27167,#27168,#27169,#27170,#27171,#27172,
#27173,#27174,#27175,#27176,#27177,#27178,#27179,#27180,#27181,#27182,#27183,
#27184,#27185,#27186,#27187,#27188,#27189,#27190,#27191,#27192,#27193,#27194,
#27195,#27196,#27197,#27198,#27199,#27200,#27201,#27202,#27203,#27204,#27205,
#27206,#27207,#27208),.UNSPECIFIED.,.F.,.F.,(6,1,1,1,1,1,1,1,1,1,1,1,1,
1,1,1,1,1,1,1,1,1,1,1,1,1,1,1,1,1,1,1,1,1,1,1,1,1,1,1,1,1,1,1,1,1,1,1,1,
1,1,1,1,1,1,1,1,1,1,1,1,1,1,1,1,1,1,1,1,6),(0.,0.0142857142857143,0.0285714285714286,
0.0428571428571429,0.0571428571428571,0.0714285714285714,0.0857142857142857,
0.1,0.114285714285714,0.128571428571429,0.142857142857143,0.157142857142857,
0.171428571428571,0.185714285714286,0.2,0.214285714285714,0.228571428571429,
0.242857142857143,0.257142857142857,0.271428571428571,0.285714285714286,
0.3,0.314285714285714,0.328571428571429,0.342857142857143,0.357142857142857,
0.371428571428571,0.385714285714286,0.4,0.414285714285714,0.428571428571429,
0.442857142857143,0.457142857142857,0.471428571428572,0.485714285714286,
0.5,0.514285714285714,0.528571428571429,0.542857142857143,0.557142857142857,
0.571428571428571,0.585714285714286,0.6,0.614285714285714,0.628571428571428,
0.642857142857142,0.657142857142857,0.671428571428571,0.685714285714285,
0.699999999999999,0.714285714285714,0.728571428571428,0.742857142857142,
0.757142857142856,0.771428571428571,0.785714285714285,0.799999999999999,
0.814285714285713,0.828571428571428,0.842857142857142,0.857142857142856,
0.87142857142857,0.885714285714284,0.899999999999999,0.914285714285713,
0.928571428571427,0.942857142857141,0.957142857142856,0.97142857142857,
1.),.UNSPECIFIED.);
#542=B_SPLINE_CURVE_WITH_KNOTS('',5,(#27209,#27210,#27211,#27212,#27213,
#27214,#27215,#27216,#27217,#27218,#27219,#27220,#27221,#27222,#27223,#27224,
#27225,#27226,#27227,#27228,#27229,#27230,#27231,#27232,#27233,#27234,#27235,
#27236,#27237,#27238,#27239,#27240,#27241,#27242,#27243,#27244,#27245,#27246,
#27247,#27248,#27249,#27250,#27251,#27252,#27253,#27254,#27255,#27256,#27257,
#27258,#27259,#27260,#27261,#27262,#27263,#27264,#27265,#27266,#27267,#27268,
#27269,#27270,#27271,#27272,#27273,#27274,#27275,#27276,#27277,#27278,#27279,
#27280,#27281,#27282),.UNSPECIFIED.,.F.,.F.,(6,1,1,1,1,1,1,1,1,1,1,1,1,
1,1,1,1,1,1,1,1,1,1,1,1,1,1,1,1,1,1,1,1,1,1,1,1,1,1,1,1,1,1,1,1,1,1,1,1,
1,1,1,1,1,1,1,1,1,1,1,1,1,1,1,1,1,1,1,1,6),(0.,0.0142857142857143,0.0285714285714286,
0.0428571428571429,0.0571428571428571,0.0714285714285714,0.0857142857142857,
0.1,0.114285714285714,0.128571428571429,0.142857142857143,0.157142857142857,
0.171428571428571,0.185714285714286,0.2,0.214285714285714,0.228571428571429,
0.242857142857143,0.257142857142857,0.271428571428571,0.285714285714286,
0.3,0.314285714285714,0.328571428571429,0.342857142857143,0.357142857142857,
0.371428571428571,0.385714285714286,0.4,0.414285714285714,0.428571428571429,
0.442857142857143,0.457142857142857,0.471428571428572,0.485714285714286,
0.5,0.514285714285714,0.528571428571429,0.542857142857143,0.557142857142857,
0.571428571428571,0.585714285714286,0.6,0.614285714285714,0.628571428571428,
0.642857142857142,0.657142857142857,0.671428571428571,0.685714285714285,
0.699999999999999,0.714285714285714,0.728571428571428,0.742857142857142,
0.757142857142856,0.771428571428571,0.785714285714285,0.799999999999999,
0.814285714285713,0.828571428571428,0.842857142857142,0.857142857142856,
0.87142857142857,0.885714285714284,0.899999999999999,0.914285714285713,
0.928571428571427,0.942857142857141,0.957142857142856,0.97142857142857,
1.),.UNSPECIFIED.);
#543=B_SPLINE_CURVE_WITH_KNOTS('',5,(#27434,#27435,#27436,#27437,#27438,
#27439,#27440,#27441,#27442,#27443,#27444,#27445,#27446,#27447,#27448,#27449,
#27450,#27451,#27452,#27453,#27454,#27455,#27456,#27457,#27458,#27459,#27460,
#27461,#27462,#27463,#27464,#27465,#27466,#27467,#27468,#27469,#27470,#27471,
#27472,#27473,#27474,#27475,#27476,#27477,#27478,#27479,#27480,#27481,#27482,
#27483,#27484,#27485,#27486,#27487,#27488,#27489,#27490,#27491,#27492,#27493,
#27494,#27495,#27496,#27497,#27498,#27499,#27500,#27501,#27502,#27503,#27504,
#27505,#27506,#27507),.UNSPECIFIED.,.F.,.F.,(6,1,1,1,1,1,1,1,1,1,1,1,1,
1,1,1,1,1,1,1,1,1,1,1,1,1,1,1,1,1,1,1,1,1,1,1,1,1,1,1,1,1,1,1,1,1,1,1,1,
1,1,1,1,1,1,1,1,1,1,1,1,1,1,1,1,1,1,1,1,6),(0.,0.0142857142857143,0.0285714285714286,
0.0428571428571429,0.0571428571428571,0.0714285714285714,0.0857142857142857,
0.1,0.114285714285714,0.128571428571429,0.142857142857143,0.157142857142857,
0.171428571428571,0.185714285714286,0.2,0.214285714285714,0.228571428571429,
0.242857142857143,0.257142857142857,0.271428571428571,0.285714285714286,
0.3,0.314285714285714,0.328571428571429,0.342857142857143,0.357142857142857,
0.371428571428571,0.385714285714286,0.4,0.414285714285714,0.428571428571429,
0.442857142857143,0.457142857142857,0.471428571428572,0.485714285714286,
0.5,0.514285714285714,0.528571428571429,0.542857142857143,0.557142857142857,
0.571428571428571,0.585714285714286,0.6,0.614285714285714,0.628571428571428,
0.642857142857142,0.657142857142857,0.671428571428571,0.685714285714285,
0.699999999999999,0.714285714285714,0.728571428571428,0.742857142857142,
0.757142857142856,0.771428571428571,0.785714285714285,0.799999999999999,
0.814285714285713,0.828571428571428,0.842857142857142,0.857142857142856,
0.87142857142857,0.885714285714284,0.899999999999999,0.914285714285713,
0.928571428571427,0.942857142857141,0.957142857142856,0.97142857142857,
1.),.UNSPECIFIED.);
#544=B_SPLINE_CURVE_WITH_KNOTS('',5,(#27509,#27510,#27511,#27512,#27513,
#27514,#27515,#27516,#27517,#27518,#27519,#27520,#27521,#27522,#27523,#27524,
#27525,#27526,#27527,#27528,#27529,#27530,#27531,#27532,#27533,#27534,#27535,
#27536,#27537,#27538,#27539,#27540,#27541,#27542,#27543,#27544,#27545,#27546,
#27547,#27548,#27549,#27550,#27551,#27552,#27553,#27554,#27555,#27556,#27557,
#27558,#27559,#27560,#27561,#27562,#27563,#27564,#27565,#27566,#27567,#27568,
#27569,#27570,#27571,#27572,#27573,#27574,#27575,#27576,#27577,#27578,#27579,
#27580,#27581,#27582,#27583),.UNSPECIFIED.,.F.,.F.,(6,1,1,1,1,1,1,1,1,1,
1,1,1,1,1,1,1,1,1,1,1,1,1,1,1,1,1,1,1,1,1,1,1,1,1,1,1,1,1,1,1,1,1,1,1,1,
1,1,1,1,1,1,1,1,1,1,1,1,1,1,1,1,1,1,1,1,1,1,1,1,6),(-1.,-0.985714285714284,
-0.97142857142857,-0.957142857142856,-0.942857142857141,-0.928571428571427,
-0.914285714285713,-0.899999999999999,-0.885714285714284,-0.87142857142857,
-0.857142857142856,-0.842857142857142,-0.828571428571428,-0.814285714285713,
-0.799999999999999,-0.785714285714285,-0.771428571428571,-0.757142857142856,
-0.742857142857142,-0.728571428571428,-0.714285714285714,-0.699999999999999,
-0.685714285714285,-0.671428571428571,-0.657142857142857,-0.642857142857142,
-0.628571428571428,-0.614285714285714,-0.6,-0.585714285714286,-0.571428571428571,
-0.557142857142857,-0.542857142857143,-0.528571428571429,-0.514285714285714,
-0.5,-0.485714285714286,-0.471428571428572,-0.457142857142857,-0.442857142857143,
-0.428571428571429,-0.414285714285714,-0.4,-0.385714285714286,-0.371428571428571,
-0.357142857142857,-0.342857142857143,-0.328571428571429,-0.314285714285714,
-0.3,-0.285714285714286,-0.271428571428571,-0.257142857142857,-0.242857142857143,
-0.228571428571429,-0.214285714285714,-0.2,-0.185714285714286,-0.171428571428571,
-0.157142857142857,-0.142857142857143,-0.128571428571429,-0.114285714285714,
-0.1,-0.0857142857142857,-0.0714285714285714,-0.0571428571428571,-0.0428571428571429,
-0.0285714285714286,-0.0142857142857143,0.),.UNSPECIFIED.);
#545=B_SPLINE_CURVE_WITH_KNOTS('',5,(#27741,#27742,#27743,#27744,#27745,
#27746,#27747,#27748,#27749,#27750,#27751,#27752,#27753,#27754,#27755,#27756,
#27757,#27758,#27759,#27760,#27761,#27762,#27763,#27764,#27765,#27766,#27767,
#27768,#27769,#27770,#27771,#27772,#27773,#27774,#27775,#27776,#27777,#27778,
#27779,#27780,#27781,#27782,#27783,#27784,#27785,#27786,#27787,#27788,#27789,
#27790,#27791,#27792,#27793,#27794,#27795,#27796,#27797,#27798,#27799,#27800,
#27801,#27802,#27803,#27804,#27805,#27806,#27807,#27808,#27809,#27810,#27811,
#27812,#27813,#27814),.UNSPECIFIED.,.F.,.F.,(6,1,1,1,1,1,1,1,1,1,1,1,1,
1,1,1,1,1,1,1,1,1,1,1,1,1,1,1,1,1,1,1,1,1,1,1,1,1,1,1,1,1,1,1,1,1,1,1,1,
1,1,1,1,1,1,1,1,1,1,1,1,1,1,1,1,1,1,1,1,6),(0.,0.0142857142857143,0.0285714285714286,
0.0428571428571429,0.0571428571428571,0.0714285714285714,0.0857142857142857,
0.1,0.114285714285714,0.128571428571429,0.142857142857143,0.157142857142857,
0.171428571428571,0.185714285714286,0.2,0.214285714285714,0.228571428571429,
0.242857142857143,0.257142857142857,0.271428571428571,0.285714285714286,
0.3,0.314285714285714,0.328571428571429,0.342857142857143,0.357142857142857,
0.371428571428571,0.385714285714286,0.4,0.414285714285714,0.428571428571429,
0.442857142857143,0.457142857142857,0.471428571428572,0.485714285714286,
0.5,0.514285714285714,0.528571428571429,0.542857142857143,0.557142857142857,
0.571428571428571,0.585714285714286,0.6,0.614285714285714,0.628571428571428,
0.642857142857142,0.657142857142857,0.671428571428571,0.685714285714285,
0.699999999999999,0.714285714285714,0.728571428571428,0.742857142857142,
0.757142857142856,0.771428571428571,0.785714285714285,0.799999999999999,
0.814285714285713,0.828571428571428,0.842857142857142,0.857142857142856,
0.87142857142857,0.885714285714284,0.899999999999999,0.914285714285713,
0.928571428571427,0.942857142857141,0.957142857142856,0.97142857142857,
1.),.UNSPECIFIED.);
#546=B_SPLINE_CURVE_WITH_KNOTS('',5,(#27815,#27816,#27817,#27818,#27819,
#27820,#27821,#27822,#27823,#27824,#27825,#27826,#27827,#27828,#27829,#27830,
#27831,#27832,#27833,#27834,#27835,#27836,#27837,#27838,#27839,#27840,#27841,
#27842,#27843,#27844,#27845,#27846,#27847,#27848,#27849,#27850,#27851,#27852,
#27853,#27854,#27855,#27856,#27857,#27858,#27859,#27860,#27861,#27862,#27863,
#27864,#27865,#27866,#27867,#27868,#27869,#27870,#27871,#27872,#27873,#27874,
#27875,#27876,#27877,#27878,#27879,#27880,#27881,#27882,#27883,#27884,#27885,
#27886,#27887,#27888),.UNSPECIFIED.,.F.,.F.,(6,1,1,1,1,1,1,1,1,1,1,1,1,
1,1,1,1,1,1,1,1,1,1,1,1,1,1,1,1,1,1,1,1,1,1,1,1,1,1,1,1,1,1,1,1,1,1,1,1,
1,1,1,1,1,1,1,1,1,1,1,1,1,1,1,1,1,1,1,1,6),(0.,0.0142857142857143,0.0285714285714286,
0.0428571428571429,0.0571428571428571,0.0714285714285714,0.0857142857142857,
0.1,0.114285714285714,0.128571428571429,0.142857142857143,0.157142857142857,
0.171428571428571,0.185714285714286,0.2,0.214285714285714,0.228571428571429,
0.242857142857143,0.257142857142857,0.271428571428571,0.285714285714286,
0.3,0.314285714285714,0.328571428571429,0.342857142857143,0.357142857142857,
0.371428571428571,0.385714285714286,0.4,0.414285714285714,0.428571428571429,
0.442857142857143,0.457142857142857,0.471428571428572,0.485714285714286,
0.5,0.514285714285714,0.528571428571429,0.542857142857143,0.557142857142857,
0.571428571428571,0.585714285714286,0.6,0.614285714285714,0.628571428571428,
0.642857142857142,0.657142857142857,0.671428571428571,0.685714285714285,
0.699999999999999,0.714285714285714,0.728571428571428,0.742857142857142,
0.757142857142856,0.771428571428571,0.785714285714285,0.799999999999999,
0.814285714285713,0.828571428571428,0.842857142857142,0.857142857142856,
0.87142857142857,0.885714285714284,0.899999999999999,0.914285714285713,
0.928571428571427,0.942857142857141,0.957142857142856,0.97142857142857,
1.),.UNSPECIFIED.);
#547=B_SPLINE_CURVE_WITH_KNOTS('',5,(#28040,#28041,#28042,#28043,#28044,
#28045,#28046,#28047,#28048,#28049,#28050,#28051,#28052,#28053,#28054,#28055,
#28056,#28057,#28058,#28059,#28060,#28061,#28062,#28063,#28064,#28065,#28066,
#28067,#28068,#28069,#28070,#28071,#28072,#28073,#28074,#28075,#28076,#28077,
#28078,#28079,#28080,#28081,#28082,#28083,#28084,#28085,#28086,#28087,#28088,
#28089,#28090,#28091,#28092,#28093,#28094,#28095,#28096,#28097,#28098,#28099,
#28100,#28101,#28102,#28103,#28104,#28105,#28106,#28107,#28108,#28109,#28110,
#28111,#28112,#28113),.UNSPECIFIED.,.F.,.F.,(6,1,1,1,1,1,1,1,1,1,1,1,1,
1,1,1,1,1,1,1,1,1,1,1,1,1,1,1,1,1,1,1,1,1,1,1,1,1,1,1,1,1,1,1,1,1,1,1,1,
1,1,1,1,1,1,1,1,1,1,1,1,1,1,1,1,1,1,1,1,6),(0.,0.0142857142857143,0.0285714285714286,
0.0428571428571429,0.0571428571428571,0.0714285714285714,0.0857142857142857,
0.1,0.114285714285714,0.128571428571429,0.142857142857143,0.157142857142857,
0.171428571428571,0.185714285714286,0.2,0.214285714285714,0.228571428571429,
0.242857142857143,0.257142857142857,0.271428571428571,0.285714285714286,
0.3,0.314285714285714,0.328571428571429,0.342857142857143,0.357142857142857,
0.371428571428571,0.385714285714286,0.4,0.414285714285714,0.428571428571429,
0.442857142857143,0.457142857142857,0.471428571428572,0.485714285714286,
0.5,0.514285714285714,0.528571428571429,0.542857142857143,0.557142857142857,
0.571428571428571,0.585714285714286,0.6,0.614285714285714,0.628571428571428,
0.642857142857142,0.657142857142857,0.671428571428571,0.685714285714285,
0.699999999999999,0.714285714285714,0.728571428571428,0.742857142857142,
0.757142857142856,0.771428571428571,0.785714285714285,0.799999999999999,
0.814285714285713,0.828571428571428,0.842857142857142,0.857142857142856,
0.87142857142857,0.885714285714284,0.899999999999999,0.914285714285713,
0.928571428571427,0.942857142857141,0.957142857142856,0.97142857142857,
1.),.UNSPECIFIED.);
#548=B_SPLINE_CURVE_WITH_KNOTS('',5,(#28115,#28116,#28117,#28118,#28119,
#28120,#28121,#28122,#28123,#28124,#28125,#28126,#28127,#28128,#28129,#28130,
#28131,#28132,#28133,#28134,#28135,#28136,#28137,#28138,#28139,#28140,#28141,
#28142,#28143,#28144,#28145,#28146,#28147,#28148,#28149,#28150,#28151,#28152,
#28153,#28154,#28155,#28156,#28157,#28158,#28159,#28160,#28161,#28162,#28163,
#28164,#28165,#28166,#28167,#28168,#28169,#28170,#28171,#28172,#28173,#28174,
#28175,#28176,#28177,#28178,#28179,#28180,#28181,#28182,#28183,#28184,#28185,
#28186,#28187,#28188,#28189),.UNSPECIFIED.,.F.,.F.,(6,1,1,1,1,1,1,1,1,1,
1,1,1,1,1,1,1,1,1,1,1,1,1,1,1,1,1,1,1,1,1,1,1,1,1,1,1,1,1,1,1,1,1,1,1,1,
1,1,1,1,1,1,1,1,1,1,1,1,1,1,1,1,1,1,1,1,1,1,1,1,6),(-1.,-0.985714285714284,
-0.97142857142857,-0.957142857142856,-0.942857142857141,-0.928571428571427,
-0.914285714285713,-0.899999999999999,-0.885714285714284,-0.87142857142857,
-0.857142857142856,-0.842857142857142,-0.828571428571428,-0.814285714285713,
-0.799999999999999,-0.785714285714285,-0.771428571428571,-0.757142857142856,
-0.742857142857142,-0.728571428571428,-0.714285714285714,-0.699999999999999,
-0.685714285714285,-0.671428571428571,-0.657142857142857,-0.642857142857142,
-0.628571428571428,-0.614285714285714,-0.6,-0.585714285714286,-0.571428571428571,
-0.557142857142857,-0.542857142857143,-0.528571428571429,-0.514285714285714,
-0.5,-0.485714285714286,-0.471428571428572,-0.457142857142857,-0.442857142857143,
-0.428571428571429,-0.414285714285714,-0.4,-0.385714285714286,-0.371428571428571,
-0.357142857142857,-0.342857142857143,-0.328571428571429,-0.314285714285714,
-0.3,-0.285714285714286,-0.271428571428571,-0.257142857142857,-0.242857142857143,
-0.228571428571429,-0.214285714285714,-0.2,-0.185714285714286,-0.171428571428571,
-0.157142857142857,-0.142857142857143,-0.128571428571429,-0.114285714285714,
-0.1,-0.0857142857142857,-0.0714285714285714,-0.0571428571428571,-0.0428571428571429,
-0.0285714285714286,-0.0142857142857143,0.),.UNSPECIFIED.);
#549=B_SPLINE_CURVE_WITH_KNOTS('',5,(#28347,#28348,#28349,#28350,#28351,
#28352,#28353,#28354,#28355,#28356,#28357,#28358,#28359,#28360,#28361,#28362,
#28363,#28364,#28365,#28366,#28367,#28368,#28369,#28370,#28371,#28372,#28373,
#28374,#28375,#28376,#28377,#28378,#28379,#28380,#28381,#28382,#28383,#28384,
#28385,#28386,#28387,#28388,#28389,#28390,#28391,#28392,#28393,#28394,#28395,
#28396,#28397,#28398,#28399,#28400,#28401,#28402,#28403,#28404,#28405,#28406,
#28407,#28408,#28409,#28410,#28411,#28412,#28413,#28414,#28415,#28416,#28417,
#28418,#28419,#28420),.UNSPECIFIED.,.F.,.F.,(6,1,1,1,1,1,1,1,1,1,1,1,1,
1,1,1,1,1,1,1,1,1,1,1,1,1,1,1,1,1,1,1,1,1,1,1,1,1,1,1,1,1,1,1,1,1,1,1,1,
1,1,1,1,1,1,1,1,1,1,1,1,1,1,1,1,1,1,1,1,6),(0.,0.0142857142857143,0.0285714285714286,
0.0428571428571429,0.0571428571428571,0.0714285714285714,0.0857142857142857,
0.1,0.114285714285714,0.128571428571429,0.142857142857143,0.157142857142857,
0.171428571428571,0.185714285714286,0.2,0.214285714285714,0.228571428571429,
0.242857142857143,0.257142857142857,0.271428571428571,0.285714285714286,
0.3,0.314285714285714,0.328571428571429,0.342857142857143,0.357142857142857,
0.371428571428571,0.385714285714286,0.4,0.414285714285714,0.428571428571429,
0.442857142857143,0.457142857142857,0.471428571428572,0.485714285714286,
0.5,0.514285714285714,0.528571428571429,0.542857142857143,0.557142857142857,
0.571428571428571,0.585714285714286,0.6,0.614285714285714,0.628571428571428,
0.642857142857142,0.657142857142857,0.671428571428571,0.685714285714285,
0.699999999999999,0.714285714285714,0.728571428571428,0.742857142857142,
0.757142857142856,0.771428571428571,0.785714285714285,0.799999999999999,
0.814285714285713,0.828571428571428,0.842857142857142,0.857142857142856,
0.87142857142857,0.885714285714284,0.899999999999999,0.914285714285713,
0.928571428571427,0.942857142857141,0.957142857142856,0.97142857142857,
1.),.UNSPECIFIED.);
#550=B_SPLINE_CURVE_WITH_KNOTS('',5,(#28421,#28422,#28423,#28424,#28425,
#28426,#28427,#28428,#28429,#28430,#28431,#28432,#28433,#28434,#28435,#28436,
#28437,#28438,#28439,#28440,#28441,#28442,#28443,#28444,#28445,#28446,#28447,
#28448,#28449,#28450,#28451,#28452,#28453,#28454,#28455,#28456,#28457,#28458,
#28459,#28460,#28461,#28462,#28463,#28464,#28465,#28466,#28467,#28468,#28469,
#28470,#28471,#28472,#28473,#28474,#28475,#28476,#28477,#28478,#28479,#28480,
#28481,#28482,#28483,#28484,#28485,#28486,#28487,#28488,#28489,#28490,#28491,
#28492,#28493,#28494),.UNSPECIFIED.,.F.,.F.,(6,1,1,1,1,1,1,1,1,1,1,1,1,
1,1,1,1,1,1,1,1,1,1,1,1,1,1,1,1,1,1,1,1,1,1,1,1,1,1,1,1,1,1,1,1,1,1,1,1,
1,1,1,1,1,1,1,1,1,1,1,1,1,1,1,1,1,1,1,1,6),(0.,0.0142857142857143,0.0285714285714286,
0.0428571428571429,0.0571428571428571,0.0714285714285714,0.0857142857142857,
0.1,0.114285714285714,0.128571428571429,0.142857142857143,0.157142857142857,
0.171428571428571,0.185714285714286,0.2,0.214285714285714,0.228571428571429,
0.242857142857143,0.257142857142857,0.271428571428571,0.285714285714286,
0.3,0.314285714285714,0.328571428571429,0.342857142857143,0.357142857142857,
0.371428571428571,0.385714285714286,0.4,0.414285714285714,0.428571428571429,
0.442857142857143,0.457142857142857,0.471428571428572,0.485714285714286,
0.5,0.514285714285714,0.528571428571429,0.542857142857143,0.557142857142857,
0.571428571428571,0.585714285714286,0.6,0.614285714285714,0.628571428571428,
0.642857142857142,0.657142857142857,0.671428571428571,0.685714285714285,
0.699999999999999,0.714285714285714,0.728571428571428,0.742857142857142,
0.757142857142856,0.771428571428571,0.785714285714285,0.799999999999999,
0.814285714285713,0.828571428571428,0.842857142857142,0.857142857142856,
0.87142857142857,0.885714285714284,0.899999999999999,0.914285714285713,
0.928571428571427,0.942857142857141,0.957142857142856,0.97142857142857,
1.),.UNSPECIFIED.);
#551=B_SPLINE_CURVE_WITH_KNOTS('',5,(#28646,#28647,#28648,#28649,#28650,
#28651,#28652,#28653,#28654,#28655,#28656,#28657,#28658,#28659,#28660,#28661,
#28662,#28663,#28664,#28665,#28666,#28667,#28668,#28669,#28670,#28671,#28672,
#28673,#28674,#28675,#28676,#28677,#28678,#28679,#28680,#28681,#28682,#28683,
#28684,#28685,#28686,#28687,#28688,#28689,#28690,#28691,#28692,#28693,#28694,
#28695,#28696,#28697,#28698,#28699,#28700,#28701,#28702,#28703,#28704,#28705,
#28706,#28707,#28708,#28709,#28710,#28711,#28712,#28713,#28714,#28715,#28716,
#28717,#28718,#28719),.UNSPECIFIED.,.F.,.F.,(6,1,1,1,1,1,1,1,1,1,1,1,1,
1,1,1,1,1,1,1,1,1,1,1,1,1,1,1,1,1,1,1,1,1,1,1,1,1,1,1,1,1,1,1,1,1,1,1,1,
1,1,1,1,1,1,1,1,1,1,1,1,1,1,1,1,1,1,1,1,6),(0.,0.0142857142857143,0.0285714285714286,
0.0428571428571429,0.0571428571428571,0.0714285714285714,0.0857142857142857,
0.1,0.114285714285714,0.128571428571429,0.142857142857143,0.157142857142857,
0.171428571428571,0.185714285714286,0.2,0.214285714285714,0.228571428571429,
0.242857142857143,0.257142857142857,0.271428571428571,0.285714285714286,
0.3,0.314285714285714,0.328571428571429,0.342857142857143,0.357142857142857,
0.371428571428571,0.385714285714286,0.4,0.414285714285714,0.428571428571429,
0.442857142857143,0.457142857142857,0.471428571428572,0.485714285714286,
0.5,0.514285714285714,0.528571428571429,0.542857142857143,0.557142857142857,
0.571428571428571,0.585714285714286,0.6,0.614285714285714,0.628571428571428,
0.642857142857142,0.657142857142857,0.671428571428571,0.685714285714285,
0.699999999999999,0.714285714285714,0.728571428571428,0.742857142857142,
0.757142857142856,0.771428571428571,0.785714285714285,0.799999999999999,
0.814285714285713,0.828571428571428,0.842857142857142,0.857142857142856,
0.87142857142857,0.885714285714284,0.899999999999999,0.914285714285713,
0.928571428571427,0.942857142857141,0.957142857142856,0.97142857142857,
1.),.UNSPECIFIED.);
#552=B_SPLINE_CURVE_WITH_KNOTS('',5,(#28721,#28722,#28723,#28724,#28725,
#28726,#28727,#28728,#28729,#28730,#28731,#28732,#28733,#28734,#28735,#28736,
#28737,#28738,#28739,#28740,#28741,#28742,#28743,#28744,#28745,#28746,#28747,
#28748,#28749,#28750,#28751,#28752,#28753,#28754,#28755,#28756,#28757,#28758,
#28759,#28760,#28761,#28762,#28763,#28764,#28765,#28766,#28767,#28768,#28769,
#28770,#28771,#28772,#28773,#28774,#28775,#28776,#28777,#28778,#28779,#28780,
#28781,#28782,#28783,#28784,#28785,#28786,#28787,#28788,#28789,#28790,#28791,
#28792,#28793,#28794,#28795),.UNSPECIFIED.,.F.,.F.,(6,1,1,1,1,1,1,1,1,1,
1,1,1,1,1,1,1,1,1,1,1,1,1,1,1,1,1,1,1,1,1,1,1,1,1,1,1,1,1,1,1,1,1,1,1,1,
1,1,1,1,1,1,1,1,1,1,1,1,1,1,1,1,1,1,1,1,1,1,1,1,6),(-1.,-0.985714285714284,
-0.97142857142857,-0.957142857142856,-0.942857142857141,-0.928571428571427,
-0.914285714285713,-0.899999999999999,-0.885714285714284,-0.87142857142857,
-0.857142857142856,-0.842857142857142,-0.828571428571428,-0.814285714285713,
-0.799999999999999,-0.785714285714285,-0.771428571428571,-0.757142857142856,
-0.742857142857142,-0.728571428571428,-0.714285714285714,-0.699999999999999,
-0.685714285714285,-0.671428571428571,-0.657142857142857,-0.642857142857142,
-0.628571428571428,-0.614285714285714,-0.6,-0.585714285714286,-0.571428571428571,
-0.557142857142857,-0.542857142857143,-0.528571428571429,-0.514285714285714,
-0.5,-0.485714285714286,-0.471428571428572,-0.457142857142857,-0.442857142857143,
-0.428571428571429,-0.414285714285714,-0.4,-0.385714285714286,-0.371428571428571,
-0.357142857142857,-0.342857142857143,-0.328571428571429,-0.314285714285714,
-0.3,-0.285714285714286,-0.271428571428571,-0.257142857142857,-0.242857142857143,
-0.228571428571429,-0.214285714285714,-0.2,-0.185714285714286,-0.171428571428571,
-0.157142857142857,-0.142857142857143,-0.128571428571429,-0.114285714285714,
-0.1,-0.0857142857142857,-0.0714285714285714,-0.0571428571428571,-0.0428571428571429,
-0.0285714285714286,-0.0142857142857143,0.),.UNSPECIFIED.);
#553=B_SPLINE_CURVE_WITH_KNOTS('',5,(#28953,#28954,#28955,#28956,#28957,
#28958,#28959,#28960,#28961,#28962,#28963,#28964,#28965,#28966,#28967,#28968,
#28969,#28970,#28971,#28972,#28973,#28974,#28975,#28976,#28977,#28978,#28979,
#28980,#28981,#28982,#28983,#28984,#28985,#28986,#28987,#28988,#28989,#28990,
#28991,#28992,#28993,#28994,#28995,#28996,#28997,#28998,#28999,#29000,#29001,
#29002,#29003,#29004,#29005,#29006,#29007,#29008,#29009,#29010,#29011,#29012,
#29013,#29014,#29015,#29016,#29017,#29018,#29019,#29020,#29021,#29022,#29023,
#29024,#29025,#29026),.UNSPECIFIED.,.F.,.F.,(6,1,1,1,1,1,1,1,1,1,1,1,1,
1,1,1,1,1,1,1,1,1,1,1,1,1,1,1,1,1,1,1,1,1,1,1,1,1,1,1,1,1,1,1,1,1,1,1,1,
1,1,1,1,1,1,1,1,1,1,1,1,1,1,1,1,1,1,1,1,6),(0.,0.0142857142857143,0.0285714285714286,
0.0428571428571429,0.0571428571428571,0.0714285714285714,0.0857142857142857,
0.1,0.114285714285714,0.128571428571429,0.142857142857143,0.157142857142857,
0.171428571428571,0.185714285714286,0.2,0.214285714285714,0.228571428571429,
0.242857142857143,0.257142857142857,0.271428571428571,0.285714285714286,
0.3,0.314285714285714,0.328571428571429,0.342857142857143,0.357142857142857,
0.371428571428571,0.385714285714286,0.4,0.414285714285714,0.428571428571429,
0.442857142857143,0.457142857142857,0.471428571428572,0.485714285714286,
0.5,0.514285714285714,0.528571428571429,0.542857142857143,0.557142857142857,
0.571428571428571,0.585714285714286,0.6,0.614285714285714,0.628571428571428,
0.642857142857142,0.657142857142857,0.671428571428571,0.685714285714285,
0.699999999999999,0.714285714285714,0.728571428571428,0.742857142857142,
0.757142857142856,0.771428571428571,0.785714285714285,0.799999999999999,
0.814285714285713,0.828571428571428,0.842857142857142,0.857142857142856,
0.87142857142857,0.885714285714284,0.899999999999999,0.914285714285713,
0.928571428571427,0.942857142857141,0.957142857142856,0.97142857142857,
1.),.UNSPECIFIED.);
#554=B_SPLINE_CURVE_WITH_KNOTS('',5,(#29027,#29028,#29029,#29030,#29031,
#29032,#29033,#29034,#29035,#29036,#29037,#29038,#29039,#29040,#29041,#29042,
#29043,#29044,#29045,#29046,#29047,#29048,#29049,#29050,#29051,#29052,#29053,
#29054,#29055,#29056,#29057,#29058,#29059,#29060,#29061,#29062,#29063,#29064,
#29065,#29066,#29067,#29068,#29069,#29070,#29071,#29072,#29073,#29074,#29075,
#29076,#29077,#29078,#29079,#29080,#29081,#29082,#29083,#29084,#29085,#29086,
#29087,#29088,#29089,#29090,#29091,#29092,#29093,#29094,#29095,#29096,#29097,
#29098,#29099,#29100),.UNSPECIFIED.,.F.,.F.,(6,1,1,1,1,1,1,1,1,1,1,1,1,
1,1,1,1,1,1,1,1,1,1,1,1,1,1,1,1,1,1,1,1,1,1,1,1,1,1,1,1,1,1,1,1,1,1,1,1,
1,1,1,1,1,1,1,1,1,1,1,1,1,1,1,1,1,1,1,1,6),(0.,0.0142857142857143,0.0285714285714286,
0.0428571428571429,0.0571428571428571,0.0714285714285714,0.0857142857142857,
0.1,0.114285714285714,0.128571428571429,0.142857142857143,0.157142857142857,
0.171428571428571,0.185714285714286,0.2,0.214285714285714,0.228571428571429,
0.242857142857143,0.257142857142857,0.271428571428571,0.285714285714286,
0.3,0.314285714285714,0.328571428571429,0.342857142857143,0.357142857142857,
0.371428571428571,0.385714285714286,0.4,0.414285714285714,0.428571428571429,
0.442857142857143,0.457142857142857,0.471428571428572,0.485714285714286,
0.5,0.514285714285714,0.528571428571429,0.542857142857143,0.557142857142857,
0.571428571428571,0.585714285714286,0.6,0.614285714285714,0.628571428571428,
0.642857142857142,0.657142857142857,0.671428571428571,0.685714285714285,
0.699999999999999,0.714285714285714,0.728571428571428,0.742857142857142,
0.757142857142856,0.771428571428571,0.785714285714285,0.799999999999999,
0.814285714285713,0.828571428571428,0.842857142857142,0.857142857142856,
0.87142857142857,0.885714285714284,0.899999999999999,0.914285714285713,
0.928571428571427,0.942857142857141,0.957142857142856,0.97142857142857,
1.),.UNSPECIFIED.);
#555=B_SPLINE_CURVE_WITH_KNOTS('',5,(#29252,#29253,#29254,#29255,#29256,
#29257,#29258,#29259,#29260,#29261,#29262,#29263,#29264,#29265,#29266,#29267,
#29268,#29269,#29270,#29271,#29272,#29273,#29274,#29275,#29276,#29277,#29278,
#29279,#29280,#29281,#29282,#29283,#29284,#29285,#29286,#29287,#29288,#29289,
#29290,#29291,#29292,#29293,#29294,#29295,#29296,#29297,#29298,#29299,#29300,
#29301,#29302,#29303,#29304,#29305,#29306,#29307,#29308,#29309,#29310,#29311,
#29312,#29313,#29314,#29315,#29316,#29317,#29318,#29319,#29320,#29321,#29322,
#29323,#29324,#29325),.UNSPECIFIED.,.F.,.F.,(6,1,1,1,1,1,1,1,1,1,1,1,1,
1,1,1,1,1,1,1,1,1,1,1,1,1,1,1,1,1,1,1,1,1,1,1,1,1,1,1,1,1,1,1,1,1,1,1,1,
1,1,1,1,1,1,1,1,1,1,1,1,1,1,1,1,1,1,1,1,6),(0.,0.0142857142857143,0.0285714285714286,
0.0428571428571429,0.0571428571428571,0.0714285714285714,0.0857142857142857,
0.1,0.114285714285714,0.128571428571429,0.142857142857143,0.157142857142857,
0.171428571428571,0.185714285714286,0.2,0.214285714285714,0.228571428571429,
0.242857142857143,0.257142857142857,0.271428571428571,0.285714285714286,
0.3,0.314285714285714,0.328571428571429,0.342857142857143,0.357142857142857,
0.371428571428571,0.385714285714286,0.4,0.414285714285714,0.428571428571429,
0.442857142857143,0.457142857142857,0.471428571428572,0.485714285714286,
0.5,0.514285714285714,0.528571428571429,0.542857142857143,0.557142857142857,
0.571428571428571,0.585714285714286,0.6,0.614285714285714,0.628571428571428,
0.642857142857142,0.657142857142857,0.671428571428571,0.685714285714285,
0.699999999999999,0.714285714285714,0.728571428571428,0.742857142857142,
0.757142857142856,0.771428571428571,0.785714285714285,0.799999999999999,
0.814285714285713,0.828571428571428,0.842857142857142,0.857142857142856,
0.87142857142857,0.885714285714284,0.899999999999999,0.914285714285713,
0.928571428571427,0.942857142857141,0.957142857142856,0.97142857142857,
1.),.UNSPECIFIED.);
#556=B_SPLINE_CURVE_WITH_KNOTS('',5,(#29327,#29328,#29329,#29330,#29331,
#29332,#29333,#29334,#29335,#29336,#29337,#29338,#29339,#29340,#29341,#29342,
#29343,#29344,#29345,#29346,#29347,#29348,#29349,#29350,#29351,#29352,#29353,
#29354,#29355,#29356,#29357,#29358,#29359,#29360,#29361,#29362,#29363,#29364,
#29365,#29366,#29367,#29368,#29369,#29370,#29371,#29372,#29373,#29374,#29375,
#29376,#29377,#29378,#29379,#29380,#29381,#29382,#29383,#29384,#29385,#29386,
#29387,#29388,#29389,#29390,#29391,#29392,#29393,#29394,#29395,#29396,#29397,
#29398,#29399,#29400,#29401),.UNSPECIFIED.,.F.,.F.,(6,1,1,1,1,1,1,1,1,1,
1,1,1,1,1,1,1,1,1,1,1,1,1,1,1,1,1,1,1,1,1,1,1,1,1,1,1,1,1,1,1,1,1,1,1,1,
1,1,1,1,1,1,1,1,1,1,1,1,1,1,1,1,1,1,1,1,1,1,1,1,6),(-1.,-0.985714285714284,
-0.97142857142857,-0.957142857142856,-0.942857142857141,-0.928571428571427,
-0.914285714285713,-0.899999999999999,-0.885714285714284,-0.87142857142857,
-0.857142857142856,-0.842857142857142,-0.828571428571428,-0.814285714285713,
-0.799999999999999,-0.785714285714285,-0.771428571428571,-0.757142857142856,
-0.742857142857142,-0.728571428571428,-0.714285714285714,-0.699999999999999,
-0.685714285714285,-0.671428571428571,-0.657142857142857,-0.642857142857142,
-0.628571428571428,-0.614285714285714,-0.6,-0.585714285714286,-0.571428571428571,
-0.557142857142857,-0.542857142857143,-0.528571428571429,-0.514285714285714,
-0.5,-0.485714285714286,-0.471428571428572,-0.457142857142857,-0.442857142857143,
-0.428571428571429,-0.414285714285714,-0.4,-0.385714285714286,-0.371428571428571,
-0.357142857142857,-0.342857142857143,-0.328571428571429,-0.314285714285714,
-0.3,-0.285714285714286,-0.271428571428571,-0.257142857142857,-0.242857142857143,
-0.228571428571429,-0.214285714285714,-0.2,-0.185714285714286,-0.171428571428571,
-0.157142857142857,-0.142857142857143,-0.128571428571429,-0.114285714285714,
-0.1,-0.0857142857142857,-0.0714285714285714,-0.0571428571428571,-0.0428571428571429,
-0.0285714285714286,-0.0142857142857143,0.),.UNSPECIFIED.);
#557=B_SPLINE_CURVE_WITH_KNOTS('',5,(#29559,#29560,#29561,#29562,#29563,
#29564,#29565,#29566,#29567,#29568,#29569,#29570,#29571,#29572,#29573,#29574,
#29575,#29576,#29577,#29578,#29579,#29580,#29581,#29582,#29583,#29584,#29585,
#29586,#29587,#29588,#29589,#29590,#29591,#29592,#29593,#29594,#29595,#29596,
#29597,#29598,#29599,#29600,#29601,#29602,#29603,#29604,#29605,#29606,#29607,
#29608,#29609,#29610,#29611,#29612,#29613,#29614,#29615,#29616,#29617,#29618,
#29619,#29620,#29621,#29622,#29623,#29624,#29625,#29626,#29627,#29628,#29629,
#29630,#29631,#29632),.UNSPECIFIED.,.F.,.F.,(6,1,1,1,1,1,1,1,1,1,1,1,1,
1,1,1,1,1,1,1,1,1,1,1,1,1,1,1,1,1,1,1,1,1,1,1,1,1,1,1,1,1,1,1,1,1,1,1,1,
1,1,1,1,1,1,1,1,1,1,1,1,1,1,1,1,1,1,1,1,6),(0.,0.0142857142857143,0.0285714285714286,
0.0428571428571429,0.0571428571428571,0.0714285714285714,0.0857142857142857,
0.1,0.114285714285714,0.128571428571429,0.142857142857143,0.157142857142857,
0.171428571428571,0.185714285714286,0.2,0.214285714285714,0.228571428571429,
0.242857142857143,0.257142857142857,0.271428571428571,0.285714285714286,
0.3,0.314285714285714,0.328571428571429,0.342857142857143,0.357142857142857,
0.371428571428571,0.385714285714286,0.4,0.414285714285714,0.428571428571429,
0.442857142857143,0.457142857142857,0.471428571428572,0.485714285714286,
0.5,0.514285714285714,0.528571428571429,0.542857142857143,0.557142857142857,
0.571428571428571,0.585714285714286,0.6,0.614285714285714,0.628571428571428,
0.642857142857142,0.657142857142857,0.671428571428571,0.685714285714285,
0.699999999999999,0.714285714285714,0.728571428571428,0.742857142857142,
0.757142857142856,0.771428571428571,0.785714285714285,0.799999999999999,
0.814285714285713,0.828571428571428,0.842857142857142,0.857142857142856,
0.87142857142857,0.885714285714284,0.899999999999999,0.914285714285713,
0.928571428571427,0.942857142857141,0.957142857142856,0.97142857142857,
1.),.UNSPECIFIED.);
#558=B_SPLINE_CURVE_WITH_KNOTS('',5,(#29633,#29634,#29635,#29636,#29637,
#29638,#29639,#29640,#29641,#29642,#29643,#29644,#29645,#29646,#29647,#29648,
#29649,#29650,#29651,#29652,#29653,#29654,#29655,#29656,#29657,#29658,#29659,
#29660,#29661,#29662,#29663,#29664,#29665,#29666,#29667,#29668,#29669,#29670,
#29671,#29672,#29673,#29674,#29675,#29676,#29677,#29678,#29679,#29680,#29681,
#29682,#29683,#29684,#29685,#29686,#29687,#29688,#29689,#29690,#29691,#29692,
#29693,#29694,#29695,#29696,#29697,#29698,#29699,#29700,#29701,#29702,#29703,
#29704,#29705,#29706),.UNSPECIFIED.,.F.,.F.,(6,1,1,1,1,1,1,1,1,1,1,1,1,
1,1,1,1,1,1,1,1,1,1,1,1,1,1,1,1,1,1,1,1,1,1,1,1,1,1,1,1,1,1,1,1,1,1,1,1,
1,1,1,1,1,1,1,1,1,1,1,1,1,1,1,1,1,1,1,1,6),(0.,0.0142857142857143,0.0285714285714286,
0.0428571428571429,0.0571428571428571,0.0714285714285714,0.0857142857142857,
0.1,0.114285714285714,0.128571428571429,0.142857142857143,0.157142857142857,
0.171428571428571,0.185714285714286,0.2,0.214285714285714,0.228571428571429,
0.242857142857143,0.257142857142857,0.271428571428571,0.285714285714286,
0.3,0.314285714285714,0.328571428571429,0.342857142857143,0.357142857142857,
0.371428571428571,0.385714285714286,0.4,0.414285714285714,0.428571428571429,
0.442857142857143,0.457142857142857,0.471428571428572,0.485714285714286,
0.5,0.514285714285714,0.528571428571429,0.542857142857143,0.557142857142857,
0.571428571428571,0.585714285714286,0.6,0.614285714285714,0.628571428571428,
0.642857142857142,0.657142857142857,0.671428571428571,0.685714285714285,
0.699999999999999,0.714285714285714,0.728571428571428,0.742857142857142,
0.757142857142856,0.771428571428571,0.785714285714285,0.799999999999999,
0.814285714285713,0.828571428571428,0.842857142857142,0.857142857142856,
0.87142857142857,0.885714285714284,0.899999999999999,0.914285714285713,
0.928571428571427,0.942857142857141,0.957142857142856,0.97142857142857,
1.),.UNSPECIFIED.);
#559=B_SPLINE_CURVE_WITH_KNOTS('',5,(#29858,#29859,#29860,#29861,#29862,
#29863,#29864,#29865,#29866,#29867,#29868,#29869,#29870,#29871,#29872,#29873,
#29874,#29875,#29876,#29877,#29878,#29879,#29880,#29881,#29882,#29883,#29884,
#29885,#29886,#29887,#29888,#29889,#29890,#29891,#29892,#29893,#29894,#29895,
#29896,#29897,#29898,#29899,#29900,#29901,#29902,#29903,#29904,#29905,#29906,
#29907,#29908,#29909,#29910,#29911,#29912,#29913,#29914,#29915,#29916,#29917,
#29918,#29919,#29920,#29921,#29922,#29923,#29924,#29925,#29926,#29927,#29928,
#29929,#29930,#29931),.UNSPECIFIED.,.F.,.F.,(6,1,1,1,1,1,1,1,1,1,1,1,1,
1,1,1,1,1,1,1,1,1,1,1,1,1,1,1,1,1,1,1,1,1,1,1,1,1,1,1,1,1,1,1,1,1,1,1,1,
1,1,1,1,1,1,1,1,1,1,1,1,1,1,1,1,1,1,1,1,6),(0.,0.0142857142857143,0.0285714285714286,
0.0428571428571429,0.0571428571428571,0.0714285714285714,0.0857142857142857,
0.1,0.114285714285714,0.128571428571429,0.142857142857143,0.157142857142857,
0.171428571428571,0.185714285714286,0.2,0.214285714285714,0.228571428571429,
0.242857142857143,0.257142857142857,0.271428571428571,0.285714285714286,
0.3,0.314285714285714,0.328571428571429,0.342857142857143,0.357142857142857,
0.371428571428571,0.385714285714286,0.4,0.414285714285714,0.428571428571429,
0.442857142857143,0.457142857142857,0.471428571428572,0.485714285714286,
0.5,0.514285714285714,0.528571428571429,0.542857142857143,0.557142857142857,
0.571428571428571,0.585714285714286,0.6,0.614285714285714,0.628571428571428,
0.642857142857142,0.657142857142857,0.671428571428571,0.685714285714285,
0.699999999999999,0.714285714285714,0.728571428571428,0.742857142857142,
0.757142857142856,0.771428571428571,0.785714285714285,0.799999999999999,
0.814285714285713,0.828571428571428,0.842857142857142,0.857142857142856,
0.87142857142857,0.885714285714284,0.899999999999999,0.914285714285713,
0.928571428571427,0.942857142857141,0.957142857142856,0.97142857142857,
1.),.UNSPECIFIED.);
#560=B_SPLINE_CURVE_WITH_KNOTS('',5,(#29933,#29934,#29935,#29936,#29937,
#29938,#29939,#29940,#29941,#29942,#29943,#29944,#29945,#29946,#29947,#29948,
#29949,#29950,#29951,#29952,#29953,#29954,#29955,#29956,#29957,#29958,#29959,
#29960,#29961,#29962,#29963,#29964,#29965,#29966,#29967,#29968,#29969,#29970,
#29971,#29972,#29973,#29974,#29975,#29976,#29977,#29978,#29979,#29980,#29981,
#29982,#29983,#29984,#29985,#29986,#29987,#29988,#29989,#29990,#29991,#29992,
#29993,#29994,#29995,#29996,#29997,#29998,#29999,#30000,#30001,#30002,#30003,
#30004,#30005,#30006,#30007),.UNSPECIFIED.,.F.,.F.,(6,1,1,1,1,1,1,1,1,1,
1,1,1,1,1,1,1,1,1,1,1,1,1,1,1,1,1,1,1,1,1,1,1,1,1,1,1,1,1,1,1,1,1,1,1,1,
1,1,1,1,1,1,1,1,1,1,1,1,1,1,1,1,1,1,1,1,1,1,1,1,6),(-1.,-0.985714285714284,
-0.97142857142857,-0.957142857142856,-0.942857142857141,-0.928571428571427,
-0.914285714285713,-0.899999999999999,-0.885714285714284,-0.87142857142857,
-0.857142857142856,-0.842857142857142,-0.828571428571428,-0.814285714285713,
-0.799999999999999,-0.785714285714285,-0.771428571428571,-0.757142857142856,
-0.742857142857142,-0.728571428571428,-0.714285714285714,-0.699999999999999,
-0.685714285714285,-0.671428571428571,-0.657142857142857,-0.642857142857142,
-0.628571428571428,-0.614285714285714,-0.6,-0.585714285714286,-0.571428571428571,
-0.557142857142857,-0.542857142857143,-0.528571428571429,-0.514285714285714,
-0.5,-0.485714285714286,-0.471428571428572,-0.457142857142857,-0.442857142857143,
-0.428571428571429,-0.414285714285714,-0.4,-0.385714285714286,-0.371428571428571,
-0.357142857142857,-0.342857142857143,-0.328571428571429,-0.314285714285714,
-0.3,-0.285714285714286,-0.271428571428571,-0.257142857142857,-0.242857142857143,
-0.228571428571429,-0.214285714285714,-0.2,-0.185714285714286,-0.171428571428571,
-0.157142857142857,-0.142857142857143,-0.128571428571429,-0.114285714285714,
-0.1,-0.0857142857142857,-0.0714285714285714,-0.0571428571428571,-0.0428571428571429,
-0.0285714285714286,-0.0142857142857143,0.),.UNSPECIFIED.);
#561=B_SPLINE_CURVE_WITH_KNOTS('',5,(#30165,#30166,#30167,#30168,#30169,
#30170,#30171,#30172,#30173,#30174,#30175,#30176,#30177,#30178,#30179,#30180,
#30181,#30182,#30183,#30184,#30185,#30186,#30187,#30188,#30189,#30190,#30191,
#30192,#30193,#30194,#30195,#30196,#30197,#30198,#30199,#30200,#30201,#30202,
#30203,#30204,#30205,#30206,#30207,#30208,#30209,#30210,#30211,#30212,#30213,
#30214,#30215,#30216,#30217,#30218,#30219,#30220,#30221,#30222,#30223,#30224,
#30225,#30226,#30227,#30228,#30229,#30230,#30231,#30232,#30233,#30234,#30235,
#30236,#30237,#30238),.UNSPECIFIED.,.F.,.F.,(6,1,1,1,1,1,1,1,1,1,1,1,1,
1,1,1,1,1,1,1,1,1,1,1,1,1,1,1,1,1,1,1,1,1,1,1,1,1,1,1,1,1,1,1,1,1,1,1,1,
1,1,1,1,1,1,1,1,1,1,1,1,1,1,1,1,1,1,1,1,6),(0.,0.0142857142857143,0.0285714285714286,
0.0428571428571429,0.0571428571428571,0.0714285714285714,0.0857142857142857,
0.1,0.114285714285714,0.128571428571429,0.142857142857143,0.157142857142857,
0.171428571428571,0.185714285714286,0.2,0.214285714285714,0.228571428571429,
0.242857142857143,0.257142857142857,0.271428571428571,0.285714285714286,
0.3,0.314285714285714,0.328571428571429,0.342857142857143,0.357142857142857,
0.371428571428571,0.385714285714286,0.4,0.414285714285714,0.428571428571429,
0.442857142857143,0.457142857142857,0.471428571428572,0.485714285714286,
0.5,0.514285714285714,0.528571428571429,0.542857142857143,0.557142857142857,
0.571428571428571,0.585714285714286,0.6,0.614285714285714,0.628571428571428,
0.642857142857142,0.657142857142857,0.671428571428571,0.685714285714285,
0.699999999999999,0.714285714285714,0.728571428571428,0.742857142857142,
0.757142857142856,0.771428571428571,0.785714285714285,0.799999999999999,
0.814285714285713,0.828571428571428,0.842857142857142,0.857142857142856,
0.87142857142857,0.885714285714284,0.899999999999999,0.914285714285713,
0.928571428571427,0.942857142857141,0.957142857142856,0.97142857142857,
1.),.UNSPECIFIED.);
#562=B_SPLINE_CURVE_WITH_KNOTS('',5,(#30239,#30240,#30241,#30242,#30243,
#30244,#30245,#30246,#30247,#30248,#30249,#30250,#30251,#30252,#30253,#30254,
#30255,#30256,#30257,#30258,#30259,#30260,#30261,#30262,#30263,#30264,#30265,
#30266,#30267,#30268,#30269,#30270,#30271,#30272,#30273,#30274,#30275,#30276,
#30277,#30278,#30279,#30280,#30281,#30282,#30283,#30284,#30285,#30286,#30287,
#30288,#30289,#30290,#30291,#30292,#30293,#30294,#30295,#30296,#30297,#30298,
#30299,#30300,#30301,#30302,#30303,#30304,#30305,#30306,#30307,#30308,#30309,
#30310,#30311,#30312),.UNSPECIFIED.,.F.,.F.,(6,1,1,1,1,1,1,1,1,1,1,1,1,
1,1,1,1,1,1,1,1,1,1,1,1,1,1,1,1,1,1,1,1,1,1,1,1,1,1,1,1,1,1,1,1,1,1,1,1,
1,1,1,1,1,1,1,1,1,1,1,1,1,1,1,1,1,1,1,1,6),(0.,0.0142857142857143,0.0285714285714286,
0.0428571428571429,0.0571428571428571,0.0714285714285714,0.0857142857142857,
0.1,0.114285714285714,0.128571428571429,0.142857142857143,0.157142857142857,
0.171428571428571,0.185714285714286,0.2,0.214285714285714,0.228571428571429,
0.242857142857143,0.257142857142857,0.271428571428571,0.285714285714286,
0.3,0.314285714285714,0.328571428571429,0.342857142857143,0.357142857142857,
0.371428571428571,0.385714285714286,0.4,0.414285714285714,0.428571428571429,
0.442857142857143,0.457142857142857,0.471428571428572,0.485714285714286,
0.5,0.514285714285714,0.528571428571429,0.542857142857143,0.557142857142857,
0.571428571428571,0.585714285714286,0.6,0.614285714285714,0.628571428571428,
0.642857142857142,0.657142857142857,0.671428571428571,0.685714285714285,
0.699999999999999,0.714285714285714,0.728571428571428,0.742857142857142,
0.757142857142856,0.771428571428571,0.785714285714285,0.799999999999999,
0.814285714285713,0.828571428571428,0.842857142857142,0.857142857142856,
0.87142857142857,0.885714285714284,0.899999999999999,0.914285714285713,
0.928571428571427,0.942857142857141,0.957142857142856,0.97142857142857,
1.),.UNSPECIFIED.);
#563=B_SPLINE_CURVE_WITH_KNOTS('',5,(#30464,#30465,#30466,#30467,#30468,
#30469,#30470,#30471,#30472,#30473,#30474,#30475,#30476,#30477,#30478,#30479,
#30480,#30481,#30482,#30483,#30484,#30485,#30486,#30487,#30488,#30489,#30490,
#30491,#30492,#30493,#30494,#30495,#30496,#30497,#30498,#30499,#30500,#30501,
#30502,#30503,#30504,#30505,#30506,#30507,#30508,#30509,#30510,#30511,#30512,
#30513,#30514,#30515,#30516,#30517,#30518,#30519,#30520,#30521,#30522,#30523,
#30524,#30525,#30526,#30527,#30528,#30529,#30530,#30531,#30532,#30533,#30534,
#30535,#30536,#30537),.UNSPECIFIED.,.F.,.F.,(6,1,1,1,1,1,1,1,1,1,1,1,1,
1,1,1,1,1,1,1,1,1,1,1,1,1,1,1,1,1,1,1,1,1,1,1,1,1,1,1,1,1,1,1,1,1,1,1,1,
1,1,1,1,1,1,1,1,1,1,1,1,1,1,1,1,1,1,1,1,6),(0.,0.0142857142857143,0.0285714285714286,
0.0428571428571429,0.0571428571428571,0.0714285714285714,0.0857142857142857,
0.1,0.114285714285714,0.128571428571429,0.142857142857143,0.157142857142857,
0.171428571428571,0.185714285714286,0.2,0.214285714285714,0.228571428571429,
0.242857142857143,0.257142857142857,0.271428571428571,0.285714285714286,
0.3,0.314285714285714,0.328571428571429,0.342857142857143,0.357142857142857,
0.371428571428571,0.385714285714286,0.4,0.414285714285714,0.428571428571429,
0.442857142857143,0.457142857142857,0.471428571428572,0.485714285714286,
0.5,0.514285714285714,0.528571428571429,0.542857142857143,0.557142857142857,
0.571428571428571,0.585714285714286,0.6,0.614285714285714,0.628571428571428,
0.642857142857142,0.657142857142857,0.671428571428571,0.685714285714285,
0.699999999999999,0.714285714285714,0.728571428571428,0.742857142857142,
0.757142857142856,0.771428571428571,0.785714285714285,0.799999999999999,
0.814285714285713,0.828571428571428,0.842857142857142,0.857142857142856,
0.87142857142857,0.885714285714284,0.899999999999999,0.914285714285713,
0.928571428571427,0.942857142857141,0.957142857142856,0.97142857142857,
1.),.UNSPECIFIED.);
#564=B_SPLINE_CURVE_WITH_KNOTS('',5,(#30539,#30540,#30541,#30542,#30543,
#30544,#30545,#30546,#30547,#30548,#30549,#30550,#30551,#30552,#30553,#30554,
#30555,#30556,#30557,#30558,#30559,#30560,#30561,#30562,#30563,#30564,#30565,
#30566,#30567,#30568,#30569,#30570,#30571,#30572,#30573,#30574,#30575,#30576,
#30577,#30578,#30579,#30580,#30581,#30582,#30583,#30584,#30585,#30586,#30587,
#30588,#30589,#30590,#30591,#30592,#30593,#30594,#30595,#30596,#30597,#30598,
#30599,#30600,#30601,#30602,#30603,#30604,#30605,#30606,#30607,#30608,#30609,
#30610,#30611,#30612,#30613),.UNSPECIFIED.,.F.,.F.,(6,1,1,1,1,1,1,1,1,1,
1,1,1,1,1,1,1,1,1,1,1,1,1,1,1,1,1,1,1,1,1,1,1,1,1,1,1,1,1,1,1,1,1,1,1,1,
1,1,1,1,1,1,1,1,1,1,1,1,1,1,1,1,1,1,1,1,1,1,1,1,6),(-1.,-0.985714285714284,
-0.97142857142857,-0.957142857142856,-0.942857142857141,-0.928571428571427,
-0.914285714285713,-0.899999999999999,-0.885714285714284,-0.87142857142857,
-0.857142857142856,-0.842857142857142,-0.828571428571428,-0.814285714285713,
-0.799999999999999,-0.785714285714285,-0.771428571428571,-0.757142857142856,
-0.742857142857142,-0.728571428571428,-0.714285714285714,-0.699999999999999,
-0.685714285714285,-0.671428571428571,-0.657142857142857,-0.642857142857142,
-0.628571428571428,-0.614285714285714,-0.6,-0.585714285714286,-0.571428571428571,
-0.557142857142857,-0.542857142857143,-0.528571428571429,-0.514285714285714,
-0.5,-0.485714285714286,-0.471428571428572,-0.457142857142857,-0.442857142857143,
-0.428571428571429,-0.414285714285714,-0.4,-0.385714285714286,-0.371428571428571,
-0.357142857142857,-0.342857142857143,-0.328571428571429,-0.314285714285714,
-0.3,-0.285714285714286,-0.271428571428571,-0.257142857142857,-0.242857142857143,
-0.228571428571429,-0.214285714285714,-0.2,-0.185714285714286,-0.171428571428571,
-0.157142857142857,-0.142857142857143,-0.128571428571429,-0.114285714285714,
-0.1,-0.0857142857142857,-0.0714285714285714,-0.0571428571428571,-0.0428571428571429,
-0.0285714285714286,-0.0142857142857143,0.),.UNSPECIFIED.);
#565=B_SPLINE_CURVE_WITH_KNOTS('',5,(#30771,#30772,#30773,#30774,#30775,
#30776,#30777,#30778,#30779,#30780,#30781,#30782,#30783,#30784,#30785,#30786,
#30787,#30788,#30789,#30790,#30791,#30792,#30793,#30794,#30795,#30796,#30797,
#30798,#30799,#30800,#30801,#30802,#30803,#30804,#30805,#30806,#30807,#30808,
#30809,#30810,#30811,#30812,#30813,#30814,#30815,#30816,#30817,#30818,#30819,
#30820,#30821,#30822,#30823,#30824,#30825,#30826,#30827,#30828,#30829,#30830,
#30831,#30832,#30833,#30834,#30835,#30836,#30837,#30838,#30839,#30840,#30841,
#30842,#30843,#30844),.UNSPECIFIED.,.F.,.F.,(6,1,1,1,1,1,1,1,1,1,1,1,1,
1,1,1,1,1,1,1,1,1,1,1,1,1,1,1,1,1,1,1,1,1,1,1,1,1,1,1,1,1,1,1,1,1,1,1,1,
1,1,1,1,1,1,1,1,1,1,1,1,1,1,1,1,1,1,1,1,6),(0.,0.0142857142857143,0.0285714285714286,
0.0428571428571429,0.0571428571428571,0.0714285714285714,0.0857142857142857,
0.1,0.114285714285714,0.128571428571429,0.142857142857143,0.157142857142857,
0.171428571428571,0.185714285714286,0.2,0.214285714285714,0.228571428571429,
0.242857142857143,0.257142857142857,0.271428571428571,0.285714285714286,
0.3,0.314285714285714,0.328571428571429,0.342857142857143,0.357142857142857,
0.371428571428571,0.385714285714286,0.4,0.414285714285714,0.428571428571429,
0.442857142857143,0.457142857142857,0.471428571428572,0.485714285714286,
0.5,0.514285714285714,0.528571428571429,0.542857142857143,0.557142857142857,
0.571428571428571,0.585714285714286,0.6,0.614285714285714,0.628571428571428,
0.642857142857142,0.657142857142857,0.671428571428571,0.685714285714285,
0.699999999999999,0.714285714285714,0.728571428571428,0.742857142857142,
0.757142857142856,0.771428571428571,0.785714285714285,0.799999999999999,
0.814285714285713,0.828571428571428,0.842857142857142,0.857142857142856,
0.87142857142857,0.885714285714284,0.899999999999999,0.914285714285713,
0.928571428571427,0.942857142857141,0.957142857142856,0.97142857142857,
1.),.UNSPECIFIED.);
#566=B_SPLINE_CURVE_WITH_KNOTS('',5,(#30845,#30846,#30847,#30848,#30849,
#30850,#30851,#30852,#30853,#30854,#30855,#30856,#30857,#30858,#30859,#30860,
#30861,#30862,#30863,#30864,#30865,#30866,#30867,#30868,#30869,#30870,#30871,
#30872,#30873,#30874,#30875,#30876,#30877,#30878,#30879,#30880,#30881,#30882,
#30883,#30884,#30885,#30886,#30887,#30888,#30889,#30890,#30891,#30892,#30893,
#30894,#30895,#30896,#30897,#30898,#30899,#30900,#30901,#30902,#30903,#30904,
#30905,#30906,#30907,#30908,#30909,#30910,#30911,#30912,#30913,#30914,#30915,
#30916,#30917,#30918),.UNSPECIFIED.,.F.,.F.,(6,1,1,1,1,1,1,1,1,1,1,1,1,
1,1,1,1,1,1,1,1,1,1,1,1,1,1,1,1,1,1,1,1,1,1,1,1,1,1,1,1,1,1,1,1,1,1,1,1,
1,1,1,1,1,1,1,1,1,1,1,1,1,1,1,1,1,1,1,1,6),(0.,0.0142857142857143,0.0285714285714286,
0.0428571428571429,0.0571428571428571,0.0714285714285714,0.0857142857142857,
0.1,0.114285714285714,0.128571428571429,0.142857142857143,0.157142857142857,
0.171428571428571,0.185714285714286,0.2,0.214285714285714,0.228571428571429,
0.242857142857143,0.257142857142857,0.271428571428571,0.285714285714286,
0.3,0.314285714285714,0.328571428571429,0.342857142857143,0.357142857142857,
0.371428571428571,0.385714285714286,0.4,0.414285714285714,0.428571428571429,
0.442857142857143,0.457142857142857,0.471428571428572,0.485714285714286,
0.5,0.514285714285714,0.528571428571429,0.542857142857143,0.557142857142857,
0.571428571428571,0.585714285714286,0.6,0.614285714285714,0.628571428571428,
0.642857142857142,0.657142857142857,0.671428571428571,0.685714285714285,
0.699999999999999,0.714285714285714,0.728571428571428,0.742857142857142,
0.757142857142856,0.771428571428571,0.785714285714285,0.799999999999999,
0.814285714285713,0.828571428571428,0.842857142857142,0.857142857142856,
0.87142857142857,0.885714285714284,0.899999999999999,0.914285714285713,
0.928571428571427,0.942857142857141,0.957142857142856,0.97142857142857,
1.),.UNSPECIFIED.);
#567=B_SPLINE_CURVE_WITH_KNOTS('',5,(#30944,#30945,#30946,#30947,#30948,
#30949,#30950,#30951,#30952,#30953,#30954,#30955,#30956,#30957,#30958,#30959,
#30960,#30961,#30962,#30963,#30964,#30965,#30966,#30967,#30968,#30969,#30970,
#30971,#30972,#30973,#30974,#30975,#30976,#30977,#30978,#30979,#30980,#30981,
#30982,#30983,#30984,#30985,#30986,#30987,#30988,#30989,#30990,#30991,#30992,
#30993,#30994,#30995,#30996,#30997,#30998,#30999,#31000,#31001,#31002,#31003,
#31004,#31005,#31006,#31007,#31008,#31009,#31010,#31011,#31012,#31013,#31014,
#31015,#31016,#31017),.UNSPECIFIED.,.F.,.F.,(6,1,1,1,1,1,1,1,1,1,1,1,1,
1,1,1,1,1,1,1,1,1,1,1,1,1,1,1,1,1,1,1,1,1,1,1,1,1,1,1,1,1,1,1,1,1,1,1,1,
1,1,1,1,1,1,1,1,1,1,1,1,1,1,1,1,1,1,1,1,6),(0.,0.0142857142857143,0.0285714285714286,
0.0428571428571429,0.0571428571428571,0.0714285714285714,0.0857142857142857,
0.1,0.114285714285714,0.128571428571429,0.142857142857143,0.157142857142857,
0.171428571428571,0.185714285714286,0.2,0.214285714285714,0.228571428571429,
0.242857142857143,0.257142857142857,0.271428571428571,0.285714285714286,
0.3,0.314285714285714,0.328571428571429,0.342857142857143,0.357142857142857,
0.371428571428571,0.385714285714286,0.4,0.414285714285714,0.428571428571429,
0.442857142857143,0.457142857142857,0.471428571428572,0.485714285714286,
0.5,0.514285714285714,0.528571428571429,0.542857142857143,0.557142857142857,
0.571428571428571,0.585714285714286,0.6,0.614285714285714,0.628571428571428,
0.642857142857142,0.657142857142857,0.671428571428571,0.685714285714285,
0.699999999999999,0.714285714285714,0.728571428571428,0.742857142857142,
0.757142857142856,0.771428571428571,0.785714285714285,0.799999999999999,
0.814285714285713,0.828571428571428,0.842857142857142,0.857142857142856,
0.87142857142857,0.885714285714284,0.899999999999999,0.914285714285713,
0.928571428571427,0.942857142857141,0.957142857142856,0.97142857142857,
1.),.UNSPECIFIED.);
#568=B_SPLINE_CURVE_WITH_KNOTS('',5,(#31021,#31022,#31023,#31024,#31025,
#31026,#31027,#31028,#31029,#31030,#31031,#31032,#31033,#31034,#31035,#31036,
#31037,#31038,#31039,#31040,#31041,#31042,#31043,#31044,#31045,#31046,#31047,
#31048,#31049,#31050,#31051,#31052,#31053,#31054,#31055,#31056,#31057,#31058,
#31059,#31060,#31061,#31062,#31063,#31064,#31065,#31066,#31067,#31068,#31069,
#31070,#31071,#31072,#31073,#31074,#31075,#31076,#31077,#31078,#31079,#31080,
#31081,#31082,#31083,#31084,#31085,#31086,#31087,#31088,#31089,#31090,#31091,
#31092,#31093,#31094),.UNSPECIFIED.,.F.,.F.,(6,1,1,1,1,1,1,1,1,1,1,1,1,
1,1,1,1,1,1,1,1,1,1,1,1,1,1,1,1,1,1,1,1,1,1,1,1,1,1,1,1,1,1,1,1,1,1,1,1,
1,1,1,1,1,1,1,1,1,1,1,1,1,1,1,1,1,1,1,1,6),(0.,0.0142857142857143,0.0285714285714286,
0.0428571428571429,0.0571428571428571,0.0714285714285714,0.0857142857142857,
0.1,0.114285714285714,0.128571428571429,0.142857142857143,0.157142857142857,
0.171428571428571,0.185714285714286,0.2,0.214285714285714,0.228571428571429,
0.242857142857143,0.257142857142857,0.271428571428571,0.285714285714286,
0.3,0.314285714285714,0.328571428571429,0.342857142857143,0.357142857142857,
0.371428571428571,0.385714285714286,0.4,0.414285714285714,0.428571428571429,
0.442857142857143,0.457142857142857,0.471428571428572,0.485714285714286,
0.5,0.514285714285714,0.528571428571429,0.542857142857143,0.557142857142857,
0.571428571428571,0.585714285714286,0.6,0.614285714285714,0.628571428571428,
0.642857142857142,0.657142857142857,0.671428571428571,0.685714285714285,
0.699999999999999,0.714285714285714,0.728571428571428,0.742857142857142,
0.757142857142856,0.771428571428571,0.785714285714285,0.799999999999999,
0.814285714285713,0.828571428571428,0.842857142857142,0.857142857142856,
0.87142857142857,0.885714285714284,0.899999999999999,0.914285714285713,
0.928571428571427,0.942857142857141,0.957142857142856,0.97142857142857,
1.),.UNSPECIFIED.);
#569=B_SPLINE_CURVE_WITH_KNOTS('',5,(#31109,#31110,#31111,#31112,#31113,
#31114,#31115,#31116,#31117,#31118,#31119,#31120,#31121,#31122,#31123,#31124,
#31125,#31126,#31127,#31128,#31129,#31130,#31131,#31132,#31133,#31134,#31135,
#31136,#31137,#31138,#31139,#31140,#31141,#31142,#31143,#31144,#31145,#31146,
#31147,#31148,#31149,#31150,#31151,#31152,#31153,#31154,#31155,#31156,#31157,
#31158,#31159,#31160,#31161,#31162,#31163,#31164,#31165,#31166,#31167,#31168,
#31169,#31170,#31171,#31172,#31173,#31174,#31175,#31176,#31177,#31178,#31179,
#31180,#31181,#31182),.UNSPECIFIED.,.F.,.F.,(6,1,1,1,1,1,1,1,1,1,1,1,1,
1,1,1,1,1,1,1,1,1,1,1,1,1,1,1,1,1,1,1,1,1,1,1,1,1,1,1,1,1,1,1,1,1,1,1,1,
1,1,1,1,1,1,1,1,1,1,1,1,1,1,1,1,1,1,1,1,6),(0.,0.0142857142857143,0.0285714285714286,
0.0428571428571429,0.0571428571428571,0.0714285714285714,0.0857142857142857,
0.1,0.114285714285714,0.128571428571429,0.142857142857143,0.157142857142857,
0.171428571428571,0.185714285714286,0.2,0.214285714285714,0.228571428571429,
0.242857142857143,0.257142857142857,0.271428571428571,0.285714285714286,
0.3,0.314285714285714,0.328571428571429,0.342857142857143,0.357142857142857,
0.371428571428571,0.385714285714286,0.4,0.414285714285714,0.428571428571429,
0.442857142857143,0.457142857142857,0.471428571428572,0.485714285714286,
0.5,0.514285714285714,0.528571428571429,0.542857142857143,0.557142857142857,
0.571428571428571,0.585714285714286,0.6,0.614285714285714,0.628571428571428,
0.642857142857142,0.657142857142857,0.671428571428571,0.685714285714285,
0.699999999999999,0.714285714285714,0.728571428571428,0.742857142857142,
0.757142857142856,0.771428571428571,0.785714285714285,0.799999999999999,
0.814285714285713,0.828571428571428,0.842857142857142,0.857142857142856,
0.87142857142857,0.885714285714284,0.899999999999999,0.914285714285713,
0.928571428571427,0.942857142857141,0.957142857142856,0.97142857142857,
1.),.UNSPECIFIED.);
#570=B_SPLINE_CURVE_WITH_KNOTS('',5,(#31186,#31187,#31188,#31189,#31190,
#31191,#31192,#31193,#31194,#31195,#31196,#31197,#31198,#31199,#31200,#31201,
#31202,#31203,#31204,#31205,#31206,#31207,#31208,#31209,#31210,#31211,#31212,
#31213,#31214,#31215,#31216,#31217,#31218,#31219,#31220,#31221,#31222,#31223,
#31224,#31225,#31226,#31227,#31228,#31229,#31230,#31231,#31232,#31233,#31234,
#31235,#31236,#31237,#31238,#31239,#31240,#31241,#31242,#31243,#31244,#31245,
#31246,#31247,#31248,#31249,#31250,#31251,#31252,#31253,#31254,#31255,#31256,
#31257,#31258,#31259,#31260),.UNSPECIFIED.,.F.,.F.,(6,1,1,1,1,1,1,1,1,1,
1,1,1,1,1,1,1,1,1,1,1,1,1,1,1,1,1,1,1,1,1,1,1,1,1,1,1,1,1,1,1,1,1,1,1,1,
1,1,1,1,1,1,1,1,1,1,1,1,1,1,1,1,1,1,1,1,1,1,1,1,6),(-1.,-0.985714285714284,
-0.97142857142857,-0.957142857142856,-0.942857142857141,-0.928571428571427,
-0.914285714285713,-0.899999999999999,-0.885714285714284,-0.87142857142857,
-0.857142857142856,-0.842857142857142,-0.828571428571428,-0.814285714285713,
-0.799999999999999,-0.785714285714285,-0.771428571428571,-0.757142857142856,
-0.742857142857142,-0.728571428571428,-0.714285714285714,-0.699999999999999,
-0.685714285714285,-0.671428571428571,-0.657142857142857,-0.642857142857142,
-0.628571428571428,-0.614285714285714,-0.6,-0.585714285714286,-0.571428571428571,
-0.557142857142857,-0.542857142857143,-0.528571428571429,-0.514285714285714,
-0.5,-0.485714285714286,-0.471428571428572,-0.457142857142857,-0.442857142857143,
-0.428571428571429,-0.414285714285714,-0.4,-0.385714285714286,-0.371428571428571,
-0.357142857142857,-0.342857142857143,-0.328571428571429,-0.314285714285714,
-0.3,-0.285714285714286,-0.271428571428571,-0.257142857142857,-0.242857142857143,
-0.228571428571429,-0.214285714285714,-0.2,-0.185714285714286,-0.171428571428571,
-0.157142857142857,-0.142857142857143,-0.128571428571429,-0.114285714285714,
-0.1,-0.0857142857142857,-0.0714285714285714,-0.0571428571428571,-0.0428571428571429,
-0.0285714285714286,-0.0142857142857143,0.),.UNSPECIFIED.);
#571=B_SPLINE_CURVE_WITH_KNOTS('',5,(#32053,#32054,#32055,#32056,#32057,
#32058,#32059,#32060,#32061,#32062,#32063,#32064,#32065,#32066,#32067,#32068,
#32069,#32070,#32071,#32072,#32073,#32074,#32075,#32076,#32077,#32078,#32079,
#32080,#32081,#32082,#32083,#32084,#32085,#32086,#32087,#32088,#32089,#32090,
#32091,#32092,#32093,#32094,#32095,#32096,#32097,#32098,#32099,#32100,#32101,
#32102,#32103,#32104,#32105,#32106,#32107,#32108,#32109,#32110,#32111,#32112,
#32113,#32114,#32115,#32116,#32117,#32118,#32119,#32120,#32121,#32122,#32123,
#32124,#32125,#32126),.UNSPECIFIED.,.F.,.F.,(6,1,1,1,1,1,1,1,1,1,1,1,1,
1,1,1,1,1,1,1,1,1,1,1,1,1,1,1,1,1,1,1,1,1,1,1,1,1,1,1,1,1,1,1,1,1,1,1,1,
1,1,1,1,1,1,1,1,1,1,1,1,1,1,1,1,1,1,1,1,6),(0.,0.0142857142857143,0.0285714285714286,
0.0428571428571429,0.0571428571428571,0.0714285714285714,0.0857142857142857,
0.1,0.114285714285714,0.128571428571429,0.142857142857143,0.157142857142857,
0.171428571428571,0.185714285714286,0.2,0.214285714285714,0.228571428571429,
0.242857142857143,0.257142857142857,0.271428571428571,0.285714285714286,
0.3,0.314285714285714,0.328571428571429,0.342857142857143,0.357142857142857,
0.371428571428571,0.385714285714286,0.4,0.414285714285714,0.428571428571429,
0.442857142857143,0.457142857142857,0.471428571428572,0.485714285714286,
0.5,0.514285714285714,0.528571428571429,0.542857142857143,0.557142857142857,
0.571428571428571,0.585714285714286,0.6,0.614285714285714,0.628571428571428,
0.642857142857142,0.657142857142857,0.671428571428571,0.685714285714285,
0.699999999999999,0.714285714285714,0.728571428571428,0.742857142857142,
0.757142857142856,0.771428571428571,0.785714285714285,0.799999999999999,
0.814285714285713,0.828571428571428,0.842857142857142,0.857142857142856,
0.87142857142857,0.885714285714284,0.899999999999999,0.914285714285713,
0.928571428571427,0.942857142857141,0.957142857142856,0.97142857142857,
1.),.UNSPECIFIED.);
#572=B_SPLINE_CURVE_WITH_KNOTS('',5,(#32128,#32129,#32130,#32131,#32132,
#32133,#32134,#32135,#32136,#32137,#32138,#32139,#32140,#32141,#32142,#32143,
#32144,#32145,#32146,#32147,#32148,#32149,#32150,#32151,#32152,#32153,#32154,
#32155,#32156,#32157,#32158,#32159,#32160,#32161,#32162,#32163,#32164,#32165,
#32166,#32167,#32168,#32169,#32170,#32171,#32172,#32173,#32174,#32175,#32176,
#32177,#32178,#32179,#32180,#32181,#32182,#32183,#32184,#32185,#32186,#32187,
#32188,#32189,#32190,#32191,#32192,#32193,#32194,#32195,#32196,#32197,#32198,
#32199,#32200,#32201,#32202),.UNSPECIFIED.,.F.,.F.,(6,1,1,1,1,1,1,1,1,1,
1,1,1,1,1,1,1,1,1,1,1,1,1,1,1,1,1,1,1,1,1,1,1,1,1,1,1,1,1,1,1,1,1,1,1,1,
1,1,1,1,1,1,1,1,1,1,1,1,1,1,1,1,1,1,1,1,1,1,1,1,6),(-1.,-0.985714285714284,
-0.97142857142857,-0.957142857142856,-0.942857142857141,-0.928571428571427,
-0.914285714285713,-0.899999999999999,-0.885714285714284,-0.87142857142857,
-0.857142857142856,-0.842857142857142,-0.828571428571428,-0.814285714285713,
-0.799999999999999,-0.785714285714285,-0.771428571428571,-0.757142857142856,
-0.742857142857142,-0.728571428571428,-0.714285714285714,-0.699999999999999,
-0.685714285714285,-0.671428571428571,-0.657142857142857,-0.642857142857142,
-0.628571428571428,-0.614285714285714,-0.6,-0.585714285714286,-0.571428571428571,
-0.557142857142857,-0.542857142857143,-0.528571428571429,-0.514285714285714,
-0.5,-0.485714285714286,-0.471428571428572,-0.457142857142857,-0.442857142857143,
-0.428571428571429,-0.414285714285714,-0.4,-0.385714285714286,-0.371428571428571,
-0.357142857142857,-0.342857142857143,-0.328571428571429,-0.314285714285714,
-0.3,-0.285714285714286,-0.271428571428571,-0.257142857142857,-0.242857142857143,
-0.228571428571429,-0.214285714285714,-0.2,-0.185714285714286,-0.171428571428571,
-0.157142857142857,-0.142857142857143,-0.128571428571429,-0.114285714285714,
-0.1,-0.0857142857142857,-0.0714285714285714,-0.0571428571428571,-0.0428571428571429,
-0.0285714285714286,-0.0142857142857143,0.),.UNSPECIFIED.);
#573=B_SPLINE_CURVE_WITH_KNOTS('',5,(#32360,#32361,#32362,#32363,#32364,
#32365,#32366,#32367,#32368,#32369,#32370,#32371,#32372,#32373,#32374,#32375,
#32376,#32377,#32378,#32379,#32380,#32381,#32382,#32383,#32384,#32385,#32386,
#32387,#32388,#32389,#32390,#32391,#32392,#32393,#32394,#32395,#32396,#32397,
#32398,#32399,#32400,#32401,#32402,#32403,#32404,#32405,#32406,#32407,#32408,
#32409,#32410,#32411,#32412,#32413,#32414,#32415,#32416,#32417,#32418,#32419,
#32420,#32421,#32422,#32423,#32424,#32425,#32426,#32427,#32428,#32429,#32430,
#32431,#32432,#32433),.UNSPECIFIED.,.F.,.F.,(6,1,1,1,1,1,1,1,1,1,1,1,1,
1,1,1,1,1,1,1,1,1,1,1,1,1,1,1,1,1,1,1,1,1,1,1,1,1,1,1,1,1,1,1,1,1,1,1,1,
1,1,1,1,1,1,1,1,1,1,1,1,1,1,1,1,1,1,1,1,6),(0.,0.0142857142857143,0.0285714285714286,
0.0428571428571429,0.0571428571428571,0.0714285714285714,0.0857142857142857,
0.1,0.114285714285714,0.128571428571429,0.142857142857143,0.157142857142857,
0.171428571428571,0.185714285714286,0.2,0.214285714285714,0.228571428571429,
0.242857142857143,0.257142857142857,0.271428571428571,0.285714285714286,
0.3,0.314285714285714,0.328571428571429,0.342857142857143,0.357142857142857,
0.371428571428571,0.385714285714286,0.4,0.414285714285714,0.428571428571429,
0.442857142857143,0.457142857142857,0.471428571428572,0.485714285714286,
0.5,0.514285714285714,0.528571428571429,0.542857142857143,0.557142857142857,
0.571428571428571,0.585714285714286,0.6,0.614285714285714,0.628571428571428,
0.642857142857142,0.657142857142857,0.671428571428571,0.685714285714285,
0.699999999999999,0.714285714285714,0.728571428571428,0.742857142857142,
0.757142857142856,0.771428571428571,0.785714285714285,0.799999999999999,
0.814285714285713,0.828571428571428,0.842857142857142,0.857142857142856,
0.87142857142857,0.885714285714284,0.899999999999999,0.914285714285713,
0.928571428571427,0.942857142857141,0.957142857142856,0.97142857142857,
1.),.UNSPECIFIED.);
#574=B_SPLINE_CURVE_WITH_KNOTS('',5,(#32434,#32435,#32436,#32437,#32438,
#32439,#32440,#32441,#32442,#32443,#32444,#32445,#32446,#32447,#32448,#32449,
#32450,#32451,#32452,#32453,#32454,#32455,#32456,#32457,#32458,#32459,#32460,
#32461,#32462,#32463,#32464,#32465,#32466,#32467,#32468,#32469,#32470,#32471,
#32472,#32473,#32474,#32475,#32476,#32477,#32478,#32479,#32480,#32481,#32482,
#32483,#32484,#32485,#32486,#32487,#32488,#32489,#32490,#32491,#32492,#32493,
#32494,#32495,#32496,#32497,#32498,#32499,#32500,#32501,#32502,#32503,#32504,
#32505,#32506,#32507),.UNSPECIFIED.,.F.,.F.,(6,1,1,1,1,1,1,1,1,1,1,1,1,
1,1,1,1,1,1,1,1,1,1,1,1,1,1,1,1,1,1,1,1,1,1,1,1,1,1,1,1,1,1,1,1,1,1,1,1,
1,1,1,1,1,1,1,1,1,1,1,1,1,1,1,1,1,1,1,1,6),(0.,0.0142857142857143,0.0285714285714286,
0.0428571428571429,0.0571428571428571,0.0714285714285714,0.0857142857142857,
0.1,0.114285714285714,0.128571428571429,0.142857142857143,0.157142857142857,
0.171428571428571,0.185714285714286,0.2,0.214285714285714,0.228571428571429,
0.242857142857143,0.257142857142857,0.271428571428571,0.285714285714286,
0.3,0.314285714285714,0.328571428571429,0.342857142857143,0.357142857142857,
0.371428571428571,0.385714285714286,0.4,0.414285714285714,0.428571428571429,
0.442857142857143,0.457142857142857,0.471428571428572,0.485714285714286,
0.5,0.514285714285714,0.528571428571429,0.542857142857143,0.557142857142857,
0.571428571428571,0.585714285714286,0.6,0.614285714285714,0.628571428571428,
0.642857142857142,0.657142857142857,0.671428571428571,0.685714285714285,
0.699999999999999,0.714285714285714,0.728571428571428,0.742857142857142,
0.757142857142856,0.771428571428571,0.785714285714285,0.799999999999999,
0.814285714285713,0.828571428571428,0.842857142857142,0.857142857142856,
0.87142857142857,0.885714285714284,0.899999999999999,0.914285714285713,
0.928571428571427,0.942857142857141,0.957142857142856,0.97142857142857,
1.),.UNSPECIFIED.);
#575=B_SPLINE_CURVE_WITH_KNOTS('',5,(#32659,#32660,#32661,#32662,#32663,
#32664,#32665,#32666,#32667,#32668,#32669,#32670,#32671,#32672,#32673,#32674,
#32675,#32676,#32677,#32678,#32679,#32680,#32681,#32682,#32683,#32684,#32685,
#32686,#32687,#32688,#32689,#32690,#32691,#32692,#32693,#32694,#32695,#32696,
#32697,#32698,#32699,#32700,#32701,#32702,#32703,#32704,#32705,#32706,#32707,
#32708,#32709,#32710,#32711,#32712,#32713,#32714,#32715,#32716,#32717,#32718,
#32719,#32720,#32721,#32722,#32723,#32724,#32725,#32726,#32727,#32728,#32729,
#32730,#32731,#32732),.UNSPECIFIED.,.F.,.F.,(6,1,1,1,1,1,1,1,1,1,1,1,1,
1,1,1,1,1,1,1,1,1,1,1,1,1,1,1,1,1,1,1,1,1,1,1,1,1,1,1,1,1,1,1,1,1,1,1,1,
1,1,1,1,1,1,1,1,1,1,1,1,1,1,1,1,1,1,1,1,6),(0.,0.0142857142857143,0.0285714285714286,
0.0428571428571429,0.0571428571428571,0.0714285714285714,0.0857142857142857,
0.1,0.114285714285714,0.128571428571429,0.142857142857143,0.157142857142857,
0.171428571428571,0.185714285714286,0.2,0.214285714285714,0.228571428571429,
0.242857142857143,0.257142857142857,0.271428571428571,0.285714285714286,
0.3,0.314285714285714,0.328571428571429,0.342857142857143,0.357142857142857,
0.371428571428571,0.385714285714286,0.4,0.414285714285714,0.428571428571429,
0.442857142857143,0.457142857142857,0.471428571428572,0.485714285714286,
0.5,0.514285714285714,0.528571428571429,0.542857142857143,0.557142857142857,
0.571428571428571,0.585714285714286,0.6,0.614285714285714,0.628571428571428,
0.642857142857142,0.657142857142857,0.671428571428571,0.685714285714285,
0.699999999999999,0.714285714285714,0.728571428571428,0.742857142857142,
0.757142857142856,0.771428571428571,0.785714285714285,0.799999999999999,
0.814285714285713,0.828571428571428,0.842857142857142,0.857142857142856,
0.87142857142857,0.885714285714284,0.899999999999999,0.914285714285713,
0.928571428571427,0.942857142857141,0.957142857142856,0.97142857142857,
1.),.UNSPECIFIED.);
#576=B_SPLINE_CURVE_WITH_KNOTS('',5,(#32734,#32735,#32736,#32737,#32738,
#32739,#32740,#32741,#32742,#32743,#32744,#32745,#32746,#32747,#32748,#32749,
#32750,#32751,#32752,#32753,#32754,#32755,#32756,#32757,#32758,#32759,#32760,
#32761,#32762,#32763,#32764,#32765,#32766,#32767,#32768,#32769,#32770,#32771,
#32772,#32773,#32774,#32775,#32776,#32777,#32778,#32779,#32780,#32781,#32782,
#32783,#32784,#32785,#32786,#32787,#32788,#32789,#32790,#32791,#32792,#32793,
#32794,#32795,#32796,#32797,#32798,#32799,#32800,#32801,#32802,#32803,#32804,
#32805,#32806,#32807,#32808),.UNSPECIFIED.,.F.,.F.,(6,1,1,1,1,1,1,1,1,1,
1,1,1,1,1,1,1,1,1,1,1,1,1,1,1,1,1,1,1,1,1,1,1,1,1,1,1,1,1,1,1,1,1,1,1,1,
1,1,1,1,1,1,1,1,1,1,1,1,1,1,1,1,1,1,1,1,1,1,1,1,6),(-1.,-0.985714285714284,
-0.97142857142857,-0.957142857142856,-0.942857142857141,-0.928571428571427,
-0.914285714285713,-0.899999999999999,-0.885714285714284,-0.87142857142857,
-0.857142857142856,-0.842857142857142,-0.828571428571428,-0.814285714285713,
-0.799999999999999,-0.785714285714285,-0.771428571428571,-0.757142857142856,
-0.742857142857142,-0.728571428571428,-0.714285714285714,-0.699999999999999,
-0.685714285714285,-0.671428571428571,-0.657142857142857,-0.642857142857142,
-0.628571428571428,-0.614285714285714,-0.6,-0.585714285714286,-0.571428571428571,
-0.557142857142857,-0.542857142857143,-0.528571428571429,-0.514285714285714,
-0.5,-0.485714285714286,-0.471428571428572,-0.457142857142857,-0.442857142857143,
-0.428571428571429,-0.414285714285714,-0.4,-0.385714285714286,-0.371428571428571,
-0.357142857142857,-0.342857142857143,-0.328571428571429,-0.314285714285714,
-0.3,-0.285714285714286,-0.271428571428571,-0.257142857142857,-0.242857142857143,
-0.228571428571429,-0.214285714285714,-0.2,-0.185714285714286,-0.171428571428571,
-0.157142857142857,-0.142857142857143,-0.128571428571429,-0.114285714285714,
-0.1,-0.0857142857142857,-0.0714285714285714,-0.0571428571428571,-0.0428571428571429,
-0.0285714285714286,-0.0142857142857143,0.),.UNSPECIFIED.);
#577=B_SPLINE_CURVE_WITH_KNOTS('',5,(#32966,#32967,#32968,#32969,#32970,
#32971,#32972,#32973,#32974,#32975,#32976,#32977,#32978,#32979,#32980,#32981,
#32982,#32983,#32984,#32985,#32986,#32987,#32988,#32989,#32990,#32991,#32992,
#32993,#32994,#32995,#32996,#32997,#32998,#32999,#33000,#33001,#33002,#33003,
#33004,#33005,#33006,#33007,#33008,#33009,#33010,#33011,#33012,#33013,#33014,
#33015,#33016,#33017,#33018,#33019,#33020,#33021,#33022,#33023,#33024,#33025,
#33026,#33027,#33028,#33029,#33030,#33031,#33032,#33033,#33034,#33035,#33036,
#33037,#33038,#33039),.UNSPECIFIED.,.F.,.F.,(6,1,1,1,1,1,1,1,1,1,1,1,1,
1,1,1,1,1,1,1,1,1,1,1,1,1,1,1,1,1,1,1,1,1,1,1,1,1,1,1,1,1,1,1,1,1,1,1,1,
1,1,1,1,1,1,1,1,1,1,1,1,1,1,1,1,1,1,1,1,6),(0.,0.0142857142857143,0.0285714285714286,
0.0428571428571429,0.0571428571428571,0.0714285714285714,0.0857142857142857,
0.1,0.114285714285714,0.128571428571429,0.142857142857143,0.157142857142857,
0.171428571428571,0.185714285714286,0.2,0.214285714285714,0.228571428571429,
0.242857142857143,0.257142857142857,0.271428571428571,0.285714285714286,
0.3,0.314285714285714,0.328571428571429,0.342857142857143,0.357142857142857,
0.371428571428571,0.385714285714286,0.4,0.414285714285714,0.428571428571429,
0.442857142857143,0.457142857142857,0.471428571428572,0.485714285714286,
0.5,0.514285714285714,0.528571428571429,0.542857142857143,0.557142857142857,
0.571428571428571,0.585714285714286,0.6,0.614285714285714,0.628571428571428,
0.642857142857142,0.657142857142857,0.671428571428571,0.685714285714285,
0.699999999999999,0.714285714285714,0.728571428571428,0.742857142857142,
0.757142857142856,0.771428571428571,0.785714285714285,0.799999999999999,
0.814285714285713,0.828571428571428,0.842857142857142,0.857142857142856,
0.87142857142857,0.885714285714284,0.899999999999999,0.914285714285713,
0.928571428571427,0.942857142857141,0.957142857142856,0.97142857142857,
1.),.UNSPECIFIED.);
#578=B_SPLINE_CURVE_WITH_KNOTS('',5,(#33040,#33041,#33042,#33043,#33044,
#33045,#33046,#33047,#33048,#33049,#33050,#33051,#33052,#33053,#33054,#33055,
#33056,#33057,#33058,#33059,#33060,#33061,#33062,#33063,#33064,#33065,#33066,
#33067,#33068,#33069,#33070,#33071,#33072,#33073,#33074,#33075,#33076,#33077,
#33078,#33079,#33080,#33081,#33082,#33083,#33084,#33085,#33086,#33087,#33088,
#33089,#33090,#33091,#33092,#33093,#33094,#33095,#33096,#33097,#33098,#33099,
#33100,#33101,#33102,#33103,#33104,#33105,#33106,#33107,#33108,#33109,#33110,
#33111,#33112,#33113),.UNSPECIFIED.,.F.,.F.,(6,1,1,1,1,1,1,1,1,1,1,1,1,
1,1,1,1,1,1,1,1,1,1,1,1,1,1,1,1,1,1,1,1,1,1,1,1,1,1,1,1,1,1,1,1,1,1,1,1,
1,1,1,1,1,1,1,1,1,1,1,1,1,1,1,1,1,1,1,1,6),(0.,0.0142857142857143,0.0285714285714286,
0.0428571428571429,0.0571428571428571,0.0714285714285714,0.0857142857142857,
0.1,0.114285714285714,0.128571428571429,0.142857142857143,0.157142857142857,
0.171428571428571,0.185714285714286,0.2,0.214285714285714,0.228571428571429,
0.242857142857143,0.257142857142857,0.271428571428571,0.285714285714286,
0.3,0.314285714285714,0.328571428571429,0.342857142857143,0.357142857142857,
0.371428571428571,0.385714285714286,0.4,0.414285714285714,0.428571428571429,
0.442857142857143,0.457142857142857,0.471428571428572,0.485714285714286,
0.5,0.514285714285714,0.528571428571429,0.542857142857143,0.557142857142857,
0.571428571428571,0.585714285714286,0.6,0.614285714285714,0.628571428571428,
0.642857142857142,0.657142857142857,0.671428571428571,0.685714285714285,
0.699999999999999,0.714285714285714,0.728571428571428,0.742857142857142,
0.757142857142856,0.771428571428571,0.785714285714285,0.799999999999999,
0.814285714285713,0.828571428571428,0.842857142857142,0.857142857142856,
0.87142857142857,0.885714285714284,0.899999999999999,0.914285714285713,
0.928571428571427,0.942857142857141,0.957142857142856,0.97142857142857,
1.),.UNSPECIFIED.);
#579=B_SPLINE_CURVE_WITH_KNOTS('',5,(#33265,#33266,#33267,#33268,#33269,
#33270,#33271,#33272,#33273,#33274,#33275,#33276,#33277,#33278,#33279,#33280,
#33281,#33282,#33283,#33284,#33285,#33286,#33287,#33288,#33289,#33290,#33291,
#33292,#33293,#33294,#33295,#33296,#33297,#33298,#33299,#33300,#33301,#33302,
#33303,#33304,#33305,#33306,#33307,#33308,#33309,#33310,#33311,#33312,#33313,
#33314,#33315,#33316,#33317,#33318,#33319,#33320,#33321,#33322,#33323,#33324,
#33325,#33326,#33327,#33328,#33329,#33330,#33331,#33332,#33333,#33334,#33335,
#33336,#33337,#33338),.UNSPECIFIED.,.F.,.F.,(6,1,1,1,1,1,1,1,1,1,1,1,1,
1,1,1,1,1,1,1,1,1,1,1,1,1,1,1,1,1,1,1,1,1,1,1,1,1,1,1,1,1,1,1,1,1,1,1,1,
1,1,1,1,1,1,1,1,1,1,1,1,1,1,1,1,1,1,1,1,6),(0.,0.0142857142857143,0.0285714285714286,
0.0428571428571429,0.0571428571428571,0.0714285714285714,0.0857142857142857,
0.1,0.114285714285714,0.128571428571429,0.142857142857143,0.157142857142857,
0.171428571428571,0.185714285714286,0.2,0.214285714285714,0.228571428571429,
0.242857142857143,0.257142857142857,0.271428571428571,0.285714285714286,
0.3,0.314285714285714,0.328571428571429,0.342857142857143,0.357142857142857,
0.371428571428571,0.385714285714286,0.4,0.414285714285714,0.428571428571429,
0.442857142857143,0.457142857142857,0.471428571428572,0.485714285714286,
0.5,0.514285714285714,0.528571428571429,0.542857142857143,0.557142857142857,
0.571428571428571,0.585714285714286,0.6,0.614285714285714,0.628571428571428,
0.642857142857142,0.657142857142857,0.671428571428571,0.685714285714285,
0.699999999999999,0.714285714285714,0.728571428571428,0.742857142857142,
0.757142857142856,0.771428571428571,0.785714285714285,0.799999999999999,
0.814285714285713,0.828571428571428,0.842857142857142,0.857142857142856,
0.87142857142857,0.885714285714284,0.899999999999999,0.914285714285713,
0.928571428571427,0.942857142857141,0.957142857142856,0.97142857142857,
1.),.UNSPECIFIED.);
#580=B_SPLINE_CURVE_WITH_KNOTS('',5,(#33340,#33341,#33342,#33343,#33344,
#33345,#33346,#33347,#33348,#33349,#33350,#33351,#33352,#33353,#33354,#33355,
#33356,#33357,#33358,#33359,#33360,#33361,#33362,#33363,#33364,#33365,#33366,
#33367,#33368,#33369,#33370,#33371,#33372,#33373,#33374,#33375,#33376,#33377,
#33378,#33379,#33380,#33381,#33382,#33383,#33384,#33385,#33386,#33387,#33388,
#33389,#33390,#33391,#33392,#33393,#33394,#33395,#33396,#33397,#33398,#33399,
#33400,#33401,#33402,#33403,#33404,#33405,#33406,#33407,#33408,#33409,#33410,
#33411,#33412,#33413,#33414),.UNSPECIFIED.,.F.,.F.,(6,1,1,1,1,1,1,1,1,1,
1,1,1,1,1,1,1,1,1,1,1,1,1,1,1,1,1,1,1,1,1,1,1,1,1,1,1,1,1,1,1,1,1,1,1,1,
1,1,1,1,1,1,1,1,1,1,1,1,1,1,1,1,1,1,1,1,1,1,1,1,6),(-1.,-0.985714285714284,
-0.97142857142857,-0.957142857142856,-0.942857142857141,-0.928571428571427,
-0.914285714285713,-0.899999999999999,-0.885714285714284,-0.87142857142857,
-0.857142857142856,-0.842857142857142,-0.828571428571428,-0.814285714285713,
-0.799999999999999,-0.785714285714285,-0.771428571428571,-0.757142857142856,
-0.742857142857142,-0.728571428571428,-0.714285714285714,-0.699999999999999,
-0.685714285714285,-0.671428571428571,-0.657142857142857,-0.642857142857142,
-0.628571428571428,-0.614285714285714,-0.6,-0.585714285714286,-0.571428571428571,
-0.557142857142857,-0.542857142857143,-0.528571428571429,-0.514285714285714,
-0.5,-0.485714285714286,-0.471428571428572,-0.457142857142857,-0.442857142857143,
-0.428571428571429,-0.414285714285714,-0.4,-0.385714285714286,-0.371428571428571,
-0.357142857142857,-0.342857142857143,-0.328571428571429,-0.314285714285714,
-0.3,-0.285714285714286,-0.271428571428571,-0.257142857142857,-0.242857142857143,
-0.228571428571429,-0.214285714285714,-0.2,-0.185714285714286,-0.171428571428571,
-0.157142857142857,-0.142857142857143,-0.128571428571429,-0.114285714285714,
-0.1,-0.0857142857142857,-0.0714285714285714,-0.0571428571428571,-0.0428571428571429,
-0.0285714285714286,-0.0142857142857143,0.),.UNSPECIFIED.);
#581=B_SPLINE_CURVE_WITH_KNOTS('',5,(#33572,#33573,#33574,#33575,#33576,
#33577,#33578,#33579,#33580,#33581,#33582,#33583,#33584,#33585,#33586,#33587,
#33588,#33589,#33590,#33591,#33592,#33593,#33594,#33595,#33596,#33597,#33598,
#33599,#33600,#33601,#33602,#33603,#33604,#33605,#33606,#33607,#33608,#33609,
#33610,#33611,#33612,#33613,#33614,#33615,#33616,#33617,#33618,#33619,#33620,
#33621,#33622,#33623,#33624,#33625,#33626,#33627,#33628,#33629,#33630,#33631,
#33632,#33633,#33634,#33635,#33636,#33637,#33638,#33639,#33640,#33641,#33642,
#33643,#33644,#33645),.UNSPECIFIED.,.F.,.F.,(6,1,1,1,1,1,1,1,1,1,1,1,1,
1,1,1,1,1,1,1,1,1,1,1,1,1,1,1,1,1,1,1,1,1,1,1,1,1,1,1,1,1,1,1,1,1,1,1,1,
1,1,1,1,1,1,1,1,1,1,1,1,1,1,1,1,1,1,1,1,6),(0.,0.0142857142857143,0.0285714285714286,
0.0428571428571429,0.0571428571428571,0.0714285714285714,0.0857142857142857,
0.1,0.114285714285714,0.128571428571429,0.142857142857143,0.157142857142857,
0.171428571428571,0.185714285714286,0.2,0.214285714285714,0.228571428571429,
0.242857142857143,0.257142857142857,0.271428571428571,0.285714285714286,
0.3,0.314285714285714,0.328571428571429,0.342857142857143,0.357142857142857,
0.371428571428571,0.385714285714286,0.4,0.414285714285714,0.428571428571429,
0.442857142857143,0.457142857142857,0.471428571428572,0.485714285714286,
0.5,0.514285714285714,0.528571428571429,0.542857142857143,0.557142857142857,
0.571428571428571,0.585714285714286,0.6,0.614285714285714,0.628571428571428,
0.642857142857142,0.657142857142857,0.671428571428571,0.685714285714285,
0.699999999999999,0.714285714285714,0.728571428571428,0.742857142857142,
0.757142857142856,0.771428571428571,0.785714285714285,0.799999999999999,
0.814285714285713,0.828571428571428,0.842857142857142,0.857142857142856,
0.87142857142857,0.885714285714284,0.899999999999999,0.914285714285713,
0.928571428571427,0.942857142857141,0.957142857142856,0.97142857142857,
1.),.UNSPECIFIED.);
#582=B_SPLINE_CURVE_WITH_KNOTS('',5,(#33646,#33647,#33648,#33649,#33650,
#33651,#33652,#33653,#33654,#33655,#33656,#33657,#33658,#33659,#33660,#33661,
#33662,#33663,#33664,#33665,#33666,#33667,#33668,#33669,#33670,#33671,#33672,
#33673,#33674,#33675,#33676,#33677,#33678,#33679,#33680,#33681,#33682,#33683,
#33684,#33685,#33686,#33687,#33688,#33689,#33690,#33691,#33692,#33693,#33694,
#33695,#33696,#33697,#33698,#33699,#33700,#33701,#33702,#33703,#33704,#33705,
#33706,#33707,#33708,#33709,#33710,#33711,#33712,#33713,#33714,#33715,#33716,
#33717,#33718,#33719),.UNSPECIFIED.,.F.,.F.,(6,1,1,1,1,1,1,1,1,1,1,1,1,
1,1,1,1,1,1,1,1,1,1,1,1,1,1,1,1,1,1,1,1,1,1,1,1,1,1,1,1,1,1,1,1,1,1,1,1,
1,1,1,1,1,1,1,1,1,1,1,1,1,1,1,1,1,1,1,1,6),(0.,0.0142857142857143,0.0285714285714286,
0.0428571428571429,0.0571428571428571,0.0714285714285714,0.0857142857142857,
0.1,0.114285714285714,0.128571428571429,0.142857142857143,0.157142857142857,
0.171428571428571,0.185714285714286,0.2,0.214285714285714,0.228571428571429,
0.242857142857143,0.257142857142857,0.271428571428571,0.285714285714286,
0.3,0.314285714285714,0.328571428571429,0.342857142857143,0.357142857142857,
0.371428571428571,0.385714285714286,0.4,0.414285714285714,0.428571428571429,
0.442857142857143,0.457142857142857,0.471428571428572,0.485714285714286,
0.5,0.514285714285714,0.528571428571429,0.542857142857143,0.557142857142857,
0.571428571428571,0.585714285714286,0.6,0.614285714285714,0.628571428571428,
0.642857142857142,0.657142857142857,0.671428571428571,0.685714285714285,
0.699999999999999,0.714285714285714,0.728571428571428,0.742857142857142,
0.757142857142856,0.771428571428571,0.785714285714285,0.799999999999999,
0.814285714285713,0.828571428571428,0.842857142857142,0.857142857142856,
0.87142857142857,0.885714285714284,0.899999999999999,0.914285714285713,
0.928571428571427,0.942857142857141,0.957142857142856,0.97142857142857,
1.),.UNSPECIFIED.);
#583=B_SPLINE_CURVE_WITH_KNOTS('',5,(#33871,#33872,#33873,#33874,#33875,
#33876,#33877,#33878,#33879,#33880,#33881,#33882,#33883,#33884,#33885,#33886,
#33887,#33888,#33889,#33890,#33891,#33892,#33893,#33894,#33895,#33896,#33897,
#33898,#33899,#33900,#33901,#33902,#33903,#33904,#33905,#33906,#33907,#33908,
#33909,#33910,#33911,#33912,#33913,#33914,#33915,#33916,#33917,#33918,#33919,
#33920,#33921,#33922,#33923,#33924,#33925,#33926,#33927,#33928,#33929,#33930,
#33931,#33932,#33933,#33934,#33935,#33936,#33937,#33938,#33939,#33940,#33941,
#33942,#33943,#33944),.UNSPECIFIED.,.F.,.F.,(6,1,1,1,1,1,1,1,1,1,1,1,1,
1,1,1,1,1,1,1,1,1,1,1,1,1,1,1,1,1,1,1,1,1,1,1,1,1,1,1,1,1,1,1,1,1,1,1,1,
1,1,1,1,1,1,1,1,1,1,1,1,1,1,1,1,1,1,1,1,6),(0.,0.0142857142857143,0.0285714285714286,
0.0428571428571429,0.0571428571428571,0.0714285714285714,0.0857142857142857,
0.1,0.114285714285714,0.128571428571429,0.142857142857143,0.157142857142857,
0.171428571428571,0.185714285714286,0.2,0.214285714285714,0.228571428571429,
0.242857142857143,0.257142857142857,0.271428571428571,0.285714285714286,
0.3,0.314285714285714,0.328571428571429,0.342857142857143,0.357142857142857,
0.371428571428571,0.385714285714286,0.4,0.414285714285714,0.428571428571429,
0.442857142857143,0.457142857142857,0.471428571428572,0.485714285714286,
0.5,0.514285714285714,0.528571428571429,0.542857142857143,0.557142857142857,
0.571428571428571,0.585714285714286,0.6,0.614285714285714,0.628571428571428,
0.642857142857142,0.657142857142857,0.671428571428571,0.685714285714285,
0.699999999999999,0.714285714285714,0.728571428571428,0.742857142857142,
0.757142857142856,0.771428571428571,0.785714285714285,0.799999999999999,
0.814285714285713,0.828571428571428,0.842857142857142,0.857142857142856,
0.87142857142857,0.885714285714284,0.899999999999999,0.914285714285713,
0.928571428571427,0.942857142857141,0.957142857142856,0.97142857142857,
1.),.UNSPECIFIED.);
#584=B_SPLINE_CURVE_WITH_KNOTS('',5,(#33946,#33947,#33948,#33949,#33950,
#33951,#33952,#33953,#33954,#33955,#33956,#33957,#33958,#33959,#33960,#33961,
#33962,#33963,#33964,#33965,#33966,#33967,#33968,#33969,#33970,#33971,#33972,
#33973,#33974,#33975,#33976,#33977,#33978,#33979,#33980,#33981,#33982,#33983,
#33984,#33985,#33986,#33987,#33988,#33989,#33990,#33991,#33992,#33993,#33994,
#33995,#33996,#33997,#33998,#33999,#34000,#34001,#34002,#34003,#34004,#34005,
#34006,#34007,#34008,#34009,#34010,#34011,#34012,#34013,#34014,#34015,#34016,
#34017,#34018,#34019,#34020),.UNSPECIFIED.,.F.,.F.,(6,1,1,1,1,1,1,1,1,1,
1,1,1,1,1,1,1,1,1,1,1,1,1,1,1,1,1,1,1,1,1,1,1,1,1,1,1,1,1,1,1,1,1,1,1,1,
1,1,1,1,1,1,1,1,1,1,1,1,1,1,1,1,1,1,1,1,1,1,1,1,6),(-1.,-0.985714285714284,
-0.97142857142857,-0.957142857142856,-0.942857142857141,-0.928571428571427,
-0.914285714285713,-0.899999999999999,-0.885714285714284,-0.87142857142857,
-0.857142857142856,-0.842857142857142,-0.828571428571428,-0.814285714285713,
-0.799999999999999,-0.785714285714285,-0.771428571428571,-0.757142857142856,
-0.742857142857142,-0.728571428571428,-0.714285714285714,-0.699999999999999,
-0.685714285714285,-0.671428571428571,-0.657142857142857,-0.642857142857142,
-0.628571428571428,-0.614285714285714,-0.6,-0.585714285714286,-0.571428571428571,
-0.557142857142857,-0.542857142857143,-0.528571428571429,-0.514285714285714,
-0.5,-0.485714285714286,-0.471428571428572,-0.457142857142857,-0.442857142857143,
-0.428571428571429,-0.414285714285714,-0.4,-0.385714285714286,-0.371428571428571,
-0.357142857142857,-0.342857142857143,-0.328571428571429,-0.314285714285714,
-0.3,-0.285714285714286,-0.271428571428571,-0.257142857142857,-0.242857142857143,
-0.228571428571429,-0.214285714285714,-0.2,-0.185714285714286,-0.171428571428571,
-0.157142857142857,-0.142857142857143,-0.128571428571429,-0.114285714285714,
-0.1,-0.0857142857142857,-0.0714285714285714,-0.0571428571428571,-0.0428571428571429,
-0.0285714285714286,-0.0142857142857143,0.),.UNSPECIFIED.);
#585=B_SPLINE_CURVE_WITH_KNOTS('',5,(#34178,#34179,#34180,#34181,#34182,
#34183,#34184,#34185,#34186,#34187,#34188,#34189,#34190,#34191,#34192,#34193,
#34194,#34195,#34196,#34197,#34198,#34199,#34200,#34201,#34202,#34203,#34204,
#34205,#34206,#34207,#34208,#34209,#34210,#34211,#34212,#34213,#34214,#34215,
#34216,#34217,#34218,#34219,#34220,#34221,#34222,#34223,#34224,#34225,#34226,
#34227,#34228,#34229,#34230,#34231,#34232,#34233,#34234,#34235,#34236,#34237,
#34238,#34239,#34240,#34241,#34242,#34243,#34244,#34245,#34246,#34247,#34248,
#34249,#34250,#34251),.UNSPECIFIED.,.F.,.F.,(6,1,1,1,1,1,1,1,1,1,1,1,1,
1,1,1,1,1,1,1,1,1,1,1,1,1,1,1,1,1,1,1,1,1,1,1,1,1,1,1,1,1,1,1,1,1,1,1,1,
1,1,1,1,1,1,1,1,1,1,1,1,1,1,1,1,1,1,1,1,6),(0.,0.0142857142857143,0.0285714285714286,
0.0428571428571429,0.0571428571428571,0.0714285714285714,0.0857142857142857,
0.1,0.114285714285714,0.128571428571429,0.142857142857143,0.157142857142857,
0.171428571428571,0.185714285714286,0.2,0.214285714285714,0.228571428571429,
0.242857142857143,0.257142857142857,0.271428571428571,0.285714285714286,
0.3,0.314285714285714,0.328571428571429,0.342857142857143,0.357142857142857,
0.371428571428571,0.385714285714286,0.4,0.414285714285714,0.428571428571429,
0.442857142857143,0.457142857142857,0.471428571428572,0.485714285714286,
0.5,0.514285714285714,0.528571428571429,0.542857142857143,0.557142857142857,
0.571428571428571,0.585714285714286,0.6,0.614285714285714,0.628571428571428,
0.642857142857142,0.657142857142857,0.671428571428571,0.685714285714285,
0.699999999999999,0.714285714285714,0.728571428571428,0.742857142857142,
0.757142857142856,0.771428571428571,0.785714285714285,0.799999999999999,
0.814285714285713,0.828571428571428,0.842857142857142,0.857142857142856,
0.87142857142857,0.885714285714284,0.899999999999999,0.914285714285713,
0.928571428571427,0.942857142857141,0.957142857142856,0.97142857142857,
1.),.UNSPECIFIED.);
#586=B_SPLINE_CURVE_WITH_KNOTS('',5,(#34252,#34253,#34254,#34255,#34256,
#34257,#34258,#34259,#34260,#34261,#34262,#34263,#34264,#34265,#34266,#34267,
#34268,#34269,#34270,#34271,#34272,#34273,#34274,#34275,#34276,#34277,#34278,
#34279,#34280,#34281,#34282,#34283,#34284,#34285,#34286,#34287,#34288,#34289,
#34290,#34291,#34292,#34293,#34294,#34295,#34296,#34297,#34298,#34299,#34300,
#34301,#34302,#34303,#34304,#34305,#34306,#34307,#34308,#34309,#34310,#34311,
#34312,#34313,#34314,#34315,#34316,#34317,#34318,#34319,#34320,#34321,#34322,
#34323,#34324,#34325),.UNSPECIFIED.,.F.,.F.,(6,1,1,1,1,1,1,1,1,1,1,1,1,
1,1,1,1,1,1,1,1,1,1,1,1,1,1,1,1,1,1,1,1,1,1,1,1,1,1,1,1,1,1,1,1,1,1,1,1,
1,1,1,1,1,1,1,1,1,1,1,1,1,1,1,1,1,1,1,1,6),(0.,0.0142857142857143,0.0285714285714286,
0.0428571428571429,0.0571428571428571,0.0714285714285714,0.0857142857142857,
0.1,0.114285714285714,0.128571428571429,0.142857142857143,0.157142857142857,
0.171428571428571,0.185714285714286,0.2,0.214285714285714,0.228571428571429,
0.242857142857143,0.257142857142857,0.271428571428571,0.285714285714286,
0.3,0.314285714285714,0.328571428571429,0.342857142857143,0.357142857142857,
0.371428571428571,0.385714285714286,0.4,0.414285714285714,0.428571428571429,
0.442857142857143,0.457142857142857,0.471428571428572,0.485714285714286,
0.5,0.514285714285714,0.528571428571429,0.542857142857143,0.557142857142857,
0.571428571428571,0.585714285714286,0.6,0.614285714285714,0.628571428571428,
0.642857142857142,0.657142857142857,0.671428571428571,0.685714285714285,
0.699999999999999,0.714285714285714,0.728571428571428,0.742857142857142,
0.757142857142856,0.771428571428571,0.785714285714285,0.799999999999999,
0.814285714285713,0.828571428571428,0.842857142857142,0.857142857142856,
0.87142857142857,0.885714285714284,0.899999999999999,0.914285714285713,
0.928571428571427,0.942857142857141,0.957142857142856,0.97142857142857,
1.),.UNSPECIFIED.);
#587=B_SPLINE_CURVE_WITH_KNOTS('',5,(#34477,#34478,#34479,#34480,#34481,
#34482,#34483,#34484,#34485,#34486,#34487,#34488,#34489,#34490,#34491,#34492,
#34493,#34494,#34495,#34496,#34497,#34498,#34499,#34500,#34501,#34502,#34503,
#34504,#34505,#34506,#34507,#34508,#34509,#34510,#34511,#34512,#34513,#34514,
#34515,#34516,#34517,#34518,#34519,#34520,#34521,#34522,#34523,#34524,#34525,
#34526,#34527,#34528,#34529,#34530,#34531,#34532,#34533,#34534,#34535,#34536,
#34537,#34538,#34539,#34540,#34541,#34542,#34543,#34544,#34545,#34546,#34547,
#34548,#34549,#34550),.UNSPECIFIED.,.F.,.F.,(6,1,1,1,1,1,1,1,1,1,1,1,1,
1,1,1,1,1,1,1,1,1,1,1,1,1,1,1,1,1,1,1,1,1,1,1,1,1,1,1,1,1,1,1,1,1,1,1,1,
1,1,1,1,1,1,1,1,1,1,1,1,1,1,1,1,1,1,1,1,6),(0.,0.0142857142857143,0.0285714285714286,
0.0428571428571429,0.0571428571428571,0.0714285714285714,0.0857142857142857,
0.1,0.114285714285714,0.128571428571429,0.142857142857143,0.157142857142857,
0.171428571428571,0.185714285714286,0.2,0.214285714285714,0.228571428571429,
0.242857142857143,0.257142857142857,0.271428571428571,0.285714285714286,
0.3,0.314285714285714,0.328571428571429,0.342857142857143,0.357142857142857,
0.371428571428571,0.385714285714286,0.4,0.414285714285714,0.428571428571429,
0.442857142857143,0.457142857142857,0.471428571428572,0.485714285714286,
0.5,0.514285714285714,0.528571428571429,0.542857142857143,0.557142857142857,
0.571428571428571,0.585714285714286,0.6,0.614285714285714,0.628571428571428,
0.642857142857142,0.657142857142857,0.671428571428571,0.685714285714285,
0.699999999999999,0.714285714285714,0.728571428571428,0.742857142857142,
0.757142857142856,0.771428571428571,0.785714285714285,0.799999999999999,
0.814285714285713,0.828571428571428,0.842857142857142,0.857142857142856,
0.87142857142857,0.885714285714284,0.899999999999999,0.914285714285713,
0.928571428571427,0.942857142857141,0.957142857142856,0.97142857142857,
1.),.UNSPECIFIED.);
#588=B_SPLINE_CURVE_WITH_KNOTS('',5,(#34552,#34553,#34554,#34555,#34556,
#34557,#34558,#34559,#34560,#34561,#34562,#34563,#34564,#34565,#34566,#34567,
#34568,#34569,#34570,#34571,#34572,#34573,#34574,#34575,#34576,#34577,#34578,
#34579,#34580,#34581,#34582,#34583,#34584,#34585,#34586,#34587,#34588,#34589,
#34590,#34591,#34592,#34593,#34594,#34595,#34596,#34597,#34598,#34599,#34600,
#34601,#34602,#34603,#34604,#34605,#34606,#34607,#34608,#34609,#34610,#34611,
#34612,#34613,#34614,#34615,#34616,#34617,#34618,#34619,#34620,#34621,#34622,
#34623,#34624,#34625,#34626),.UNSPECIFIED.,.F.,.F.,(6,1,1,1,1,1,1,1,1,1,
1,1,1,1,1,1,1,1,1,1,1,1,1,1,1,1,1,1,1,1,1,1,1,1,1,1,1,1,1,1,1,1,1,1,1,1,
1,1,1,1,1,1,1,1,1,1,1,1,1,1,1,1,1,1,1,1,1,1,1,1,6),(-1.,-0.985714285714284,
-0.97142857142857,-0.957142857142856,-0.942857142857141,-0.928571428571427,
-0.914285714285713,-0.899999999999999,-0.885714285714284,-0.87142857142857,
-0.857142857142856,-0.842857142857142,-0.828571428571428,-0.814285714285713,
-0.799999999999999,-0.785714285714285,-0.771428571428571,-0.757142857142856,
-0.742857142857142,-0.728571428571428,-0.714285714285714,-0.699999999999999,
-0.685714285714285,-0.671428571428571,-0.657142857142857,-0.642857142857142,
-0.628571428571428,-0.614285714285714,-0.6,-0.585714285714286,-0.571428571428571,
-0.557142857142857,-0.542857142857143,-0.528571428571429,-0.514285714285714,
-0.5,-0.485714285714286,-0.471428571428572,-0.457142857142857,-0.442857142857143,
-0.428571428571429,-0.414285714285714,-0.4,-0.385714285714286,-0.371428571428571,
-0.357142857142857,-0.342857142857143,-0.328571428571429,-0.314285714285714,
-0.3,-0.285714285714286,-0.271428571428571,-0.257142857142857,-0.242857142857143,
-0.228571428571429,-0.214285714285714,-0.2,-0.185714285714286,-0.171428571428571,
-0.157142857142857,-0.142857142857143,-0.128571428571429,-0.114285714285714,
-0.1,-0.0857142857142857,-0.0714285714285714,-0.0571428571428571,-0.0428571428571429,
-0.0285714285714286,-0.0142857142857143,0.),.UNSPECIFIED.);
#589=B_SPLINE_CURVE_WITH_KNOTS('',5,(#34784,#34785,#34786,#34787,#34788,
#34789,#34790,#34791,#34792,#34793,#34794,#34795,#34796,#34797,#34798,#34799,
#34800,#34801,#34802,#34803,#34804,#34805,#34806,#34807,#34808,#34809,#34810,
#34811,#34812,#34813,#34814,#34815,#34816,#34817,#34818,#34819,#34820,#34821,
#34822,#34823,#34824,#34825,#34826,#34827,#34828,#34829,#34830,#34831,#34832,
#34833,#34834,#34835,#34836,#34837,#34838,#34839,#34840,#34841,#34842,#34843,
#34844,#34845,#34846,#34847,#34848,#34849,#34850,#34851,#34852,#34853,#34854,
#34855,#34856,#34857),.UNSPECIFIED.,.F.,.F.,(6,1,1,1,1,1,1,1,1,1,1,1,1,
1,1,1,1,1,1,1,1,1,1,1,1,1,1,1,1,1,1,1,1,1,1,1,1,1,1,1,1,1,1,1,1,1,1,1,1,
1,1,1,1,1,1,1,1,1,1,1,1,1,1,1,1,1,1,1,1,6),(0.,0.0142857142857143,0.0285714285714286,
0.0428571428571429,0.0571428571428571,0.0714285714285714,0.0857142857142857,
0.1,0.114285714285714,0.128571428571429,0.142857142857143,0.157142857142857,
0.171428571428571,0.185714285714286,0.2,0.214285714285714,0.228571428571429,
0.242857142857143,0.257142857142857,0.271428571428571,0.285714285714286,
0.3,0.314285714285714,0.328571428571429,0.342857142857143,0.357142857142857,
0.371428571428571,0.385714285714286,0.4,0.414285714285714,0.428571428571429,
0.442857142857143,0.457142857142857,0.471428571428572,0.485714285714286,
0.5,0.514285714285714,0.528571428571429,0.542857142857143,0.557142857142857,
0.571428571428571,0.585714285714286,0.6,0.614285714285714,0.628571428571428,
0.642857142857142,0.657142857142857,0.671428571428571,0.685714285714285,
0.699999999999999,0.714285714285714,0.728571428571428,0.742857142857142,
0.757142857142856,0.771428571428571,0.785714285714285,0.799999999999999,
0.814285714285713,0.828571428571428,0.842857142857142,0.857142857142856,
0.87142857142857,0.885714285714284,0.899999999999999,0.914285714285713,
0.928571428571427,0.942857142857141,0.957142857142856,0.97142857142857,
1.),.UNSPECIFIED.);
#590=B_SPLINE_CURVE_WITH_KNOTS('',5,(#34858,#34859,#34860,#34861,#34862,
#34863,#34864,#34865,#34866,#34867,#34868,#34869,#34870,#34871,#34872,#34873,
#34874,#34875,#34876,#34877,#34878,#34879,#34880,#34881,#34882,#34883,#34884,
#34885,#34886,#34887,#34888,#34889,#34890,#34891,#34892,#34893,#34894,#34895,
#34896,#34897,#34898,#34899,#34900,#34901,#34902,#34903,#34904,#34905,#34906,
#34907,#34908,#34909,#34910,#34911,#34912,#34913,#34914,#34915,#34916,#34917,
#34918,#34919,#34920,#34921,#34922,#34923,#34924,#34925,#34926,#34927,#34928,
#34929,#34930,#34931),.UNSPECIFIED.,.F.,.F.,(6,1,1,1,1,1,1,1,1,1,1,1,1,
1,1,1,1,1,1,1,1,1,1,1,1,1,1,1,1,1,1,1,1,1,1,1,1,1,1,1,1,1,1,1,1,1,1,1,1,
1,1,1,1,1,1,1,1,1,1,1,1,1,1,1,1,1,1,1,1,6),(0.,0.0142857142857143,0.0285714285714286,
0.0428571428571429,0.0571428571428571,0.0714285714285714,0.0857142857142857,
0.1,0.114285714285714,0.128571428571429,0.142857142857143,0.157142857142857,
0.171428571428571,0.185714285714286,0.2,0.214285714285714,0.228571428571429,
0.242857142857143,0.257142857142857,0.271428571428571,0.285714285714286,
0.3,0.314285714285714,0.328571428571429,0.342857142857143,0.357142857142857,
0.371428571428571,0.385714285714286,0.4,0.414285714285714,0.428571428571429,
0.442857142857143,0.457142857142857,0.471428571428572,0.485714285714286,
0.5,0.514285714285714,0.528571428571429,0.542857142857143,0.557142857142857,
0.571428571428571,0.585714285714286,0.6,0.614285714285714,0.628571428571428,
0.642857142857142,0.657142857142857,0.671428571428571,0.685714285714285,
0.699999999999999,0.714285714285714,0.728571428571428,0.742857142857142,
0.757142857142856,0.771428571428571,0.785714285714285,0.799999999999999,
0.814285714285713,0.828571428571428,0.842857142857142,0.857142857142856,
0.87142857142857,0.885714285714284,0.899999999999999,0.914285714285713,
0.928571428571427,0.942857142857141,0.957142857142856,0.97142857142857,
1.),.UNSPECIFIED.);
#591=B_SPLINE_CURVE_WITH_KNOTS('',5,(#35083,#35084,#35085,#35086,#35087,
#35088,#35089,#35090,#35091,#35092,#35093,#35094,#35095,#35096,#35097,#35098,
#35099,#35100,#35101,#35102,#35103,#35104,#35105,#35106,#35107,#35108,#35109,
#35110,#35111,#35112,#35113,#35114,#35115,#35116,#35117,#35118,#35119,#35120,
#35121,#35122,#35123,#35124,#35125,#35126,#35127,#35128,#35129,#35130,#35131,
#35132,#35133,#35134,#35135,#35136,#35137,#35138,#35139,#35140,#35141,#35142,
#35143,#35144,#35145,#35146,#35147,#35148,#35149,#35150,#35151,#35152,#35153,
#35154,#35155,#35156),.UNSPECIFIED.,.F.,.F.,(6,1,1,1,1,1,1,1,1,1,1,1,1,
1,1,1,1,1,1,1,1,1,1,1,1,1,1,1,1,1,1,1,1,1,1,1,1,1,1,1,1,1,1,1,1,1,1,1,1,
1,1,1,1,1,1,1,1,1,1,1,1,1,1,1,1,1,1,1,1,6),(0.,0.0142857142857143,0.0285714285714286,
0.0428571428571429,0.0571428571428571,0.0714285714285714,0.0857142857142857,
0.1,0.114285714285714,0.128571428571429,0.142857142857143,0.157142857142857,
0.171428571428571,0.185714285714286,0.2,0.214285714285714,0.228571428571429,
0.242857142857143,0.257142857142857,0.271428571428571,0.285714285714286,
0.3,0.314285714285714,0.328571428571429,0.342857142857143,0.357142857142857,
0.371428571428571,0.385714285714286,0.4,0.414285714285714,0.428571428571429,
0.442857142857143,0.457142857142857,0.471428571428572,0.485714285714286,
0.5,0.514285714285714,0.528571428571429,0.542857142857143,0.557142857142857,
0.571428571428571,0.585714285714286,0.6,0.614285714285714,0.628571428571428,
0.642857142857142,0.657142857142857,0.671428571428571,0.685714285714285,
0.699999999999999,0.714285714285714,0.728571428571428,0.742857142857142,
0.757142857142856,0.771428571428571,0.785714285714285,0.799999999999999,
0.814285714285713,0.828571428571428,0.842857142857142,0.857142857142856,
0.87142857142857,0.885714285714284,0.899999999999999,0.914285714285713,
0.928571428571427,0.942857142857141,0.957142857142856,0.97142857142857,
1.),.UNSPECIFIED.);
#592=B_SPLINE_CURVE_WITH_KNOTS('',5,(#35158,#35159,#35160,#35161,#35162,
#35163,#35164,#35165,#35166,#35167,#35168,#35169,#35170,#35171,#35172,#35173,
#35174,#35175,#35176,#35177,#35178,#35179,#35180,#35181,#35182,#35183,#35184,
#35185,#35186,#35187,#35188,#35189,#35190,#35191,#35192,#35193,#35194,#35195,
#35196,#35197,#35198,#35199,#35200,#35201,#35202,#35203,#35204,#35205,#35206,
#35207,#35208,#35209,#35210,#35211,#35212,#35213,#35214,#35215,#35216,#35217,
#35218,#35219,#35220,#35221,#35222,#35223,#35224,#35225,#35226,#35227,#35228,
#35229,#35230,#35231,#35232),.UNSPECIFIED.,.F.,.F.,(6,1,1,1,1,1,1,1,1,1,
1,1,1,1,1,1,1,1,1,1,1,1,1,1,1,1,1,1,1,1,1,1,1,1,1,1,1,1,1,1,1,1,1,1,1,1,
1,1,1,1,1,1,1,1,1,1,1,1,1,1,1,1,1,1,1,1,1,1,1,1,6),(-1.,-0.985714285714284,
-0.97142857142857,-0.957142857142856,-0.942857142857141,-0.928571428571427,
-0.914285714285713,-0.899999999999999,-0.885714285714284,-0.87142857142857,
-0.857142857142856,-0.842857142857142,-0.828571428571428,-0.814285714285713,
-0.799999999999999,-0.785714285714285,-0.771428571428571,-0.757142857142856,
-0.742857142857142,-0.728571428571428,-0.714285714285714,-0.699999999999999,
-0.685714285714285,-0.671428571428571,-0.657142857142857,-0.642857142857142,
-0.628571428571428,-0.614285714285714,-0.6,-0.585714285714286,-0.571428571428571,
-0.557142857142857,-0.542857142857143,-0.528571428571429,-0.514285714285714,
-0.5,-0.485714285714286,-0.471428571428572,-0.457142857142857,-0.442857142857143,
-0.428571428571429,-0.414285714285714,-0.4,-0.385714285714286,-0.371428571428571,
-0.357142857142857,-0.342857142857143,-0.328571428571429,-0.314285714285714,
-0.3,-0.285714285714286,-0.271428571428571,-0.257142857142857,-0.242857142857143,
-0.228571428571429,-0.214285714285714,-0.2,-0.185714285714286,-0.171428571428571,
-0.157142857142857,-0.142857142857143,-0.128571428571429,-0.114285714285714,
-0.1,-0.0857142857142857,-0.0714285714285714,-0.0571428571428571,-0.0428571428571429,
-0.0285714285714286,-0.0142857142857143,0.),.UNSPECIFIED.);
#593=B_SPLINE_CURVE_WITH_KNOTS('',5,(#35390,#35391,#35392,#35393,#35394,
#35395,#35396,#35397,#35398,#35399,#35400,#35401,#35402,#35403,#35404,#35405,
#35406,#35407,#35408,#35409,#35410,#35411,#35412,#35413,#35414,#35415,#35416,
#35417,#35418,#35419,#35420,#35421,#35422,#35423,#35424,#35425,#35426,#35427,
#35428,#35429,#35430,#35431,#35432,#35433,#35434,#35435,#35436,#35437,#35438,
#35439,#35440,#35441,#35442,#35443,#35444,#35445,#35446,#35447,#35448,#35449,
#35450,#35451,#35452,#35453,#35454,#35455,#35456,#35457,#35458,#35459,#35460,
#35461,#35462,#35463),.UNSPECIFIED.,.F.,.F.,(6,1,1,1,1,1,1,1,1,1,1,1,1,
1,1,1,1,1,1,1,1,1,1,1,1,1,1,1,1,1,1,1,1,1,1,1,1,1,1,1,1,1,1,1,1,1,1,1,1,
1,1,1,1,1,1,1,1,1,1,1,1,1,1,1,1,1,1,1,1,6),(0.,0.0142857142857143,0.0285714285714286,
0.0428571428571429,0.0571428571428571,0.0714285714285714,0.0857142857142857,
0.1,0.114285714285714,0.128571428571429,0.142857142857143,0.157142857142857,
0.171428571428571,0.185714285714286,0.2,0.214285714285714,0.228571428571429,
0.242857142857143,0.257142857142857,0.271428571428571,0.285714285714286,
0.3,0.314285714285714,0.328571428571429,0.342857142857143,0.357142857142857,
0.371428571428571,0.385714285714286,0.4,0.414285714285714,0.428571428571429,
0.442857142857143,0.457142857142857,0.471428571428572,0.485714285714286,
0.5,0.514285714285714,0.528571428571429,0.542857142857143,0.557142857142857,
0.571428571428571,0.585714285714286,0.6,0.614285714285714,0.628571428571428,
0.642857142857142,0.657142857142857,0.671428571428571,0.685714285714285,
0.699999999999999,0.714285714285714,0.728571428571428,0.742857142857142,
0.757142857142856,0.771428571428571,0.785714285714285,0.799999999999999,
0.814285714285713,0.828571428571428,0.842857142857142,0.857142857142856,
0.87142857142857,0.885714285714284,0.899999999999999,0.914285714285713,
0.928571428571427,0.942857142857141,0.957142857142856,0.97142857142857,
1.),.UNSPECIFIED.);
#594=B_SPLINE_CURVE_WITH_KNOTS('',5,(#35464,#35465,#35466,#35467,#35468,
#35469,#35470,#35471,#35472,#35473,#35474,#35475,#35476,#35477,#35478,#35479,
#35480,#35481,#35482,#35483,#35484,#35485,#35486,#35487,#35488,#35489,#35490,
#35491,#35492,#35493,#35494,#35495,#35496,#35497,#35498,#35499,#35500,#35501,
#35502,#35503,#35504,#35505,#35506,#35507,#35508,#35509,#35510,#35511,#35512,
#35513,#35514,#35515,#35516,#35517,#35518,#35519,#35520,#35521,#35522,#35523,
#35524,#35525,#35526,#35527,#35528,#35529,#35530,#35531,#35532,#35533,#35534,
#35535,#35536,#35537),.UNSPECIFIED.,.F.,.F.,(6,1,1,1,1,1,1,1,1,1,1,1,1,
1,1,1,1,1,1,1,1,1,1,1,1,1,1,1,1,1,1,1,1,1,1,1,1,1,1,1,1,1,1,1,1,1,1,1,1,
1,1,1,1,1,1,1,1,1,1,1,1,1,1,1,1,1,1,1,1,6),(0.,0.0142857142857143,0.0285714285714286,
0.0428571428571429,0.0571428571428571,0.0714285714285714,0.0857142857142857,
0.1,0.114285714285714,0.128571428571429,0.142857142857143,0.157142857142857,
0.171428571428571,0.185714285714286,0.2,0.214285714285714,0.228571428571429,
0.242857142857143,0.257142857142857,0.271428571428571,0.285714285714286,
0.3,0.314285714285714,0.328571428571429,0.342857142857143,0.357142857142857,
0.371428571428571,0.385714285714286,0.4,0.414285714285714,0.428571428571429,
0.442857142857143,0.457142857142857,0.471428571428572,0.485714285714286,
0.5,0.514285714285714,0.528571428571429,0.542857142857143,0.557142857142857,
0.571428571428571,0.585714285714286,0.6,0.614285714285714,0.628571428571428,
0.642857142857142,0.657142857142857,0.671428571428571,0.685714285714285,
0.699999999999999,0.714285714285714,0.728571428571428,0.742857142857142,
0.757142857142856,0.771428571428571,0.785714285714285,0.799999999999999,
0.814285714285713,0.828571428571428,0.842857142857142,0.857142857142856,
0.87142857142857,0.885714285714284,0.899999999999999,0.914285714285713,
0.928571428571427,0.942857142857141,0.957142857142856,0.97142857142857,
1.),.UNSPECIFIED.);
#595=B_SPLINE_CURVE_WITH_KNOTS('',5,(#35689,#35690,#35691,#35692,#35693,
#35694,#35695,#35696,#35697,#35698,#35699,#35700,#35701,#35702,#35703,#35704,
#35705,#35706,#35707,#35708,#35709,#35710,#35711,#35712,#35713,#35714,#35715,
#35716,#35717,#35718,#35719,#35720,#35721,#35722,#35723,#35724,#35725,#35726,
#35727,#35728,#35729,#35730,#35731,#35732,#35733,#35734,#35735,#35736,#35737,
#35738,#35739,#35740,#35741,#35742,#35743,#35744,#35745,#35746,#35747,#35748,
#35749,#35750,#35751,#35752,#35753,#35754,#35755,#35756,#35757,#35758,#35759,
#35760,#35761,#35762),.UNSPECIFIED.,.F.,.F.,(6,1,1,1,1,1,1,1,1,1,1,1,1,
1,1,1,1,1,1,1,1,1,1,1,1,1,1,1,1,1,1,1,1,1,1,1,1,1,1,1,1,1,1,1,1,1,1,1,1,
1,1,1,1,1,1,1,1,1,1,1,1,1,1,1,1,1,1,1,1,6),(0.,0.0142857142857143,0.0285714285714286,
0.0428571428571429,0.0571428571428571,0.0714285714285714,0.0857142857142857,
0.1,0.114285714285714,0.128571428571429,0.142857142857143,0.157142857142857,
0.171428571428571,0.185714285714286,0.2,0.214285714285714,0.228571428571429,
0.242857142857143,0.257142857142857,0.271428571428571,0.285714285714286,
0.3,0.314285714285714,0.328571428571429,0.342857142857143,0.357142857142857,
0.371428571428571,0.385714285714286,0.4,0.414285714285714,0.428571428571429,
0.442857142857143,0.457142857142857,0.471428571428572,0.485714285714286,
0.5,0.514285714285714,0.528571428571429,0.542857142857143,0.557142857142857,
0.571428571428571,0.585714285714286,0.6,0.614285714285714,0.628571428571428,
0.642857142857142,0.657142857142857,0.671428571428571,0.685714285714285,
0.699999999999999,0.714285714285714,0.728571428571428,0.742857142857142,
0.757142857142856,0.771428571428571,0.785714285714285,0.799999999999999,
0.814285714285713,0.828571428571428,0.842857142857142,0.857142857142856,
0.87142857142857,0.885714285714284,0.899999999999999,0.914285714285713,
0.928571428571427,0.942857142857141,0.957142857142856,0.97142857142857,
1.),.UNSPECIFIED.);
#596=B_SPLINE_CURVE_WITH_KNOTS('',5,(#35764,#35765,#35766,#35767,#35768,
#35769,#35770,#35771,#35772,#35773,#35774,#35775,#35776,#35777,#35778,#35779,
#35780,#35781,#35782,#35783,#35784,#35785,#35786,#35787,#35788,#35789,#35790,
#35791,#35792,#35793,#35794,#35795,#35796,#35797,#35798,#35799,#35800,#35801,
#35802,#35803,#35804,#35805,#35806,#35807,#35808,#35809,#35810,#35811,#35812,
#35813,#35814,#35815,#35816,#35817,#35818,#35819,#35820,#35821,#35822,#35823,
#35824,#35825,#35826,#35827,#35828,#35829,#35830,#35831,#35832,#35833,#35834,
#35835,#35836,#35837,#35838),.UNSPECIFIED.,.F.,.F.,(6,1,1,1,1,1,1,1,1,1,
1,1,1,1,1,1,1,1,1,1,1,1,1,1,1,1,1,1,1,1,1,1,1,1,1,1,1,1,1,1,1,1,1,1,1,1,
1,1,1,1,1,1,1,1,1,1,1,1,1,1,1,1,1,1,1,1,1,1,1,1,6),(-1.,-0.985714285714284,
-0.97142857142857,-0.957142857142856,-0.942857142857141,-0.928571428571427,
-0.914285714285713,-0.899999999999999,-0.885714285714284,-0.87142857142857,
-0.857142857142856,-0.842857142857142,-0.828571428571428,-0.814285714285713,
-0.799999999999999,-0.785714285714285,-0.771428571428571,-0.757142857142856,
-0.742857142857142,-0.728571428571428,-0.714285714285714,-0.699999999999999,
-0.685714285714285,-0.671428571428571,-0.657142857142857,-0.642857142857142,
-0.628571428571428,-0.614285714285714,-0.6,-0.585714285714286,-0.571428571428571,
-0.557142857142857,-0.542857142857143,-0.528571428571429,-0.514285714285714,
-0.5,-0.485714285714286,-0.471428571428572,-0.457142857142857,-0.442857142857143,
-0.428571428571429,-0.414285714285714,-0.4,-0.385714285714286,-0.371428571428571,
-0.357142857142857,-0.342857142857143,-0.328571428571429,-0.314285714285714,
-0.3,-0.285714285714286,-0.271428571428571,-0.257142857142857,-0.242857142857143,
-0.228571428571429,-0.214285714285714,-0.2,-0.185714285714286,-0.171428571428571,
-0.157142857142857,-0.142857142857143,-0.128571428571429,-0.114285714285714,
-0.1,-0.0857142857142857,-0.0714285714285714,-0.0571428571428571,-0.0428571428571429,
-0.0285714285714286,-0.0142857142857143,0.),.UNSPECIFIED.);
#597=B_SPLINE_CURVE_WITH_KNOTS('',5,(#35996,#35997,#35998,#35999,#36000,
#36001,#36002,#36003,#36004,#36005,#36006,#36007,#36008,#36009,#36010,#36011,
#36012,#36013,#36014,#36015,#36016,#36017,#36018,#36019,#36020,#36021,#36022,
#36023,#36024,#36025,#36026,#36027,#36028,#36029,#36030,#36031,#36032,#36033,
#36034,#36035,#36036,#36037,#36038,#36039,#36040,#36041,#36042,#36043,#36044,
#36045,#36046,#36047,#36048,#36049,#36050,#36051,#36052,#36053,#36054,#36055,
#36056,#36057,#36058,#36059,#36060,#36061,#36062,#36063,#36064,#36065,#36066,
#36067,#36068,#36069),.UNSPECIFIED.,.F.,.F.,(6,1,1,1,1,1,1,1,1,1,1,1,1,
1,1,1,1,1,1,1,1,1,1,1,1,1,1,1,1,1,1,1,1,1,1,1,1,1,1,1,1,1,1,1,1,1,1,1,1,
1,1,1,1,1,1,1,1,1,1,1,1,1,1,1,1,1,1,1,1,6),(0.,0.0142857142857143,0.0285714285714286,
0.0428571428571429,0.0571428571428571,0.0714285714285714,0.0857142857142857,
0.1,0.114285714285714,0.128571428571429,0.142857142857143,0.157142857142857,
0.171428571428571,0.185714285714286,0.2,0.214285714285714,0.228571428571429,
0.242857142857143,0.257142857142857,0.271428571428571,0.285714285714286,
0.3,0.314285714285714,0.328571428571429,0.342857142857143,0.357142857142857,
0.371428571428571,0.385714285714286,0.4,0.414285714285714,0.428571428571429,
0.442857142857143,0.457142857142857,0.471428571428572,0.485714285714286,
0.5,0.514285714285714,0.528571428571429,0.542857142857143,0.557142857142857,
0.571428571428571,0.585714285714286,0.6,0.614285714285714,0.628571428571428,
0.642857142857142,0.657142857142857,0.671428571428571,0.685714285714285,
0.699999999999999,0.714285714285714,0.728571428571428,0.742857142857142,
0.757142857142856,0.771428571428571,0.785714285714285,0.799999999999999,
0.814285714285713,0.828571428571428,0.842857142857142,0.857142857142856,
0.87142857142857,0.885714285714284,0.899999999999999,0.914285714285713,
0.928571428571427,0.942857142857141,0.957142857142856,0.97142857142857,
1.),.UNSPECIFIED.);
#598=B_SPLINE_CURVE_WITH_KNOTS('',5,(#36070,#36071,#36072,#36073,#36074,
#36075,#36076,#36077,#36078,#36079,#36080,#36081,#36082,#36083,#36084,#36085,
#36086,#36087,#36088,#36089,#36090,#36091,#36092,#36093,#36094,#36095,#36096,
#36097,#36098,#36099,#36100,#36101,#36102,#36103,#36104,#36105,#36106,#36107,
#36108,#36109,#36110,#36111,#36112,#36113,#36114,#36115,#36116,#36117,#36118,
#36119,#36120,#36121,#36122,#36123,#36124,#36125,#36126,#36127,#36128,#36129,
#36130,#36131,#36132,#36133,#36134,#36135,#36136,#36137,#36138,#36139,#36140,
#36141,#36142,#36143),.UNSPECIFIED.,.F.,.F.,(6,1,1,1,1,1,1,1,1,1,1,1,1,
1,1,1,1,1,1,1,1,1,1,1,1,1,1,1,1,1,1,1,1,1,1,1,1,1,1,1,1,1,1,1,1,1,1,1,1,
1,1,1,1,1,1,1,1,1,1,1,1,1,1,1,1,1,1,1,1,6),(0.,0.0142857142857143,0.0285714285714286,
0.0428571428571429,0.0571428571428571,0.0714285714285714,0.0857142857142857,
0.1,0.114285714285714,0.128571428571429,0.142857142857143,0.157142857142857,
0.171428571428571,0.185714285714286,0.2,0.214285714285714,0.228571428571429,
0.242857142857143,0.257142857142857,0.271428571428571,0.285714285714286,
0.3,0.314285714285714,0.328571428571429,0.342857142857143,0.357142857142857,
0.371428571428571,0.385714285714286,0.4,0.414285714285714,0.428571428571429,
0.442857142857143,0.457142857142857,0.471428571428572,0.485714285714286,
0.5,0.514285714285714,0.528571428571429,0.542857142857143,0.557142857142857,
0.571428571428571,0.585714285714286,0.6,0.614285714285714,0.628571428571428,
0.642857142857142,0.657142857142857,0.671428571428571,0.685714285714285,
0.699999999999999,0.714285714285714,0.728571428571428,0.742857142857142,
0.757142857142856,0.771428571428571,0.785714285714285,0.799999999999999,
0.814285714285713,0.828571428571428,0.842857142857142,0.857142857142856,
0.87142857142857,0.885714285714284,0.899999999999999,0.914285714285713,
0.928571428571427,0.942857142857141,0.957142857142856,0.97142857142857,
1.),.UNSPECIFIED.);
#599=B_SPLINE_CURVE_WITH_KNOTS('',5,(#36295,#36296,#36297,#36298,#36299,
#36300,#36301,#36302,#36303,#36304,#36305,#36306,#36307,#36308,#36309,#36310,
#36311,#36312,#36313,#36314,#36315,#36316,#36317,#36318,#36319,#36320,#36321,
#36322,#36323,#36324,#36325,#36326,#36327,#36328,#36329,#36330,#36331,#36332,
#36333,#36334,#36335,#36336,#36337,#36338,#36339,#36340,#36341,#36342,#36343,
#36344,#36345,#36346,#36347,#36348,#36349,#36350,#36351,#36352,#36353,#36354,
#36355,#36356,#36357,#36358,#36359,#36360,#36361,#36362,#36363,#36364,#36365,
#36366,#36367,#36368),.UNSPECIFIED.,.F.,.F.,(6,1,1,1,1,1,1,1,1,1,1,1,1,
1,1,1,1,1,1,1,1,1,1,1,1,1,1,1,1,1,1,1,1,1,1,1,1,1,1,1,1,1,1,1,1,1,1,1,1,
1,1,1,1,1,1,1,1,1,1,1,1,1,1,1,1,1,1,1,1,6),(0.,0.0142857142857143,0.0285714285714286,
0.0428571428571429,0.0571428571428571,0.0714285714285714,0.0857142857142857,
0.1,0.114285714285714,0.128571428571429,0.142857142857143,0.157142857142857,
0.171428571428571,0.185714285714286,0.2,0.214285714285714,0.228571428571429,
0.242857142857143,0.257142857142857,0.271428571428571,0.285714285714286,
0.3,0.314285714285714,0.328571428571429,0.342857142857143,0.357142857142857,
0.371428571428571,0.385714285714286,0.4,0.414285714285714,0.428571428571429,
0.442857142857143,0.457142857142857,0.471428571428572,0.485714285714286,
0.5,0.514285714285714,0.528571428571429,0.542857142857143,0.557142857142857,
0.571428571428571,0.585714285714286,0.6,0.614285714285714,0.628571428571428,
0.642857142857142,0.657142857142857,0.671428571428571,0.685714285714285,
0.699999999999999,0.714285714285714,0.728571428571428,0.742857142857142,
0.757142857142856,0.771428571428571,0.785714285714285,0.799999999999999,
0.814285714285713,0.828571428571428,0.842857142857142,0.857142857142856,
0.87142857142857,0.885714285714284,0.899999999999999,0.914285714285713,
0.928571428571427,0.942857142857141,0.957142857142856,0.97142857142857,
1.),.UNSPECIFIED.);
#600=B_SPLINE_CURVE_WITH_KNOTS('',5,(#36370,#36371,#36372,#36373,#36374,
#36375,#36376,#36377,#36378,#36379,#36380,#36381,#36382,#36383,#36384,#36385,
#36386,#36387,#36388,#36389,#36390,#36391,#36392,#36393,#36394,#36395,#36396,
#36397,#36398,#36399,#36400,#36401,#36402,#36403,#36404,#36405,#36406,#36407,
#36408,#36409,#36410,#36411,#36412,#36413,#36414,#36415,#36416,#36417,#36418,
#36419,#36420,#36421,#36422,#36423,#36424,#36425,#36426,#36427,#36428,#36429,
#36430,#36431,#36432,#36433,#36434,#36435,#36436,#36437,#36438,#36439,#36440,
#36441,#36442,#36443,#36444),.UNSPECIFIED.,.F.,.F.,(6,1,1,1,1,1,1,1,1,1,
1,1,1,1,1,1,1,1,1,1,1,1,1,1,1,1,1,1,1,1,1,1,1,1,1,1,1,1,1,1,1,1,1,1,1,1,
1,1,1,1,1,1,1,1,1,1,1,1,1,1,1,1,1,1,1,1,1,1,1,1,6),(-1.,-0.985714285714284,
-0.97142857142857,-0.957142857142856,-0.942857142857141,-0.928571428571427,
-0.914285714285713,-0.899999999999999,-0.885714285714284,-0.87142857142857,
-0.857142857142856,-0.842857142857142,-0.828571428571428,-0.814285714285713,
-0.799999999999999,-0.785714285714285,-0.771428571428571,-0.757142857142856,
-0.742857142857142,-0.728571428571428,-0.714285714285714,-0.699999999999999,
-0.685714285714285,-0.671428571428571,-0.657142857142857,-0.642857142857142,
-0.628571428571428,-0.614285714285714,-0.6,-0.585714285714286,-0.571428571428571,
-0.557142857142857,-0.542857142857143,-0.528571428571429,-0.514285714285714,
-0.5,-0.485714285714286,-0.471428571428572,-0.457142857142857,-0.442857142857143,
-0.428571428571429,-0.414285714285714,-0.4,-0.385714285714286,-0.371428571428571,
-0.357142857142857,-0.342857142857143,-0.328571428571429,-0.314285714285714,
-0.3,-0.285714285714286,-0.271428571428571,-0.257142857142857,-0.242857142857143,
-0.228571428571429,-0.214285714285714,-0.2,-0.185714285714286,-0.171428571428571,
-0.157142857142857,-0.142857142857143,-0.128571428571429,-0.114285714285714,
-0.1,-0.0857142857142857,-0.0714285714285714,-0.0571428571428571,-0.0428571428571429,
-0.0285714285714286,-0.0142857142857143,0.),.UNSPECIFIED.);
#601=B_SPLINE_CURVE_WITH_KNOTS('',5,(#36602,#36603,#36604,#36605,#36606,
#36607,#36608,#36609,#36610,#36611,#36612,#36613,#36614,#36615,#36616,#36617,
#36618,#36619,#36620,#36621,#36622,#36623,#36624,#36625,#36626,#36627,#36628,
#36629,#36630,#36631,#36632,#36633,#36634,#36635,#36636,#36637,#36638,#36639,
#36640,#36641,#36642,#36643,#36644,#36645,#36646,#36647,#36648,#36649,#36650,
#36651,#36652,#36653,#36654,#36655,#36656,#36657,#36658,#36659,#36660,#36661,
#36662,#36663,#36664,#36665,#36666,#36667,#36668,#36669,#36670,#36671,#36672,
#36673,#36674,#36675),.UNSPECIFIED.,.F.,.F.,(6,1,1,1,1,1,1,1,1,1,1,1,1,
1,1,1,1,1,1,1,1,1,1,1,1,1,1,1,1,1,1,1,1,1,1,1,1,1,1,1,1,1,1,1,1,1,1,1,1,
1,1,1,1,1,1,1,1,1,1,1,1,1,1,1,1,1,1,1,1,6),(0.,0.0142857142857143,0.0285714285714286,
0.0428571428571429,0.0571428571428571,0.0714285714285714,0.0857142857142857,
0.1,0.114285714285714,0.128571428571429,0.142857142857143,0.157142857142857,
0.171428571428571,0.185714285714286,0.2,0.214285714285714,0.228571428571429,
0.242857142857143,0.257142857142857,0.271428571428571,0.285714285714286,
0.3,0.314285714285714,0.328571428571429,0.342857142857143,0.357142857142857,
0.371428571428571,0.385714285714286,0.4,0.414285714285714,0.428571428571429,
0.442857142857143,0.457142857142857,0.471428571428572,0.485714285714286,
0.5,0.514285714285714,0.528571428571429,0.542857142857143,0.557142857142857,
0.571428571428571,0.585714285714286,0.6,0.614285714285714,0.628571428571428,
0.642857142857142,0.657142857142857,0.671428571428571,0.685714285714285,
0.699999999999999,0.714285714285714,0.728571428571428,0.742857142857142,
0.757142857142856,0.771428571428571,0.785714285714285,0.799999999999999,
0.814285714285713,0.828571428571428,0.842857142857142,0.857142857142856,
0.87142857142857,0.885714285714284,0.899999999999999,0.914285714285713,
0.928571428571427,0.942857142857141,0.957142857142856,0.97142857142857,
1.),.UNSPECIFIED.);
#602=B_SPLINE_CURVE_WITH_KNOTS('',5,(#36676,#36677,#36678,#36679,#36680,
#36681,#36682,#36683,#36684,#36685,#36686,#36687,#36688,#36689,#36690,#36691,
#36692,#36693,#36694,#36695,#36696,#36697,#36698,#36699,#36700,#36701,#36702,
#36703,#36704,#36705,#36706,#36707,#36708,#36709,#36710,#36711,#36712,#36713,
#36714,#36715,#36716,#36717,#36718,#36719,#36720,#36721,#36722,#36723,#36724,
#36725,#36726,#36727,#36728,#36729,#36730,#36731,#36732,#36733,#36734,#36735,
#36736,#36737,#36738,#36739,#36740,#36741,#36742,#36743,#36744,#36745,#36746,
#36747,#36748,#36749),.UNSPECIFIED.,.F.,.F.,(6,1,1,1,1,1,1,1,1,1,1,1,1,
1,1,1,1,1,1,1,1,1,1,1,1,1,1,1,1,1,1,1,1,1,1,1,1,1,1,1,1,1,1,1,1,1,1,1,1,
1,1,1,1,1,1,1,1,1,1,1,1,1,1,1,1,1,1,1,1,6),(0.,0.0142857142857143,0.0285714285714286,
0.0428571428571429,0.0571428571428571,0.0714285714285714,0.0857142857142857,
0.1,0.114285714285714,0.128571428571429,0.142857142857143,0.157142857142857,
0.171428571428571,0.185714285714286,0.2,0.214285714285714,0.228571428571429,
0.242857142857143,0.257142857142857,0.271428571428571,0.285714285714286,
0.3,0.314285714285714,0.328571428571429,0.342857142857143,0.357142857142857,
0.371428571428571,0.385714285714286,0.4,0.414285714285714,0.428571428571429,
0.442857142857143,0.457142857142857,0.471428571428572,0.485714285714286,
0.5,0.514285714285714,0.528571428571429,0.542857142857143,0.557142857142857,
0.571428571428571,0.585714285714286,0.6,0.614285714285714,0.628571428571428,
0.642857142857142,0.657142857142857,0.671428571428571,0.685714285714285,
0.699999999999999,0.714285714285714,0.728571428571428,0.742857142857142,
0.757142857142856,0.771428571428571,0.785714285714285,0.799999999999999,
0.814285714285713,0.828571428571428,0.842857142857142,0.857142857142856,
0.87142857142857,0.885714285714284,0.899999999999999,0.914285714285713,
0.928571428571427,0.942857142857141,0.957142857142856,0.97142857142857,
1.),.UNSPECIFIED.);
#603=B_SPLINE_CURVE_WITH_KNOTS('',5,(#36901,#36902,#36903,#36904,#36905,
#36906,#36907,#36908,#36909,#36910,#36911,#36912,#36913,#36914,#36915,#36916,
#36917,#36918,#36919,#36920,#36921,#36922,#36923,#36924,#36925,#36926,#36927,
#36928,#36929,#36930,#36931,#36932,#36933,#36934,#36935,#36936,#36937,#36938,
#36939,#36940,#36941,#36942,#36943,#36944,#36945,#36946,#36947,#36948,#36949,
#36950,#36951,#36952,#36953,#36954,#36955,#36956,#36957,#36958,#36959,#36960,
#36961,#36962,#36963,#36964,#36965,#36966,#36967,#36968,#36969,#36970,#36971,
#36972,#36973,#36974),.UNSPECIFIED.,.F.,.F.,(6,1,1,1,1,1,1,1,1,1,1,1,1,
1,1,1,1,1,1,1,1,1,1,1,1,1,1,1,1,1,1,1,1,1,1,1,1,1,1,1,1,1,1,1,1,1,1,1,1,
1,1,1,1,1,1,1,1,1,1,1,1,1,1,1,1,1,1,1,1,6),(0.,0.0142857142857143,0.0285714285714286,
0.0428571428571429,0.0571428571428571,0.0714285714285714,0.0857142857142857,
0.1,0.114285714285714,0.128571428571429,0.142857142857143,0.157142857142857,
0.171428571428571,0.185714285714286,0.2,0.214285714285714,0.228571428571429,
0.242857142857143,0.257142857142857,0.271428571428571,0.285714285714286,
0.3,0.314285714285714,0.328571428571429,0.342857142857143,0.357142857142857,
0.371428571428571,0.385714285714286,0.4,0.414285714285714,0.428571428571429,
0.442857142857143,0.457142857142857,0.471428571428572,0.485714285714286,
0.5,0.514285714285714,0.528571428571429,0.542857142857143,0.557142857142857,
0.571428571428571,0.585714285714286,0.6,0.614285714285714,0.628571428571428,
0.642857142857142,0.657142857142857,0.671428571428571,0.685714285714285,
0.699999999999999,0.714285714285714,0.728571428571428,0.742857142857142,
0.757142857142856,0.771428571428571,0.785714285714285,0.799999999999999,
0.814285714285713,0.828571428571428,0.842857142857142,0.857142857142856,
0.87142857142857,0.885714285714284,0.899999999999999,0.914285714285713,
0.928571428571427,0.942857142857141,0.957142857142856,0.97142857142857,
1.),.UNSPECIFIED.);
#604=B_SPLINE_CURVE_WITH_KNOTS('',5,(#36976,#36977,#36978,#36979,#36980,
#36981,#36982,#36983,#36984,#36985,#36986,#36987,#36988,#36989,#36990,#36991,
#36992,#36993,#36994,#36995,#36996,#36997,#36998,#36999,#37000,#37001,#37002,
#37003,#37004,#37005,#37006,#37007,#37008,#37009,#37010,#37011,#37012,#37013,
#37014,#37015,#37016,#37017,#37018,#37019,#37020,#37021,#37022,#37023,#37024,
#37025,#37026,#37027,#37028,#37029,#37030,#37031,#37032,#37033,#37034,#37035,
#37036,#37037,#37038,#37039,#37040,#37041,#37042,#37043,#37044,#37045,#37046,
#37047,#37048,#37049,#37050),.UNSPECIFIED.,.F.,.F.,(6,1,1,1,1,1,1,1,1,1,
1,1,1,1,1,1,1,1,1,1,1,1,1,1,1,1,1,1,1,1,1,1,1,1,1,1,1,1,1,1,1,1,1,1,1,1,
1,1,1,1,1,1,1,1,1,1,1,1,1,1,1,1,1,1,1,1,1,1,1,1,6),(-1.,-0.985714285714284,
-0.97142857142857,-0.957142857142856,-0.942857142857141,-0.928571428571427,
-0.914285714285713,-0.899999999999999,-0.885714285714284,-0.87142857142857,
-0.857142857142856,-0.842857142857142,-0.828571428571428,-0.814285714285713,
-0.799999999999999,-0.785714285714285,-0.771428571428571,-0.757142857142856,
-0.742857142857142,-0.728571428571428,-0.714285714285714,-0.699999999999999,
-0.685714285714285,-0.671428571428571,-0.657142857142857,-0.642857142857142,
-0.628571428571428,-0.614285714285714,-0.6,-0.585714285714286,-0.571428571428571,
-0.557142857142857,-0.542857142857143,-0.528571428571429,-0.514285714285714,
-0.5,-0.485714285714286,-0.471428571428572,-0.457142857142857,-0.442857142857143,
-0.428571428571429,-0.414285714285714,-0.4,-0.385714285714286,-0.371428571428571,
-0.357142857142857,-0.342857142857143,-0.328571428571429,-0.314285714285714,
-0.3,-0.285714285714286,-0.271428571428571,-0.257142857142857,-0.242857142857143,
-0.228571428571429,-0.214285714285714,-0.2,-0.185714285714286,-0.171428571428571,
-0.157142857142857,-0.142857142857143,-0.128571428571429,-0.114285714285714,
-0.1,-0.0857142857142857,-0.0714285714285714,-0.0571428571428571,-0.0428571428571429,
-0.0285714285714286,-0.0142857142857143,0.),.UNSPECIFIED.);
#605=B_SPLINE_CURVE_WITH_KNOTS('',5,(#37208,#37209,#37210,#37211,#37212,
#37213,#37214,#37215,#37216,#37217,#37218,#37219,#37220,#37221,#37222,#37223,
#37224,#37225,#37226,#37227,#37228,#37229,#37230,#37231,#37232,#37233,#37234,
#37235,#37236,#37237,#37238,#37239,#37240,#37241,#37242,#37243,#37244,#37245,
#37246,#37247,#37248,#37249,#37250,#37251,#37252,#37253,#37254,#37255,#37256,
#37257,#37258,#37259,#37260,#37261,#37262,#37263,#37264,#37265,#37266,#37267,
#37268,#37269,#37270,#37271,#37272,#37273,#37274,#37275,#37276,#37277,#37278,
#37279,#37280,#37281),.UNSPECIFIED.,.F.,.F.,(6,1,1,1,1,1,1,1,1,1,1,1,1,
1,1,1,1,1,1,1,1,1,1,1,1,1,1,1,1,1,1,1,1,1,1,1,1,1,1,1,1,1,1,1,1,1,1,1,1,
1,1,1,1,1,1,1,1,1,1,1,1,1,1,1,1,1,1,1,1,6),(0.,0.0142857142857143,0.0285714285714286,
0.0428571428571429,0.0571428571428571,0.0714285714285714,0.0857142857142857,
0.1,0.114285714285714,0.128571428571429,0.142857142857143,0.157142857142857,
0.171428571428571,0.185714285714286,0.2,0.214285714285714,0.228571428571429,
0.242857142857143,0.257142857142857,0.271428571428571,0.285714285714286,
0.3,0.314285714285714,0.328571428571429,0.342857142857143,0.357142857142857,
0.371428571428571,0.385714285714286,0.4,0.414285714285714,0.428571428571429,
0.442857142857143,0.457142857142857,0.471428571428572,0.485714285714286,
0.5,0.514285714285714,0.528571428571429,0.542857142857143,0.557142857142857,
0.571428571428571,0.585714285714286,0.6,0.614285714285714,0.628571428571428,
0.642857142857142,0.657142857142857,0.671428571428571,0.685714285714285,
0.699999999999999,0.714285714285714,0.728571428571428,0.742857142857142,
0.757142857142856,0.771428571428571,0.785714285714285,0.799999999999999,
0.814285714285713,0.828571428571428,0.842857142857142,0.857142857142856,
0.87142857142857,0.885714285714284,0.899999999999999,0.914285714285713,
0.928571428571427,0.942857142857141,0.957142857142856,0.97142857142857,
1.),.UNSPECIFIED.);
#606=B_SPLINE_CURVE_WITH_KNOTS('',5,(#37282,#37283,#37284,#37285,#37286,
#37287,#37288,#37289,#37290,#37291,#37292,#37293,#37294,#37295,#37296,#37297,
#37298,#37299,#37300,#37301,#37302,#37303,#37304,#37305,#37306,#37307,#37308,
#37309,#37310,#37311,#37312,#37313,#37314,#37315,#37316,#37317,#37318,#37319,
#37320,#37321,#37322,#37323,#37324,#37325,#37326,#37327,#37328,#37329,#37330,
#37331,#37332,#37333,#37334,#37335,#37336,#37337,#37338,#37339,#37340,#37341,
#37342,#37343,#37344,#37345,#37346,#37347,#37348,#37349,#37350,#37351,#37352,
#37353,#37354,#37355),.UNSPECIFIED.,.F.,.F.,(6,1,1,1,1,1,1,1,1,1,1,1,1,
1,1,1,1,1,1,1,1,1,1,1,1,1,1,1,1,1,1,1,1,1,1,1,1,1,1,1,1,1,1,1,1,1,1,1,1,
1,1,1,1,1,1,1,1,1,1,1,1,1,1,1,1,1,1,1,1,6),(0.,0.0142857142857143,0.0285714285714286,
0.0428571428571429,0.0571428571428571,0.0714285714285714,0.0857142857142857,
0.1,0.114285714285714,0.128571428571429,0.142857142857143,0.157142857142857,
0.171428571428571,0.185714285714286,0.2,0.214285714285714,0.228571428571429,
0.242857142857143,0.257142857142857,0.271428571428571,0.285714285714286,
0.3,0.314285714285714,0.328571428571429,0.342857142857143,0.357142857142857,
0.371428571428571,0.385714285714286,0.4,0.414285714285714,0.428571428571429,
0.442857142857143,0.457142857142857,0.471428571428572,0.485714285714286,
0.5,0.514285714285714,0.528571428571429,0.542857142857143,0.557142857142857,
0.571428571428571,0.585714285714286,0.6,0.614285714285714,0.628571428571428,
0.642857142857142,0.657142857142857,0.671428571428571,0.685714285714285,
0.699999999999999,0.714285714285714,0.728571428571428,0.742857142857142,
0.757142857142856,0.771428571428571,0.785714285714285,0.799999999999999,
0.814285714285713,0.828571428571428,0.842857142857142,0.857142857142856,
0.87142857142857,0.885714285714284,0.899999999999999,0.914285714285713,
0.928571428571427,0.942857142857141,0.957142857142856,0.97142857142857,
1.),.UNSPECIFIED.);
#607=B_SPLINE_CURVE_WITH_KNOTS('',5,(#37371,#37372,#37373,#37374,#37375,
#37376,#37377,#37378,#37379,#37380,#37381,#37382,#37383,#37384,#37385,#37386,
#37387,#37388,#37389,#37390,#37391,#37392,#37393,#37394,#37395,#37396,#37397,
#37398,#37399,#37400,#37401,#37402,#37403,#37404,#37405,#37406,#37407,#37408,
#37409,#37410,#37411,#37412,#37413,#37414,#37415,#37416,#37417,#37418,#37419,
#37420,#37421,#37422,#37423,#37424,#37425,#37426,#37427,#37428,#37429,#37430,
#37431,#37432,#37433,#37434,#37435,#37436,#37437,#37438,#37439,#37440,#37441,
#37442,#37443,#37444),.UNSPECIFIED.,.F.,.F.,(6,1,1,1,1,1,1,1,1,1,1,1,1,
1,1,1,1,1,1,1,1,1,1,1,1,1,1,1,1,1,1,1,1,1,1,1,1,1,1,1,1,1,1,1,1,1,1,1,1,
1,1,1,1,1,1,1,1,1,1,1,1,1,1,1,1,1,1,1,1,6),(0.,0.0142857142857143,0.0285714285714286,
0.0428571428571429,0.0571428571428571,0.0714285714285714,0.0857142857142857,
0.1,0.114285714285714,0.128571428571429,0.142857142857143,0.157142857142857,
0.171428571428571,0.185714285714286,0.2,0.214285714285714,0.228571428571429,
0.242857142857143,0.257142857142857,0.271428571428571,0.285714285714286,
0.3,0.314285714285714,0.328571428571429,0.342857142857143,0.357142857142857,
0.371428571428571,0.385714285714286,0.4,0.414285714285714,0.428571428571429,
0.442857142857143,0.457142857142857,0.471428571428572,0.485714285714286,
0.5,0.514285714285714,0.528571428571429,0.542857142857143,0.557142857142857,
0.571428571428571,0.585714285714286,0.6,0.614285714285714,0.628571428571428,
0.642857142857142,0.657142857142857,0.671428571428571,0.685714285714285,
0.699999999999999,0.714285714285714,0.728571428571428,0.742857142857142,
0.757142857142856,0.771428571428571,0.785714285714285,0.799999999999999,
0.814285714285713,0.828571428571428,0.842857142857142,0.857142857142856,
0.87142857142857,0.885714285714284,0.899999999999999,0.914285714285713,
0.928571428571427,0.942857142857141,0.957142857142856,0.97142857142857,
1.),.UNSPECIFIED.);
#608=B_SPLINE_CURVE_WITH_KNOTS('',5,(#37448,#37449,#37450,#37451,#37452,
#37453,#37454,#37455,#37456,#37457,#37458,#37459,#37460,#37461,#37462,#37463,
#37464,#37465,#37466,#37467,#37468,#37469,#37470,#37471,#37472,#37473,#37474,
#37475,#37476,#37477,#37478,#37479,#37480,#37481,#37482,#37483,#37484,#37485,
#37486,#37487,#37488,#37489,#37490,#37491,#37492,#37493,#37494,#37495,#37496,
#37497,#37498,#37499,#37500,#37501,#37502,#37503,#37504,#37505,#37506,#37507,
#37508,#37509,#37510,#37511,#37512,#37513,#37514,#37515,#37516,#37517,#37518,
#37519,#37520,#37521),.UNSPECIFIED.,.F.,.F.,(6,1,1,1,1,1,1,1,1,1,1,1,1,
1,1,1,1,1,1,1,1,1,1,1,1,1,1,1,1,1,1,1,1,1,1,1,1,1,1,1,1,1,1,1,1,1,1,1,1,
1,1,1,1,1,1,1,1,1,1,1,1,1,1,1,1,1,1,1,1,6),(0.,0.0142857142857143,0.0285714285714286,
0.0428571428571429,0.0571428571428571,0.0714285714285714,0.0857142857142857,
0.1,0.114285714285714,0.128571428571429,0.142857142857143,0.157142857142857,
0.171428571428571,0.185714285714286,0.2,0.214285714285714,0.228571428571429,
0.242857142857143,0.257142857142857,0.271428571428571,0.285714285714286,
0.3,0.314285714285714,0.328571428571429,0.342857142857143,0.357142857142857,
0.371428571428571,0.385714285714286,0.4,0.414285714285714,0.428571428571429,
0.442857142857143,0.457142857142857,0.471428571428572,0.485714285714286,
0.5,0.514285714285714,0.528571428571429,0.542857142857143,0.557142857142857,
0.571428571428571,0.585714285714286,0.6,0.614285714285714,0.628571428571428,
0.642857142857142,0.657142857142857,0.671428571428571,0.685714285714285,
0.699999999999999,0.714285714285714,0.728571428571428,0.742857142857142,
0.757142857142856,0.771428571428571,0.785714285714285,0.799999999999999,
0.814285714285713,0.828571428571428,0.842857142857142,0.857142857142856,
0.87142857142857,0.885714285714284,0.899999999999999,0.914285714285713,
0.928571428571427,0.942857142857141,0.957142857142856,0.97142857142857,
1.),.UNSPECIFIED.);
#609=B_SPLINE_CURVE_WITH_KNOTS('',5,(#37536,#37537,#37538,#37539,#37540,
#37541,#37542,#37543,#37544,#37545,#37546,#37547,#37548,#37549,#37550,#37551,
#37552,#37553,#37554,#37555,#37556,#37557,#37558,#37559,#37560,#37561,#37562,
#37563,#37564,#37565,#37566,#37567,#37568,#37569,#37570,#37571,#37572,#37573,
#37574,#37575,#37576,#37577,#37578,#37579,#37580,#37581,#37582,#37583,#37584,
#37585,#37586,#37587,#37588,#37589,#37590,#37591,#37592,#37593,#37594,#37595,
#37596,#37597,#37598,#37599,#37600,#37601,#37602,#37603,#37604,#37605,#37606,
#37607,#37608,#37609),.UNSPECIFIED.,.F.,.F.,(6,1,1,1,1,1,1,1,1,1,1,1,1,
1,1,1,1,1,1,1,1,1,1,1,1,1,1,1,1,1,1,1,1,1,1,1,1,1,1,1,1,1,1,1,1,1,1,1,1,
1,1,1,1,1,1,1,1,1,1,1,1,1,1,1,1,1,1,1,1,6),(0.,0.0142857142857143,0.0285714285714286,
0.0428571428571429,0.0571428571428571,0.0714285714285714,0.0857142857142857,
0.1,0.114285714285714,0.128571428571429,0.142857142857143,0.157142857142857,
0.171428571428571,0.185714285714286,0.2,0.214285714285714,0.228571428571429,
0.242857142857143,0.257142857142857,0.271428571428571,0.285714285714286,
0.3,0.314285714285714,0.328571428571429,0.342857142857143,0.357142857142857,
0.371428571428571,0.385714285714286,0.4,0.414285714285714,0.428571428571429,
0.442857142857143,0.457142857142857,0.471428571428572,0.485714285714286,
0.5,0.514285714285714,0.528571428571429,0.542857142857143,0.557142857142857,
0.571428571428571,0.585714285714286,0.6,0.614285714285714,0.628571428571428,
0.642857142857142,0.657142857142857,0.671428571428571,0.685714285714285,
0.699999999999999,0.714285714285714,0.728571428571428,0.742857142857142,
0.757142857142856,0.771428571428571,0.785714285714285,0.799999999999999,
0.814285714285713,0.828571428571428,0.842857142857142,0.857142857142856,
0.87142857142857,0.885714285714284,0.899999999999999,0.914285714285713,
0.928571428571427,0.942857142857141,0.957142857142856,0.97142857142857,
1.),.UNSPECIFIED.);
#610=B_SPLINE_CURVE_WITH_KNOTS('',5,(#37613,#37614,#37615,#37616,#37617,
#37618,#37619,#37620,#37621,#37622,#37623,#37624,#37625,#37626,#37627,#37628,
#37629,#37630,#37631,#37632,#37633,#37634,#37635,#37636,#37637,#37638,#37639,
#37640,#37641,#37642,#37643,#37644,#37645,#37646,#37647,#37648,#37649,#37650,
#37651,#37652,#37653,#37654,#37655,#37656,#37657,#37658,#37659,#37660,#37661,
#37662,#37663,#37664,#37665,#37666,#37667,#37668,#37669,#37670,#37671,#37672,
#37673,#37674,#37675,#37676,#37677,#37678,#37679,#37680,#37681,#37682,#37683,
#37684,#37685,#37686,#37687),.UNSPECIFIED.,.F.,.F.,(6,1,1,1,1,1,1,1,1,1,
1,1,1,1,1,1,1,1,1,1,1,1,1,1,1,1,1,1,1,1,1,1,1,1,1,1,1,1,1,1,1,1,1,1,1,1,
1,1,1,1,1,1,1,1,1,1,1,1,1,1,1,1,1,1,1,1,1,1,1,1,6),(-1.,-0.985714285714284,
-0.97142857142857,-0.957142857142856,-0.942857142857141,-0.928571428571427,
-0.914285714285713,-0.899999999999999,-0.885714285714284,-0.87142857142857,
-0.857142857142856,-0.842857142857142,-0.828571428571428,-0.814285714285713,
-0.799999999999999,-0.785714285714285,-0.771428571428571,-0.757142857142856,
-0.742857142857142,-0.728571428571428,-0.714285714285714,-0.699999999999999,
-0.685714285714285,-0.671428571428571,-0.657142857142857,-0.642857142857142,
-0.628571428571428,-0.614285714285714,-0.6,-0.585714285714286,-0.571428571428571,
-0.557142857142857,-0.542857142857143,-0.528571428571429,-0.514285714285714,
-0.5,-0.485714285714286,-0.471428571428572,-0.457142857142857,-0.442857142857143,
-0.428571428571429,-0.414285714285714,-0.4,-0.385714285714286,-0.371428571428571,
-0.357142857142857,-0.342857142857143,-0.328571428571429,-0.314285714285714,
-0.3,-0.285714285714286,-0.271428571428571,-0.257142857142857,-0.242857142857143,
-0.228571428571429,-0.214285714285714,-0.2,-0.185714285714286,-0.171428571428571,
-0.157142857142857,-0.142857142857143,-0.128571428571429,-0.114285714285714,
-0.1,-0.0857142857142857,-0.0714285714285714,-0.0571428571428571,-0.0428571428571429,
-0.0285714285714286,-0.0142857142857143,0.),.UNSPECIFIED.);
#611=B_SPLINE_CURVE_WITH_KNOTS('',3,(#38185,#38186,#38187,#38188,#38189,
#38190),.UNSPECIFIED.,.F.,.F.,(4,2,4),(0.436494357616827,0.49057908163088,
0.523269669927392),.UNSPECIFIED.);
#612=B_SPLINE_CURVE_WITH_KNOTS('',3,(#38192,#38193,#38194,#38195,#38196,
#38197,#38198,#38199,#38200,#38201,#38202,#38203,#38204,#38205,#38206,#38207,
#38208,#38209,#38210),.UNSPECIFIED.,.F.,.F.,(4,3,3,3,3,3,4),(1.21344063784114,
1.25510987200879,1.29073244309217,1.33189452838103,1.37317594357341,1.41463545273866,
1.43283480298246),.UNSPECIFIED.);
#613=B_SPLINE_CURVE_WITH_KNOTS('',3,(#38212,#38213,#38214,#38215,#38216,
#38217),.UNSPECIFIED.,.F.,.F.,(4,2,4),(0.436494357616828,0.49057908163088,
0.523269669927516),.UNSPECIFIED.);
#614=B_SPLINE_CURVE_WITH_KNOTS('',3,(#38218,#38219,#38220,#38221,#38222,
#38223,#38224,#38225,#38226,#38227,#38228,#38229,#38230,#38231,#38232,#38233,
#38234,#38235,#38236),.UNSPECIFIED.,.F.,.F.,(4,3,3,3,3,3,4),(-1.40481265039417,
-1.36522996541144,-1.32585540726346,-1.28679683363995,-1.26015734748852,
-1.21999608757349,-1.1843388203003),.UNSPECIFIED.);
#615=B_SPLINE_CURVE_WITH_KNOTS('',3,(#38239,#38240,#38241,#38242,#38243,
#38244),.UNSPECIFIED.,.F.,.F.,(4,2,4),(1.43904665659616,1.47173724489264,
1.52582196890669),.UNSPECIFIED.);
#616=B_SPLINE_CURVE_WITH_KNOTS('',3,(#38246,#38247,#38248,#38249,#38250,
#38251,#38252,#38253,#38254,#38255,#38256,#38257,#38258,#38259,#38260,#38261,
#38262,#38263,#38264),.UNSPECIFIED.,.F.,.F.,(4,3,3,3,3,3,4),(-0.110253525235352,
-0.070240741437667,-0.0308586443223014,0.,0.0392000421916667,0.0788707706427855,
0.110060546834446),.UNSPECIFIED.);
#617=B_SPLINE_CURVE_WITH_KNOTS('',3,(#38266,#38267,#38268,#38269,#38270,
#38271),.UNSPECIFIED.,.F.,.F.,(4,2,4),(1.43904665659616,1.47173724489264,
1.52582196890582),.UNSPECIFIED.);
#618=B_SPLINE_CURVE_WITH_KNOTS('',3,(#38272,#38273,#38274,#38275,#38276,
#38277,#38278,#38279,#38280,#38281,#38282,#38283,#38284,#38285,#38286,#38287,
#38288,#38289,#38290),.UNSPECIFIED.,.F.,.F.,(4,3,3,3,3,3,4),(2.53632937909178,
2.57775416224765,2.61898206719527,2.6459019021663,2.68717408326041,2.72876559667488,
2.75562831582286),.UNSPECIFIED.);
#619=B_SPLINE_CURVE_WITH_KNOTS('',3,(#38300,#38301,#38302,#38303,#38304,
#38305,#38306),.UNSPECIFIED.,.F.,.F.,(4,3,4),(1.98904556960248,2.09488046175532,
2.20071535390815),.UNSPECIFIED.);
#620=B_SPLINE_CURVE_WITH_KNOTS('',3,(#38310,#38311,#38312,#38313,#38314,
#38315,#38316),.UNSPECIFIED.,.F.,.F.,(4,3,4),(-0.105611957753097,0.,0.105611957753097),
 .UNSPECIFIED.);
#621=B_SPLINE_CURVE_WITH_KNOTS('',3,(#38321,#38322,#38323,#38324,#38325,
#38326),.UNSPECIFIED.,.F.,.F.,(4,2,4),(-1.17106027221854,-1.06544831446544,
-0.959836356712345),.UNSPECIFIED.);
#622=B_SPLINE_CURVE_WITH_KNOTS('',3,(#38329,#38330,#38331,#38332,#38333,
#38334),.UNSPECIFIED.,.F.,.F.,(4,2,4),(0.941605338724826,1.04744023087766,
1.15327512303049),.UNSPECIFIED.);
#623=B_SPLINE_CURVE_WITH_KNOTS('',3,(#38347,#38348,#38349,#38350,#38351,
#38352),.UNSPECIFIED.,.F.,.F.,(4,2,4),(0.436494357616816,0.49057908163088,
0.523269669927352),.UNSPECIFIED.);
#624=B_SPLINE_CURVE_WITH_KNOTS('',3,(#38354,#38355,#38356,#38357,#38358,
#38359,#38360,#38361,#38362,#38363,#38364,#38365,#38366,#38367,#38368,#38369,
#38370,#38371,#38372),.UNSPECIFIED.,.F.,.F.,(4,3,3,3,3,3,4),(1.21344063784117,
1.2551098720088,1.29073244309219,1.33189452838105,1.37317594357344,1.41463545273871,
1.43283480298249),.UNSPECIFIED.);
#625=B_SPLINE_CURVE_WITH_KNOTS('',3,(#38374,#38375,#38376,#38377,#38378,
#38379),.UNSPECIFIED.,.F.,.F.,(4,2,4),(0.436484426249651,0.490578640084517,
0.523250481795878),.UNSPECIFIED.);
#626=B_SPLINE_CURVE_WITH_KNOTS('',3,(#38380,#38381,#38382,#38383,#38384,
#38385,#38386,#38387,#38388,#38389,#38390,#38391,#38392,#38393,#38394,#38395,
#38396,#38397,#38398),.UNSPECIFIED.,.F.,.F.,(4,3,3,3,3,3,4),(-1.40481265039413,
-1.36522996541145,-1.32585540726349,-1.28679683363998,-1.2601573474885,
-1.21999608757352,-1.18433882030031),.UNSPECIFIED.);
#627=B_SPLINE_CURVE_WITH_KNOTS('',3,(#38401,#38402,#38403,#38404,#38405,
#38406),.UNSPECIFIED.,.F.,.F.,(4,2,4),(1.43906407854219,1.47173592025355,
1.52583013408841),.UNSPECIFIED.);
#628=B_SPLINE_CURVE_WITH_KNOTS('',3,(#38408,#38409,#38410,#38411,#38412,
#38413,#38414,#38415,#38416,#38417,#38418,#38419,#38420,#38421,#38422,#38423,
#38424,#38425,#38426),.UNSPECIFIED.,.F.,.F.,(4,3,3,3,3,3,4),(-0.110253525235351,
-0.0702407414376934,-0.0308586443223274,0.,0.0392000421916682,0.0788707706427895,
0.110060546834446),.UNSPECIFIED.);
#629=B_SPLINE_CURVE_WITH_KNOTS('',3,(#38428,#38429,#38430,#38431,#38432,
#38433),.UNSPECIFIED.,.F.,.F.,(4,2,4),(1.43906407854219,1.47173592025355,
1.52583013408754),.UNSPECIFIED.);
#630=B_SPLINE_CURVE_WITH_KNOTS('',3,(#38434,#38435,#38436,#38437,#38438,
#38439,#38440,#38441,#38442,#38443,#38444,#38445,#38446,#38447,#38448,#38449,
#38450,#38451,#38452),.UNSPECIFIED.,.F.,.F.,(4,3,3,3,3,3,4),(2.53632937909181,
2.57775416224765,2.61898206719527,2.64590190216633,2.68717408326044,2.72876559667489,
2.75562831582288),.UNSPECIFIED.);
#631=B_SPLINE_CURVE_WITH_KNOTS('',3,(#38462,#38463,#38464,#38465,#38466,
#38467,#38468),.UNSPECIFIED.,.F.,.F.,(4,3,4),(1.98904556960249,2.09488046175532,
2.20071535390816),.UNSPECIFIED.);
#632=B_SPLINE_CURVE_WITH_KNOTS('',3,(#38472,#38473,#38474,#38475,#38476,
#38477,#38478),.UNSPECIFIED.,.F.,.F.,(4,3,4),(-0.105611957753097,0.,0.105611957753097),
 .UNSPECIFIED.);
#633=B_SPLINE_CURVE_WITH_KNOTS('',3,(#38483,#38484,#38485,#38486,#38487,
#38488),.UNSPECIFIED.,.F.,.F.,(4,2,4),(-1.17106027221854,-1.06544831446544,
-0.959836356712344),.UNSPECIFIED.);
#634=B_SPLINE_CURVE_WITH_KNOTS('',3,(#38491,#38492,#38493,#38494,#38495,
#38496),.UNSPECIFIED.,.F.,.F.,(4,2,4),(0.941605338724829,1.04744023087766,
1.15327512303049),.UNSPECIFIED.);
#635=B_SPLINE_CURVE_WITH_KNOTS('',3,(#38509,#38510,#38511,#38512,#38513,
#38514),.UNSPECIFIED.,.F.,.F.,(4,2,4),(0.436484426249655,0.490578640084517,
0.523250481795882),.UNSPECIFIED.);
#636=B_SPLINE_CURVE_WITH_KNOTS('',3,(#38516,#38517,#38518,#38519,#38520,
#38521,#38522,#38523,#38524,#38525,#38526,#38527,#38528,#38529,#38530,#38531,
#38532,#38533,#38534),.UNSPECIFIED.,.F.,.F.,(4,3,3,3,3,3,4),(2.53632937909178,
2.57775416224762,2.61898206719525,2.64590190216632,2.68717408326042,2.72876559667488,
2.75562831582289),.UNSPECIFIED.);
#637=B_SPLINE_CURVE_WITH_KNOTS('',3,(#38536,#38537,#38538,#38539,#38540,
#38541),.UNSPECIFIED.,.F.,.F.,(4,2,4),(0.436494357616821,0.49057908163088,
0.523269669927365),.UNSPECIFIED.);
#638=B_SPLINE_CURVE_WITH_KNOTS('',3,(#38542,#38543,#38544,#38545,#38546,
#38547,#38548,#38549,#38550,#38551,#38552,#38553,#38554,#38555,#38556,#38557,
#38558,#38559,#38560),.UNSPECIFIED.,.F.,.F.,(4,3,3,3,3,3,4),(-0.110253525235353,
-0.0702407414376493,-0.0308586443222864,0.,0.0392000421916586,0.0788707706427754,
0.110060546834447),.UNSPECIFIED.);
#639=B_SPLINE_CURVE_WITH_KNOTS('',3,(#38563,#38564,#38565,#38566,#38567,
#38568),.UNSPECIFIED.,.F.,.F.,(4,2,4),(1.43906407854219,1.47173592025355,
1.52583013408841),.UNSPECIFIED.);
#640=B_SPLINE_CURVE_WITH_KNOTS('',3,(#38570,#38571,#38572,#38573,#38574,
#38575,#38576,#38577,#38578,#38579,#38580,#38581,#38582,#38583,#38584,#38585,
#38586,#38587,#38588),.UNSPECIFIED.,.F.,.F.,(4,3,3,3,3,3,4),(-1.40481265039415,
-1.36522996541142,-1.32585540726345,-1.28679683363994,-1.26015734748852,
-1.21999608757345,-1.18433882030032),.UNSPECIFIED.);
#641=B_SPLINE_CURVE_WITH_KNOTS('',3,(#38590,#38591,#38592,#38593,#38594,
#38595),.UNSPECIFIED.,.F.,.F.,(4,2,4),(1.43906407854219,1.47173592025355,
1.52583013408753),.UNSPECIFIED.);
#642=B_SPLINE_CURVE_WITH_KNOTS('',3,(#38596,#38597,#38598,#38599,#38600,
#38601,#38602,#38603,#38604,#38605,#38606,#38607,#38608,#38609,#38610,#38611,
#38612,#38613,#38614),.UNSPECIFIED.,.F.,.F.,(4,3,3,3,3,3,4),(1.21344063784118,
1.25510987200885,1.29073244309219,1.33189452838105,1.37317594357345,1.41463545273868,
1.43283480298247),.UNSPECIFIED.);
#643=B_SPLINE_CURVE_WITH_KNOTS('',3,(#38624,#38625,#38626,#38627,#38628,
#38629,#38630),.UNSPECIFIED.,.F.,.F.,(4,3,4),(1.98904556960249,2.09488046175532,
2.20071535390815),.UNSPECIFIED.);
#644=B_SPLINE_CURVE_WITH_KNOTS('',3,(#38634,#38635,#38636,#38637,#38638,
#38639,#38640),.UNSPECIFIED.,.F.,.F.,(4,3,4),(-0.105611957753096,0.,0.105611957753097),
 .UNSPECIFIED.);
#645=B_SPLINE_CURVE_WITH_KNOTS('',3,(#38645,#38646,#38647,#38648,#38649,
#38650),.UNSPECIFIED.,.F.,.F.,(4,2,4),(-1.17106027221854,-1.06544831446544,
-0.959836356712344),.UNSPECIFIED.);
#646=B_SPLINE_CURVE_WITH_KNOTS('',3,(#38653,#38654,#38655,#38656,#38657,
#38658),.UNSPECIFIED.,.F.,.F.,(4,2,4),(0.941605338724827,1.04744023087766,
1.15327512303049),.UNSPECIFIED.);
#647=B_SPLINE_CURVE_WITH_KNOTS('',3,(#38671,#38672,#38673,#38674,#38675,
#38676),.UNSPECIFIED.,.F.,.F.,(4,2,4),(0.436494357616822,0.49057908163088,
0.523269669927398),.UNSPECIFIED.);
#648=B_SPLINE_CURVE_WITH_KNOTS('',3,(#38678,#38679,#38680,#38681,#38682,
#38683,#38684,#38685,#38686,#38687,#38688,#38689,#38690,#38691,#38692,#38693,
#38694,#38695,#38696),.UNSPECIFIED.,.F.,.F.,(4,3,3,3,3,3,4),(2.53632937909185,
2.57775416224773,2.61898206719535,2.64590190216638,2.6871740832605,2.72876559667492,
2.75562831582295),.UNSPECIFIED.);
#649=B_SPLINE_CURVE_WITH_KNOTS('',3,(#38698,#38699,#38700,#38701,#38702,
#38703),.UNSPECIFIED.,.F.,.F.,(4,2,4),(0.436484426249657,0.490578640084517,
0.523250481796065),.UNSPECIFIED.);
#650=B_SPLINE_CURVE_WITH_KNOTS('',3,(#38704,#38705,#38706,#38707,#38708,
#38709,#38710,#38711,#38712,#38713,#38714,#38715,#38716,#38717,#38718,#38719,
#38720,#38721,#38722),.UNSPECIFIED.,.F.,.F.,(4,3,3,3,3,3,4),(-0.110253525235377,
-0.070240741437708,-0.0308586443223363,0.,0.03920004219167,0.0788707706428437,
0.110060546834472),.UNSPECIFIED.);
#651=B_SPLINE_CURVE_WITH_KNOTS('',3,(#38725,#38726,#38727,#38728,#38729,
#38730),.UNSPECIFIED.,.F.,.F.,(4,2,4),(1.43904665659616,1.47173724489264,
1.52582196890669),.UNSPECIFIED.);
#652=B_SPLINE_CURVE_WITH_KNOTS('',3,(#38732,#38733,#38734,#38735,#38736,
#38737,#38738,#38739,#38740,#38741,#38742,#38743,#38744,#38745,#38746,#38747,
#38748,#38749,#38750),.UNSPECIFIED.,.F.,.F.,(4,3,3,3,3,3,4),(-1.40481265039411,
-1.36522996541141,-1.32585540726345,-1.28679683363994,-1.26015734748849,
-1.21999608757351,-1.1843388203003),.UNSPECIFIED.);
#653=B_SPLINE_CURVE_WITH_KNOTS('',3,(#38752,#38753,#38754,#38755,#38756,
#38757),.UNSPECIFIED.,.F.,.F.,(4,2,4),(1.43904665659616,1.47173724489264,
1.52582196890583),.UNSPECIFIED.);
#654=B_SPLINE_CURVE_WITH_KNOTS('',3,(#38758,#38759,#38760,#38761,#38762,
#38763,#38764,#38765,#38766,#38767,#38768,#38769,#38770,#38771,#38772,#38773,
#38774,#38775,#38776),.UNSPECIFIED.,.F.,.F.,(4,3,3,3,3,3,4),(1.2134406378412,
1.25510987200883,1.29073244309221,1.33189452838107,1.37317594357346,1.41463545273868,
1.43283480298249),.UNSPECIFIED.);
#655=B_SPLINE_CURVE_WITH_KNOTS('',3,(#38786,#38787,#38788,#38789,#38790,
#38791,#38792),.UNSPECIFIED.,.F.,.F.,(4,3,4),(1.98904556960248,2.09488046175532,
2.20071535390815),.UNSPECIFIED.);
#656=B_SPLINE_CURVE_WITH_KNOTS('',3,(#38796,#38797,#38798,#38799,#38800,
#38801,#38802),.UNSPECIFIED.,.F.,.F.,(4,3,4),(-0.105611957753097,0.,0.105611957753097),
 .UNSPECIFIED.);
#657=B_SPLINE_CURVE_WITH_KNOTS('',3,(#38807,#38808,#38809,#38810,#38811,
#38812),.UNSPECIFIED.,.F.,.F.,(4,2,4),(-1.17106027221854,-1.06544831446544,
-0.959836356712344),.UNSPECIFIED.);
#658=B_SPLINE_CURVE_WITH_KNOTS('',3,(#38815,#38816,#38817,#38818,#38819,
#38820),.UNSPECIFIED.,.F.,.F.,(4,2,4),(0.941605338724826,1.04744023087766,
1.15327512303049),.UNSPECIFIED.);
#659=B_SPLINE_CURVE_WITH_KNOTS('',3,(#38833,#38834,#38835,#38836,#38837,
#38838),.UNSPECIFIED.,.F.,.F.,(4,2,4),(0.436494357616821,0.49057908163088,
0.523269669927355),.UNSPECIFIED.);
#660=B_SPLINE_CURVE_WITH_KNOTS('',3,(#38840,#38841,#38842,#38843,#38844,
#38845,#38846,#38847,#38848,#38849,#38850,#38851,#38852,#38853,#38854,#38855,
#38856,#38857,#38858),.UNSPECIFIED.,.F.,.F.,(4,3,3,3,3,3,4),(2.53632937909179,
2.57775416224772,2.61898206719534,2.64590190216632,2.68717408326042,2.72876559667486,
2.75562831582289),.UNSPECIFIED.);
#661=B_SPLINE_CURVE_WITH_KNOTS('',3,(#38860,#38861,#38862,#38863,#38864,
#38865),.UNSPECIFIED.,.F.,.F.,(4,2,4),(0.436494357616821,0.49057908163088,
0.523269669927355),.UNSPECIFIED.);
#662=B_SPLINE_CURVE_WITH_KNOTS('',3,(#38866,#38867,#38868,#38869,#38870,
#38871,#38872,#38873,#38874,#38875,#38876,#38877,#38878,#38879,#38880,#38881,
#38882,#38883,#38884),.UNSPECIFIED.,.F.,.F.,(4,3,3,3,3,3,4),(-0.110253525235352,
-0.0702407414377446,-0.0308586443223844,0.,0.039200042191676,0.0788707706427867,
0.110060546834448),.UNSPECIFIED.);
#663=B_SPLINE_CURVE_WITH_KNOTS('',3,(#38887,#38888,#38889,#38890,#38891,
#38892),.UNSPECIFIED.,.F.,.F.,(4,2,4),(1.43904665659616,1.47173724489264,
1.5258219689067),.UNSPECIFIED.);
#664=B_SPLINE_CURVE_WITH_KNOTS('',3,(#38894,#38895,#38896,#38897,#38898,
#38899,#38900,#38901,#38902,#38903,#38904,#38905,#38906,#38907,#38908,#38909,
#38910,#38911,#38912),.UNSPECIFIED.,.F.,.F.,(4,3,3,3,3,3,4),(-1.40481265039416,
-1.36522996541145,-1.32585540726348,-1.28679683363997,-1.26015734748853,
-1.21999608757355,-1.18433882030033),.UNSPECIFIED.);
#665=B_SPLINE_CURVE_WITH_KNOTS('',3,(#38914,#38915,#38916,#38917,#38918,
#38919),.UNSPECIFIED.,.F.,.F.,(4,2,4),(1.43904665659616,1.47173724489264,
1.52582196890582),.UNSPECIFIED.);
#666=B_SPLINE_CURVE_WITH_KNOTS('',3,(#38920,#38921,#38922,#38923,#38924,
#38925,#38926,#38927,#38928,#38929,#38930,#38931,#38932,#38933,#38934,#38935,
#38936,#38937,#38938),.UNSPECIFIED.,.F.,.F.,(4,3,3,3,3,3,4),(1.21344063784118,
1.25510987200879,1.29073244309219,1.33189452838105,1.37317594357344,1.41463545273868,
1.43283480298247),.UNSPECIFIED.);
#667=B_SPLINE_CURVE_WITH_KNOTS('',3,(#38948,#38949,#38950,#38951,#38952,
#38953,#38954),.UNSPECIFIED.,.F.,.F.,(4,3,4),(1.98904556960248,2.09488046175532,
2.20071535390815),.UNSPECIFIED.);
#668=B_SPLINE_CURVE_WITH_KNOTS('',3,(#38958,#38959,#38960,#38961,#38962,
#38963,#38964),.UNSPECIFIED.,.F.,.F.,(4,3,4),(-0.105611957753098,0.,0.105611957753098),
 .UNSPECIFIED.);
#669=B_SPLINE_CURVE_WITH_KNOTS('',3,(#38969,#38970,#38971,#38972,#38973,
#38974),.UNSPECIFIED.,.F.,.F.,(4,2,4),(-1.17106027221854,-1.06544831446544,
-0.959836356712345),.UNSPECIFIED.);
#670=B_SPLINE_CURVE_WITH_KNOTS('',3,(#38977,#38978,#38979,#38980,#38981,
#38982),.UNSPECIFIED.,.F.,.F.,(4,2,4),(0.941605338724826,1.04744023087766,
1.15327512303049),.UNSPECIFIED.);
#671=B_SPLINE_CURVE_WITH_KNOTS('',3,(#38995,#38996,#38997,#38998,#38999,
#39000,#39001,#39002,#39003,#39004,#39005,#39006,#39007,#39008,#39009,#39010,
#39011,#39012,#39013),.UNSPECIFIED.,.F.,.F.,(4,3,3,3,3,3,4),(2.47883976068978,
2.51859129056809,2.55786629068885,2.58890030752247,2.62818560996811,2.66809093310445,
2.69915383275782),.UNSPECIFIED.);
#672=B_SPLINE_CURVE_WITH_KNOTS('',3,(#39015,#39016,#39017,#39018,#39019,
#39020),.UNSPECIFIED.,.F.,.F.,(4,2,4),(-0.523250481795672,-0.490578640084517,
-0.436484426249653),.UNSPECIFIED.);
#673=B_SPLINE_CURVE_WITH_KNOTS('',3,(#39022,#39023,#39024,#39025,#39026,
#39027,#39028,#39029,#39030,#39031,#39032,#39033,#39034,#39035,#39036,#39037,
#39038,#39039,#39040),.UNSPECIFIED.,.F.,.F.,(4,3,3,3,3,3,4),(-0.109726413656553,
-0.0680893754924848,-0.0267736956128723,0.,0.0412006233150074,0.082597721206199,
0.109572523074534),.UNSPECIFIED.);
#674=B_SPLINE_CURVE_WITH_KNOTS('',3,(#39041,#39042,#39043,#39044,#39045,
#39046),.UNSPECIFIED.,.F.,.F.,(4,2,4),(-0.523250481795879,-0.490578640084517,
-0.43648442624966),.UNSPECIFIED.);
#675=B_SPLINE_CURVE_WITH_KNOTS('',3,(#39049,#39050,#39051,#39052,#39053,
#39054),.UNSPECIFIED.,.F.,.F.,(4,2,4),(1.43904665659616,1.47173724489264,
1.5258219689067),.UNSPECIFIED.);
#676=B_SPLINE_CURVE_WITH_KNOTS('',3,(#39056,#39057,#39058,#39059,#39060,
#39061,#39062,#39063,#39064,#39065,#39066,#39067,#39068,#39069,#39070,#39071,
#39072,#39073,#39074),.UNSPECIFIED.,.F.,.F.,(4,3,3,3,3,3,4),(-1.40481265039414,
-1.36522996541144,-1.32585540726348,-1.28679683363997,-1.26015734748851,
-1.21999608757358,-1.18433882030032),.UNSPECIFIED.);
#677=B_SPLINE_CURVE_WITH_KNOTS('',3,(#39076,#39077,#39078,#39079,#39080,
#39081),.UNSPECIFIED.,.F.,.F.,(4,2,4),(1.43904665659617,1.47173724489264,
1.52582196890583),.UNSPECIFIED.);
#678=B_SPLINE_CURVE_WITH_KNOTS('',3,(#39082,#39083,#39084,#39085,#39086,
#39087,#39088,#39089,#39090,#39091,#39092,#39093,#39094,#39095,#39096,#39097,
#39098,#39099,#39100),.UNSPECIFIED.,.F.,.F.,(4,3,3,3,3,3,4),(1.21344063784118,
1.25510987200878,1.29073244309219,1.33189452838105,1.37317594357344,1.41463545273868,
1.43283480298247),.UNSPECIFIED.);
#679=B_SPLINE_CURVE_WITH_KNOTS('',3,(#39106,#39107,#39108,#39109,#39110,
#39111),.UNSPECIFIED.,.F.,.F.,(4,2,4),(0.959836356712344,1.06544831446544,
1.17106027221854),.UNSPECIFIED.);
#680=B_SPLINE_CURVE_WITH_KNOTS('',3,(#39115,#39116,#39117,#39118,#39119,
#39120),.UNSPECIFIED.,.F.,.F.,(4,2,4),(-1.15327512303049,-1.04744023087766,
-0.941605338724826),.UNSPECIFIED.);
#681=B_SPLINE_CURVE_WITH_KNOTS('',3,(#39127,#39128,#39129,#39130,#39131,
#39132,#39133),.UNSPECIFIED.,.F.,.F.,(4,3,4),(1.98904556960249,2.09488046175532,
2.20071535390815),.UNSPECIFIED.);
#682=B_SPLINE_CURVE_WITH_KNOTS('',3,(#39137,#39138,#39139,#39140,#39141,
#39142,#39143),.UNSPECIFIED.,.F.,.F.,(4,3,4),(-0.105611957753097,0.,0.105611957753097),
 .UNSPECIFIED.);
#683=B_SPLINE_CURVE_WITH_KNOTS('',3,(#39158,#39159,#39160,#39161,#39162,
#39163,#39164),.UNSPECIFIED.,.F.,.F.,(4,3,4),(1.98904556960249,2.09488046175532,
2.20071535390815),.UNSPECIFIED.);
#684=B_SPLINE_CURVE_WITH_KNOTS('',3,(#39168,#39169,#39170,#39171,#39172,
#39173,#39174),.UNSPECIFIED.,.F.,.F.,(4,3,4),(-0.105611957753096,0.,0.105611957753097),
 .UNSPECIFIED.);
#685=B_SPLINE_CURVE_WITH_KNOTS('',3,(#39179,#39180,#39181,#39182,#39183,
#39184),.UNSPECIFIED.,.F.,.F.,(4,2,4),(-1.17106027221854,-1.06544831446544,
-0.959836356712344),.UNSPECIFIED.);
#686=B_SPLINE_CURVE_WITH_KNOTS('',3,(#39187,#39188,#39189,#39190,#39191,
#39192),.UNSPECIFIED.,.F.,.F.,(4,2,4),(0.941605338724827,1.04744023087766,
1.15327512303049),.UNSPECIFIED.);
#687=B_SPLINE_CURVE_WITH_KNOTS('',3,(#39205,#39206,#39207,#39208,#39209,
#39210),.UNSPECIFIED.,.F.,.F.,(4,2,4),(0.43648442624966,0.490578640084517,
0.523250481795913),.UNSPECIFIED.);
#688=B_SPLINE_CURVE_WITH_KNOTS('',3,(#39212,#39213,#39214,#39215,#39216,
#39217,#39218,#39219,#39220,#39221,#39222,#39223,#39224,#39225,#39226,#39227,
#39228,#39229,#39230),.UNSPECIFIED.,.F.,.F.,(4,3,3,3,3,3,4),(1.21344063784115,
1.25510987200874,1.29073244309218,1.33189452838104,1.37317594357343,1.41463545273866,
1.43283480298248),.UNSPECIFIED.);
#689=B_SPLINE_CURVE_WITH_KNOTS('',3,(#39232,#39233,#39234,#39235,#39236,
#39237),.UNSPECIFIED.,.F.,.F.,(4,2,4),(0.436494357616825,0.49057908163088,
0.523269669927497),.UNSPECIFIED.);
#690=B_SPLINE_CURVE_WITH_KNOTS('',3,(#39238,#39239,#39240,#39241,#39242,
#39243,#39244,#39245,#39246,#39247,#39248,#39249,#39250,#39251,#39252,#39253,
#39254,#39255,#39256),.UNSPECIFIED.,.F.,.F.,(4,3,3,3,3,3,4),(-1.40481265039423,
-1.36522996541152,-1.32585540726357,-1.28679683364005,-1.26015734748857,
-1.2199960875736,-1.18433882030035),.UNSPECIFIED.);
#691=B_SPLINE_CURVE_WITH_KNOTS('',3,(#39259,#39260,#39261,#39262,#39263,
#39264),.UNSPECIFIED.,.F.,.F.,(4,2,4),(1.43906407854219,1.47173592025355,
1.52583013408841),.UNSPECIFIED.);
#692=B_SPLINE_CURVE_WITH_KNOTS('',3,(#39266,#39267,#39268,#39269,#39270,
#39271,#39272,#39273,#39274,#39275,#39276,#39277,#39278,#39279,#39280,#39281,
#39282,#39283,#39284),.UNSPECIFIED.,.F.,.F.,(4,3,3,3,3,3,4),(-0.110253525235352,
-0.0702407414376601,-0.030858644322292,0.,0.0392000421916706,0.0788707706427867,
0.110060546834447),.UNSPECIFIED.);
#693=B_SPLINE_CURVE_WITH_KNOTS('',3,(#39286,#39287,#39288,#39289,#39290,
#39291),.UNSPECIFIED.,.F.,.F.,(4,2,4),(1.43906407854219,1.47173592025355,
1.52583013408754),.UNSPECIFIED.);
#694=B_SPLINE_CURVE_WITH_KNOTS('',3,(#39292,#39293,#39294,#39295,#39296,
#39297,#39298,#39299,#39300,#39301,#39302,#39303,#39304,#39305,#39306,#39307,
#39308,#39309,#39310),.UNSPECIFIED.,.F.,.F.,(4,3,3,3,3,3,4),(2.53632937909179,
2.57775416224768,2.61898206719531,2.64590190216631,2.68717408326042,2.72876559667485,
2.75562831582286),.UNSPECIFIED.);
#695=B_SPLINE_CURVE_WITH_KNOTS('',3,(#39598,#39599,#39600,#39601,#39602,
#39603),.UNSPECIFIED.,.F.,.F.,(4,2,4),(0.436494357616827,0.49057908163088,
0.523269669927392),.UNSPECIFIED.);
#696=B_SPLINE_CURVE_WITH_KNOTS('',3,(#39605,#39606,#39607,#39608,#39609,
#39610,#39611,#39612,#39613,#39614,#39615,#39616,#39617,#39618,#39619,#39620,
#39621,#39622,#39623),.UNSPECIFIED.,.F.,.F.,(4,3,3,3,3,3,4),(1.21344063784114,
1.25510987200879,1.29073244309217,1.33189452838103,1.37317594357341,1.41463545273866,
1.43283480298246),.UNSPECIFIED.);
#697=B_SPLINE_CURVE_WITH_KNOTS('',3,(#39625,#39626,#39627,#39628,#39629,
#39630),.UNSPECIFIED.,.F.,.F.,(4,2,4),(0.436494357616828,0.49057908163088,
0.523269669927516),.UNSPECIFIED.);
#698=B_SPLINE_CURVE_WITH_KNOTS('',3,(#39631,#39632,#39633,#39634,#39635,
#39636,#39637,#39638,#39639,#39640,#39641,#39642,#39643,#39644,#39645,#39646,
#39647,#39648,#39649),.UNSPECIFIED.,.F.,.F.,(4,3,3,3,3,3,4),(-1.40481265039417,
-1.36522996541144,-1.32585540726346,-1.28679683363995,-1.26015734748852,
-1.21999608757349,-1.1843388203003),.UNSPECIFIED.);
#699=B_SPLINE_CURVE_WITH_KNOTS('',3,(#39652,#39653,#39654,#39655,#39656,
#39657),.UNSPECIFIED.,.F.,.F.,(4,2,4),(1.43904665659616,1.47173724489264,
1.52582196890669),.UNSPECIFIED.);
#700=B_SPLINE_CURVE_WITH_KNOTS('',3,(#39659,#39660,#39661,#39662,#39663,
#39664,#39665,#39666,#39667,#39668,#39669,#39670,#39671,#39672,#39673,#39674,
#39675,#39676,#39677),.UNSPECIFIED.,.F.,.F.,(4,3,3,3,3,3,4),(-0.110253525235352,
-0.070240741437667,-0.0308586443223014,0.,0.0392000421916667,0.0788707706427855,
0.110060546834446),.UNSPECIFIED.);
#701=B_SPLINE_CURVE_WITH_KNOTS('',3,(#39679,#39680,#39681,#39682,#39683,
#39684),.UNSPECIFIED.,.F.,.F.,(4,2,4),(1.43904665659616,1.47173724489264,
1.52582196890582),.UNSPECIFIED.);
#702=B_SPLINE_CURVE_WITH_KNOTS('',3,(#39685,#39686,#39687,#39688,#39689,
#39690,#39691,#39692,#39693,#39694,#39695,#39696,#39697,#39698,#39699,#39700,
#39701,#39702,#39703),.UNSPECIFIED.,.F.,.F.,(4,3,3,3,3,3,4),(2.53632937909178,
2.57775416224765,2.61898206719527,2.6459019021663,2.68717408326041,2.72876559667488,
2.75562831582286),.UNSPECIFIED.);
#703=B_SPLINE_CURVE_WITH_KNOTS('',3,(#39713,#39714,#39715,#39716,#39717,
#39718,#39719),.UNSPECIFIED.,.F.,.F.,(4,3,4),(1.98904556960248,2.09488046175532,
2.20071535390815),.UNSPECIFIED.);
#704=B_SPLINE_CURVE_WITH_KNOTS('',3,(#39723,#39724,#39725,#39726,#39727,
#39728,#39729),.UNSPECIFIED.,.F.,.F.,(4,3,4),(-0.105611957753097,0.,0.105611957753097),
 .UNSPECIFIED.);
#705=B_SPLINE_CURVE_WITH_KNOTS('',3,(#39734,#39735,#39736,#39737,#39738,
#39739),.UNSPECIFIED.,.F.,.F.,(4,2,4),(-1.17106027221854,-1.06544831446544,
-0.959836356712345),.UNSPECIFIED.);
#706=B_SPLINE_CURVE_WITH_KNOTS('',3,(#39742,#39743,#39744,#39745,#39746,
#39747),.UNSPECIFIED.,.F.,.F.,(4,2,4),(0.941605338724826,1.04744023087766,
1.15327512303049),.UNSPECIFIED.);
#707=B_SPLINE_CURVE_WITH_KNOTS('',3,(#39760,#39761,#39762,#39763,#39764,
#39765),.UNSPECIFIED.,.F.,.F.,(4,2,4),(0.436494357616816,0.49057908163088,
0.523269669927352),.UNSPECIFIED.);
#708=B_SPLINE_CURVE_WITH_KNOTS('',3,(#39767,#39768,#39769,#39770,#39771,
#39772,#39773,#39774,#39775,#39776,#39777,#39778,#39779,#39780,#39781,#39782,
#39783,#39784,#39785),.UNSPECIFIED.,.F.,.F.,(4,3,3,3,3,3,4),(1.21344063784117,
1.2551098720088,1.29073244309219,1.33189452838105,1.37317594357344,1.41463545273871,
1.43283480298249),.UNSPECIFIED.);
#709=B_SPLINE_CURVE_WITH_KNOTS('',3,(#39787,#39788,#39789,#39790,#39791,
#39792),.UNSPECIFIED.,.F.,.F.,(4,2,4),(0.436484426249651,0.490578640084517,
0.523250481795878),.UNSPECIFIED.);
#710=B_SPLINE_CURVE_WITH_KNOTS('',3,(#39793,#39794,#39795,#39796,#39797,
#39798,#39799,#39800,#39801,#39802,#39803,#39804,#39805,#39806,#39807,#39808,
#39809,#39810,#39811),.UNSPECIFIED.,.F.,.F.,(4,3,3,3,3,3,4),(-1.40481265039413,
-1.36522996541145,-1.32585540726349,-1.28679683363998,-1.2601573474885,
-1.21999608757352,-1.18433882030031),.UNSPECIFIED.);
#711=B_SPLINE_CURVE_WITH_KNOTS('',3,(#39814,#39815,#39816,#39817,#39818,
#39819),.UNSPECIFIED.,.F.,.F.,(4,2,4),(1.43906407854219,1.47173592025355,
1.52583013408841),.UNSPECIFIED.);
#712=B_SPLINE_CURVE_WITH_KNOTS('',3,(#39821,#39822,#39823,#39824,#39825,
#39826,#39827,#39828,#39829,#39830,#39831,#39832,#39833,#39834,#39835,#39836,
#39837,#39838,#39839),.UNSPECIFIED.,.F.,.F.,(4,3,3,3,3,3,4),(-0.110253525235351,
-0.0702407414376934,-0.0308586443223274,0.,0.0392000421916682,0.0788707706427895,
0.110060546834446),.UNSPECIFIED.);
#713=B_SPLINE_CURVE_WITH_KNOTS('',3,(#39841,#39842,#39843,#39844,#39845,
#39846),.UNSPECIFIED.,.F.,.F.,(4,2,4),(1.43906407854219,1.47173592025355,
1.52583013408754),.UNSPECIFIED.);
#714=B_SPLINE_CURVE_WITH_KNOTS('',3,(#39847,#39848,#39849,#39850,#39851,
#39852,#39853,#39854,#39855,#39856,#39857,#39858,#39859,#39860,#39861,#39862,
#39863,#39864,#39865),.UNSPECIFIED.,.F.,.F.,(4,3,3,3,3,3,4),(2.53632937909181,
2.57775416224765,2.61898206719527,2.64590190216633,2.68717408326044,2.72876559667489,
2.75562831582288),.UNSPECIFIED.);
#715=B_SPLINE_CURVE_WITH_KNOTS('',3,(#39875,#39876,#39877,#39878,#39879,
#39880,#39881),.UNSPECIFIED.,.F.,.F.,(4,3,4),(1.98904556960249,2.09488046175532,
2.20071535390816),.UNSPECIFIED.);
#716=B_SPLINE_CURVE_WITH_KNOTS('',3,(#39885,#39886,#39887,#39888,#39889,
#39890,#39891),.UNSPECIFIED.,.F.,.F.,(4,3,4),(-0.105611957753097,0.,0.105611957753097),
 .UNSPECIFIED.);
#717=B_SPLINE_CURVE_WITH_KNOTS('',3,(#39896,#39897,#39898,#39899,#39900,
#39901),.UNSPECIFIED.,.F.,.F.,(4,2,4),(-1.17106027221854,-1.06544831446544,
-0.959836356712344),.UNSPECIFIED.);
#718=B_SPLINE_CURVE_WITH_KNOTS('',3,(#39904,#39905,#39906,#39907,#39908,
#39909),.UNSPECIFIED.,.F.,.F.,(4,2,4),(0.941605338724829,1.04744023087766,
1.15327512303049),.UNSPECIFIED.);
#719=B_SPLINE_CURVE_WITH_KNOTS('',3,(#39922,#39923,#39924,#39925,#39926,
#39927),.UNSPECIFIED.,.F.,.F.,(4,2,4),(0.436484426249655,0.490578640084517,
0.523250481795882),.UNSPECIFIED.);
#720=B_SPLINE_CURVE_WITH_KNOTS('',3,(#39929,#39930,#39931,#39932,#39933,
#39934,#39935,#39936,#39937,#39938,#39939,#39940,#39941,#39942,#39943,#39944,
#39945,#39946,#39947),.UNSPECIFIED.,.F.,.F.,(4,3,3,3,3,3,4),(2.53632937909178,
2.57775416224762,2.61898206719525,2.64590190216632,2.68717408326042,2.72876559667488,
2.75562831582289),.UNSPECIFIED.);
#721=B_SPLINE_CURVE_WITH_KNOTS('',3,(#39949,#39950,#39951,#39952,#39953,
#39954),.UNSPECIFIED.,.F.,.F.,(4,2,4),(0.436494357616821,0.49057908163088,
0.523269669927365),.UNSPECIFIED.);
#722=B_SPLINE_CURVE_WITH_KNOTS('',3,(#39955,#39956,#39957,#39958,#39959,
#39960,#39961,#39962,#39963,#39964,#39965,#39966,#39967,#39968,#39969,#39970,
#39971,#39972,#39973),.UNSPECIFIED.,.F.,.F.,(4,3,3,3,3,3,4),(-0.110253525235353,
-0.0702407414376493,-0.0308586443222864,0.,0.0392000421916586,0.0788707706427754,
0.110060546834447),.UNSPECIFIED.);
#723=B_SPLINE_CURVE_WITH_KNOTS('',3,(#39976,#39977,#39978,#39979,#39980,
#39981),.UNSPECIFIED.,.F.,.F.,(4,2,4),(1.43906407854219,1.47173592025355,
1.52583013408841),.UNSPECIFIED.);
#724=B_SPLINE_CURVE_WITH_KNOTS('',3,(#39983,#39984,#39985,#39986,#39987,
#39988,#39989,#39990,#39991,#39992,#39993,#39994,#39995,#39996,#39997,#39998,
#39999,#40000,#40001),.UNSPECIFIED.,.F.,.F.,(4,3,3,3,3,3,4),(-1.40481265039415,
-1.36522996541142,-1.32585540726345,-1.28679683363994,-1.26015734748852,
-1.21999608757345,-1.18433882030032),.UNSPECIFIED.);
#725=B_SPLINE_CURVE_WITH_KNOTS('',3,(#40003,#40004,#40005,#40006,#40007,
#40008),.UNSPECIFIED.,.F.,.F.,(4,2,4),(1.43906407854219,1.47173592025355,
1.52583013408753),.UNSPECIFIED.);
#726=B_SPLINE_CURVE_WITH_KNOTS('',3,(#40009,#40010,#40011,#40012,#40013,
#40014,#40015,#40016,#40017,#40018,#40019,#40020,#40021,#40022,#40023,#40024,
#40025,#40026,#40027),.UNSPECIFIED.,.F.,.F.,(4,3,3,3,3,3,4),(1.21344063784118,
1.25510987200885,1.29073244309219,1.33189452838105,1.37317594357345,1.41463545273868,
1.43283480298247),.UNSPECIFIED.);
#727=B_SPLINE_CURVE_WITH_KNOTS('',3,(#40037,#40038,#40039,#40040,#40041,
#40042,#40043),.UNSPECIFIED.,.F.,.F.,(4,3,4),(1.98904556960249,2.09488046175532,
2.20071535390815),.UNSPECIFIED.);
#728=B_SPLINE_CURVE_WITH_KNOTS('',3,(#40047,#40048,#40049,#40050,#40051,
#40052,#40053),.UNSPECIFIED.,.F.,.F.,(4,3,4),(-0.105611957753096,0.,0.105611957753097),
 .UNSPECIFIED.);
#729=B_SPLINE_CURVE_WITH_KNOTS('',3,(#40058,#40059,#40060,#40061,#40062,
#40063),.UNSPECIFIED.,.F.,.F.,(4,2,4),(-1.17106027221854,-1.06544831446544,
-0.959836356712344),.UNSPECIFIED.);
#730=B_SPLINE_CURVE_WITH_KNOTS('',3,(#40066,#40067,#40068,#40069,#40070,
#40071),.UNSPECIFIED.,.F.,.F.,(4,2,4),(0.941605338724827,1.04744023087766,
1.15327512303049),.UNSPECIFIED.);
#731=B_SPLINE_CURVE_WITH_KNOTS('',3,(#40084,#40085,#40086,#40087,#40088,
#40089),.UNSPECIFIED.,.F.,.F.,(4,2,4),(0.436494357616822,0.49057908163088,
0.523269669927398),.UNSPECIFIED.);
#732=B_SPLINE_CURVE_WITH_KNOTS('',3,(#40091,#40092,#40093,#40094,#40095,
#40096,#40097,#40098,#40099,#40100,#40101,#40102,#40103,#40104,#40105,#40106,
#40107,#40108,#40109),.UNSPECIFIED.,.F.,.F.,(4,3,3,3,3,3,4),(2.53632937909185,
2.57775416224773,2.61898206719535,2.64590190216638,2.6871740832605,2.72876559667492,
2.75562831582295),.UNSPECIFIED.);
#733=B_SPLINE_CURVE_WITH_KNOTS('',3,(#40111,#40112,#40113,#40114,#40115,
#40116),.UNSPECIFIED.,.F.,.F.,(4,2,4),(0.436484426249657,0.490578640084517,
0.523250481796065),.UNSPECIFIED.);
#734=B_SPLINE_CURVE_WITH_KNOTS('',3,(#40117,#40118,#40119,#40120,#40121,
#40122,#40123,#40124,#40125,#40126,#40127,#40128,#40129,#40130,#40131,#40132,
#40133,#40134,#40135),.UNSPECIFIED.,.F.,.F.,(4,3,3,3,3,3,4),(-0.110253525235377,
-0.070240741437708,-0.0308586443223363,0.,0.03920004219167,0.0788707706428437,
0.110060546834472),.UNSPECIFIED.);
#735=B_SPLINE_CURVE_WITH_KNOTS('',3,(#40138,#40139,#40140,#40141,#40142,
#40143),.UNSPECIFIED.,.F.,.F.,(4,2,4),(1.43904665659616,1.47173724489264,
1.52582196890669),.UNSPECIFIED.);
#736=B_SPLINE_CURVE_WITH_KNOTS('',3,(#40145,#40146,#40147,#40148,#40149,
#40150,#40151,#40152,#40153,#40154,#40155,#40156,#40157,#40158,#40159,#40160,
#40161,#40162,#40163),.UNSPECIFIED.,.F.,.F.,(4,3,3,3,3,3,4),(-1.40481265039411,
-1.36522996541141,-1.32585540726345,-1.28679683363994,-1.26015734748849,
-1.21999608757351,-1.1843388203003),.UNSPECIFIED.);
#737=B_SPLINE_CURVE_WITH_KNOTS('',3,(#40165,#40166,#40167,#40168,#40169,
#40170),.UNSPECIFIED.,.F.,.F.,(4,2,4),(1.43904665659616,1.47173724489264,
1.52582196890583),.UNSPECIFIED.);
#738=B_SPLINE_CURVE_WITH_KNOTS('',3,(#40171,#40172,#40173,#40174,#40175,
#40176,#40177,#40178,#40179,#40180,#40181,#40182,#40183,#40184,#40185,#40186,
#40187,#40188,#40189),.UNSPECIFIED.,.F.,.F.,(4,3,3,3,3,3,4),(1.2134406378412,
1.25510987200883,1.29073244309221,1.33189452838107,1.37317594357346,1.41463545273868,
1.43283480298249),.UNSPECIFIED.);
#739=B_SPLINE_CURVE_WITH_KNOTS('',3,(#40199,#40200,#40201,#40202,#40203,
#40204,#40205),.UNSPECIFIED.,.F.,.F.,(4,3,4),(1.98904556960248,2.09488046175532,
2.20071535390815),.UNSPECIFIED.);
#740=B_SPLINE_CURVE_WITH_KNOTS('',3,(#40209,#40210,#40211,#40212,#40213,
#40214,#40215),.UNSPECIFIED.,.F.,.F.,(4,3,4),(-0.105611957753097,0.,0.105611957753097),
 .UNSPECIFIED.);
#741=B_SPLINE_CURVE_WITH_KNOTS('',3,(#40220,#40221,#40222,#40223,#40224,
#40225),.UNSPECIFIED.,.F.,.F.,(4,2,4),(-1.17106027221854,-1.06544831446544,
-0.959836356712344),.UNSPECIFIED.);
#742=B_SPLINE_CURVE_WITH_KNOTS('',3,(#40228,#40229,#40230,#40231,#40232,
#40233),.UNSPECIFIED.,.F.,.F.,(4,2,4),(0.941605338724826,1.04744023087766,
1.15327512303049),.UNSPECIFIED.);
#743=B_SPLINE_CURVE_WITH_KNOTS('',3,(#40246,#40247,#40248,#40249,#40250,
#40251),.UNSPECIFIED.,.F.,.F.,(4,2,4),(0.436494357616821,0.49057908163088,
0.523269669927355),.UNSPECIFIED.);
#744=B_SPLINE_CURVE_WITH_KNOTS('',3,(#40253,#40254,#40255,#40256,#40257,
#40258,#40259,#40260,#40261,#40262,#40263,#40264,#40265,#40266,#40267,#40268,
#40269,#40270,#40271),.UNSPECIFIED.,.F.,.F.,(4,3,3,3,3,3,4),(2.53632937909179,
2.57775416224772,2.61898206719534,2.64590190216632,2.68717408326042,2.72876559667486,
2.75562831582289),.UNSPECIFIED.);
#745=B_SPLINE_CURVE_WITH_KNOTS('',3,(#40273,#40274,#40275,#40276,#40277,
#40278),.UNSPECIFIED.,.F.,.F.,(4,2,4),(0.436494357616821,0.49057908163088,
0.523269669927355),.UNSPECIFIED.);
#746=B_SPLINE_CURVE_WITH_KNOTS('',3,(#40279,#40280,#40281,#40282,#40283,
#40284,#40285,#40286,#40287,#40288,#40289,#40290,#40291,#40292,#40293,#40294,
#40295,#40296,#40297),.UNSPECIFIED.,.F.,.F.,(4,3,3,3,3,3,4),(-0.110253525235352,
-0.0702407414377446,-0.0308586443223844,0.,0.039200042191676,0.0788707706427867,
0.110060546834448),.UNSPECIFIED.);
#747=B_SPLINE_CURVE_WITH_KNOTS('',3,(#40300,#40301,#40302,#40303,#40304,
#40305),.UNSPECIFIED.,.F.,.F.,(4,2,4),(1.43904665659616,1.47173724489264,
1.5258219689067),.UNSPECIFIED.);
#748=B_SPLINE_CURVE_WITH_KNOTS('',3,(#40307,#40308,#40309,#40310,#40311,
#40312,#40313,#40314,#40315,#40316,#40317,#40318,#40319,#40320,#40321,#40322,
#40323,#40324,#40325),.UNSPECIFIED.,.F.,.F.,(4,3,3,3,3,3,4),(-1.40481265039416,
-1.36522996541145,-1.32585540726348,-1.28679683363997,-1.26015734748853,
-1.21999608757355,-1.18433882030033),.UNSPECIFIED.);
#749=B_SPLINE_CURVE_WITH_KNOTS('',3,(#40327,#40328,#40329,#40330,#40331,
#40332),.UNSPECIFIED.,.F.,.F.,(4,2,4),(1.43904665659616,1.47173724489264,
1.52582196890582),.UNSPECIFIED.);
#750=B_SPLINE_CURVE_WITH_KNOTS('',3,(#40333,#40334,#40335,#40336,#40337,
#40338,#40339,#40340,#40341,#40342,#40343,#40344,#40345,#40346,#40347,#40348,
#40349,#40350,#40351),.UNSPECIFIED.,.F.,.F.,(4,3,3,3,3,3,4),(1.21344063784118,
1.25510987200879,1.29073244309219,1.33189452838105,1.37317594357344,1.41463545273868,
1.43283480298247),.UNSPECIFIED.);
#751=B_SPLINE_CURVE_WITH_KNOTS('',3,(#40361,#40362,#40363,#40364,#40365,
#40366,#40367),.UNSPECIFIED.,.F.,.F.,(4,3,4),(1.98904556960248,2.09488046175532,
2.20071535390815),.UNSPECIFIED.);
#752=B_SPLINE_CURVE_WITH_KNOTS('',3,(#40371,#40372,#40373,#40374,#40375,
#40376,#40377),.UNSPECIFIED.,.F.,.F.,(4,3,4),(-0.105611957753098,0.,0.105611957753098),
 .UNSPECIFIED.);
#753=B_SPLINE_CURVE_WITH_KNOTS('',3,(#40382,#40383,#40384,#40385,#40386,
#40387),.UNSPECIFIED.,.F.,.F.,(4,2,4),(-1.17106027221854,-1.06544831446544,
-0.959836356712345),.UNSPECIFIED.);
#754=B_SPLINE_CURVE_WITH_KNOTS('',3,(#40390,#40391,#40392,#40393,#40394,
#40395),.UNSPECIFIED.,.F.,.F.,(4,2,4),(0.941605338724826,1.04744023087766,
1.15327512303049),.UNSPECIFIED.);
#755=B_SPLINE_CURVE_WITH_KNOTS('',3,(#40408,#40409,#40410,#40411,#40412,
#40413,#40414,#40415,#40416,#40417,#40418,#40419,#40420,#40421,#40422,#40423,
#40424,#40425,#40426),.UNSPECIFIED.,.F.,.F.,(4,3,3,3,3,3,4),(2.47883976068978,
2.51859129056809,2.55786629068885,2.58890030752247,2.62818560996811,2.66809093310445,
2.69915383275782),.UNSPECIFIED.);
#756=B_SPLINE_CURVE_WITH_KNOTS('',3,(#40428,#40429,#40430,#40431,#40432,
#40433),.UNSPECIFIED.,.F.,.F.,(4,2,4),(-0.523250481795672,-0.490578640084517,
-0.436484426249653),.UNSPECIFIED.);
#757=B_SPLINE_CURVE_WITH_KNOTS('',3,(#40435,#40436,#40437,#40438,#40439,
#40440,#40441,#40442,#40443,#40444,#40445,#40446,#40447,#40448,#40449,#40450,
#40451,#40452,#40453),.UNSPECIFIED.,.F.,.F.,(4,3,3,3,3,3,4),(-0.109726413656553,
-0.0680893754924848,-0.0267736956128723,0.,0.0412006233150074,0.082597721206199,
0.109572523074534),.UNSPECIFIED.);
#758=B_SPLINE_CURVE_WITH_KNOTS('',3,(#40454,#40455,#40456,#40457,#40458,
#40459),.UNSPECIFIED.,.F.,.F.,(4,2,4),(-0.523250481795879,-0.490578640084517,
-0.43648442624966),.UNSPECIFIED.);
#759=B_SPLINE_CURVE_WITH_KNOTS('',3,(#40462,#40463,#40464,#40465,#40466,
#40467),.UNSPECIFIED.,.F.,.F.,(4,2,4),(1.43904665659616,1.47173724489264,
1.5258219689067),.UNSPECIFIED.);
#760=B_SPLINE_CURVE_WITH_KNOTS('',3,(#40469,#40470,#40471,#40472,#40473,
#40474,#40475,#40476,#40477,#40478,#40479,#40480,#40481,#40482,#40483,#40484,
#40485,#40486,#40487),.UNSPECIFIED.,.F.,.F.,(4,3,3,3,3,3,4),(-1.40481265039414,
-1.36522996541144,-1.32585540726348,-1.28679683363997,-1.26015734748851,
-1.21999608757358,-1.18433882030032),.UNSPECIFIED.);
#761=B_SPLINE_CURVE_WITH_KNOTS('',3,(#40489,#40490,#40491,#40492,#40493,
#40494),.UNSPECIFIED.,.F.,.F.,(4,2,4),(1.43904665659617,1.47173724489264,
1.52582196890583),.UNSPECIFIED.);
#762=B_SPLINE_CURVE_WITH_KNOTS('',3,(#40495,#40496,#40497,#40498,#40499,
#40500,#40501,#40502,#40503,#40504,#40505,#40506,#40507,#40508,#40509,#40510,
#40511,#40512,#40513),.UNSPECIFIED.,.F.,.F.,(4,3,3,3,3,3,4),(1.21344063784118,
1.25510987200878,1.29073244309219,1.33189452838105,1.37317594357344,1.41463545273868,
1.43283480298247),.UNSPECIFIED.);
#763=B_SPLINE_CURVE_WITH_KNOTS('',3,(#40519,#40520,#40521,#40522,#40523,
#40524),.UNSPECIFIED.,.F.,.F.,(4,2,4),(0.959836356712344,1.06544831446544,
1.17106027221854),.UNSPECIFIED.);
#764=B_SPLINE_CURVE_WITH_KNOTS('',3,(#40528,#40529,#40530,#40531,#40532,
#40533),.UNSPECIFIED.,.F.,.F.,(4,2,4),(-1.15327512303049,-1.04744023087766,
-0.941605338724826),.UNSPECIFIED.);
#765=B_SPLINE_CURVE_WITH_KNOTS('',3,(#40540,#40541,#40542,#40543,#40544,
#40545,#40546),.UNSPECIFIED.,.F.,.F.,(4,3,4),(1.98904556960249,2.09488046175532,
2.20071535390815),.UNSPECIFIED.);
#766=B_SPLINE_CURVE_WITH_KNOTS('',3,(#40550,#40551,#40552,#40553,#40554,
#40555,#40556),.UNSPECIFIED.,.F.,.F.,(4,3,4),(-0.105611957753097,0.,0.105611957753097),
 .UNSPECIFIED.);
#767=B_SPLINE_CURVE_WITH_KNOTS('',3,(#40571,#40572,#40573,#40574,#40575,
#40576,#40577),.UNSPECIFIED.,.F.,.F.,(4,3,4),(1.98904556960249,2.09488046175532,
2.20071535390815),.UNSPECIFIED.);
#768=B_SPLINE_CURVE_WITH_KNOTS('',3,(#40581,#40582,#40583,#40584,#40585,
#40586,#40587),.UNSPECIFIED.,.F.,.F.,(4,3,4),(-0.105611957753096,0.,0.105611957753097),
 .UNSPECIFIED.);
#769=B_SPLINE_CURVE_WITH_KNOTS('',3,(#40592,#40593,#40594,#40595,#40596,
#40597),.UNSPECIFIED.,.F.,.F.,(4,2,4),(-1.17106027221854,-1.06544831446544,
-0.959836356712344),.UNSPECIFIED.);
#770=B_SPLINE_CURVE_WITH_KNOTS('',3,(#40600,#40601,#40602,#40603,#40604,
#40605),.UNSPECIFIED.,.F.,.F.,(4,2,4),(0.941605338724827,1.04744023087766,
1.15327512303049),.UNSPECIFIED.);
#771=B_SPLINE_CURVE_WITH_KNOTS('',3,(#40618,#40619,#40620,#40621,#40622,
#40623),.UNSPECIFIED.,.F.,.F.,(4,2,4),(0.43648442624966,0.490578640084517,
0.523250481795913),.UNSPECIFIED.);
#772=B_SPLINE_CURVE_WITH_KNOTS('',3,(#40625,#40626,#40627,#40628,#40629,
#40630,#40631,#40632,#40633,#40634,#40635,#40636,#40637,#40638,#40639,#40640,
#40641,#40642,#40643),.UNSPECIFIED.,.F.,.F.,(4,3,3,3,3,3,4),(1.21344063784115,
1.25510987200874,1.29073244309218,1.33189452838104,1.37317594357343,1.41463545273866,
1.43283480298248),.UNSPECIFIED.);
#773=B_SPLINE_CURVE_WITH_KNOTS('',3,(#40645,#40646,#40647,#40648,#40649,
#40650),.UNSPECIFIED.,.F.,.F.,(4,2,4),(0.436494357616825,0.49057908163088,
0.523269669927497),.UNSPECIFIED.);
#774=B_SPLINE_CURVE_WITH_KNOTS('',3,(#40651,#40652,#40653,#40654,#40655,
#40656,#40657,#40658,#40659,#40660,#40661,#40662,#40663,#40664,#40665,#40666,
#40667,#40668,#40669),.UNSPECIFIED.,.F.,.F.,(4,3,3,3,3,3,4),(-1.40481265039423,
-1.36522996541152,-1.32585540726357,-1.28679683364005,-1.26015734748857,
-1.2199960875736,-1.18433882030035),.UNSPECIFIED.);
#775=B_SPLINE_CURVE_WITH_KNOTS('',3,(#40672,#40673,#40674,#40675,#40676,
#40677),.UNSPECIFIED.,.F.,.F.,(4,2,4),(1.43906407854219,1.47173592025355,
1.52583013408841),.UNSPECIFIED.);
#776=B_SPLINE_CURVE_WITH_KNOTS('',3,(#40679,#40680,#40681,#40682,#40683,
#40684,#40685,#40686,#40687,#40688,#40689,#40690,#40691,#40692,#40693,#40694,
#40695,#40696,#40697),.UNSPECIFIED.,.F.,.F.,(4,3,3,3,3,3,4),(-0.110253525235352,
-0.0702407414376601,-0.030858644322292,0.,0.0392000421916706,0.0788707706427867,
0.110060546834447),.UNSPECIFIED.);
#777=B_SPLINE_CURVE_WITH_KNOTS('',3,(#40699,#40700,#40701,#40702,#40703,
#40704),.UNSPECIFIED.,.F.,.F.,(4,2,4),(1.43906407854219,1.47173592025355,
1.52583013408754),.UNSPECIFIED.);
#778=B_SPLINE_CURVE_WITH_KNOTS('',3,(#40705,#40706,#40707,#40708,#40709,
#40710,#40711,#40712,#40713,#40714,#40715,#40716,#40717,#40718,#40719,#40720,
#40721,#40722,#40723),.UNSPECIFIED.,.F.,.F.,(4,3,3,3,3,3,4),(2.53632937909179,
2.57775416224768,2.61898206719531,2.64590190216631,2.68717408326042,2.72876559667485,
2.75562831582286),.UNSPECIFIED.);
#779=B_SPLINE_CURVE_WITH_KNOTS('',3,(#41011,#41012,#41013,#41014,#41015,
#41016),.UNSPECIFIED.,.F.,.F.,(4,2,4),(0.436494357616827,0.49057908163088,
0.523269669927392),.UNSPECIFIED.);
#780=B_SPLINE_CURVE_WITH_KNOTS('',3,(#41018,#41019,#41020,#41021,#41022,
#41023,#41024,#41025,#41026,#41027,#41028,#41029,#41030,#41031,#41032,#41033,
#41034,#41035,#41036),.UNSPECIFIED.,.F.,.F.,(4,3,3,3,3,3,4),(-1.40481265039417,
-1.36522996541144,-1.32585540726346,-1.28679683363995,-1.26015734748852,
-1.21999608757349,-1.1843388203003),.UNSPECIFIED.);
#781=B_SPLINE_CURVE_WITH_KNOTS('',3,(#41038,#41039,#41040,#41041,#41042,
#41043),.UNSPECIFIED.,.F.,.F.,(4,2,4),(0.436494357616828,0.49057908163088,
0.523269669927516),.UNSPECIFIED.);
#782=B_SPLINE_CURVE_WITH_KNOTS('',3,(#41044,#41045,#41046,#41047,#41048,
#41049,#41050,#41051,#41052,#41053,#41054,#41055,#41056,#41057,#41058,#41059,
#41060,#41061,#41062),.UNSPECIFIED.,.F.,.F.,(4,3,3,3,3,3,4),(1.21344063784114,
1.25510987200879,1.29073244309217,1.33189452838103,1.37317594357341,1.41463545273866,
1.43283480298246),.UNSPECIFIED.);
#783=B_SPLINE_CURVE_WITH_KNOTS('',3,(#41065,#41066,#41067,#41068,#41069,
#41070),.UNSPECIFIED.,.F.,.F.,(4,2,4),(1.43904665659616,1.47173724489264,
1.52582196890669),.UNSPECIFIED.);
#784=B_SPLINE_CURVE_WITH_KNOTS('',3,(#41072,#41073,#41074,#41075,#41076,
#41077,#41078,#41079,#41080,#41081,#41082,#41083,#41084,#41085,#41086,#41087,
#41088,#41089,#41090),.UNSPECIFIED.,.F.,.F.,(4,3,3,3,3,3,4),(2.53632937909178,
2.57775416224765,2.61898206719527,2.6459019021663,2.68717408326041,2.72876559667488,
2.75562831582286),.UNSPECIFIED.);
#785=B_SPLINE_CURVE_WITH_KNOTS('',3,(#41092,#41093,#41094,#41095,#41096,
#41097),.UNSPECIFIED.,.F.,.F.,(4,2,4),(1.43904665659616,1.47173724489264,
1.52582196890582),.UNSPECIFIED.);
#786=B_SPLINE_CURVE_WITH_KNOTS('',3,(#41098,#41099,#41100,#41101,#41102,
#41103,#41104,#41105,#41106,#41107,#41108,#41109,#41110,#41111,#41112,#41113,
#41114,#41115,#41116),.UNSPECIFIED.,.F.,.F.,(4,3,3,3,3,3,4),(-0.110253525235352,
-0.070240741437667,-0.0308586443223014,0.,0.0392000421916667,0.0788707706427855,
0.110060546834446),.UNSPECIFIED.);
#787=B_SPLINE_CURVE_WITH_KNOTS('',3,(#41122,#41123,#41124,#41125,#41126,
#41127),.UNSPECIFIED.,.F.,.F.,(4,2,4),(-1.15327512303049,-1.04744023087766,
-0.941605338724827),.UNSPECIFIED.);
#788=B_SPLINE_CURVE_WITH_KNOTS('',3,(#41131,#41132,#41133,#41134,#41135,
#41136),.UNSPECIFIED.,.F.,.F.,(4,2,4),(0.959836356712345,1.06544831446544,
1.17106027221854),.UNSPECIFIED.);
#789=B_SPLINE_CURVE_WITH_KNOTS('',3,(#41143,#41144,#41145,#41146,#41147,
#41148,#41149),.UNSPECIFIED.,.F.,.F.,(4,3,4),(2.02528467117779,2.13089662893088,
2.23650858668398),.UNSPECIFIED.);
#790=B_SPLINE_CURVE_WITH_KNOTS('',3,(#41153,#41154,#41155,#41156,#41157,
#41158,#41159),.UNSPECIFIED.,.F.,.F.,(4,3,4),(-0.105834892152833,0.,0.105834892152833),
 .UNSPECIFIED.);
#791=B_SPLINE_CURVE_WITH_KNOTS('',3,(#41173,#41174,#41175,#41176,#41177,
#41178),.UNSPECIFIED.,.F.,.F.,(4,2,4),(0.436494357616816,0.49057908163088,
0.523269669927352),.UNSPECIFIED.);
#792=B_SPLINE_CURVE_WITH_KNOTS('',3,(#41180,#41181,#41182,#41183,#41184,
#41185,#41186,#41187,#41188,#41189,#41190,#41191,#41192,#41193,#41194,#41195,
#41196,#41197,#41198),.UNSPECIFIED.,.F.,.F.,(4,3,3,3,3,3,4),(-1.40481265039413,
-1.36522996541145,-1.32585540726349,-1.28679683363998,-1.2601573474885,
-1.21999608757352,-1.18433882030031),.UNSPECIFIED.);
#793=B_SPLINE_CURVE_WITH_KNOTS('',3,(#41200,#41201,#41202,#41203,#41204,
#41205),.UNSPECIFIED.,.F.,.F.,(4,2,4),(0.436484426249651,0.490578640084517,
0.523250481795878),.UNSPECIFIED.);
#794=B_SPLINE_CURVE_WITH_KNOTS('',3,(#41206,#41207,#41208,#41209,#41210,
#41211,#41212,#41213,#41214,#41215,#41216,#41217,#41218,#41219,#41220,#41221,
#41222,#41223,#41224),.UNSPECIFIED.,.F.,.F.,(4,3,3,3,3,3,4),(1.21344063784117,
1.2551098720088,1.29073244309219,1.33189452838105,1.37317594357344,1.41463545273871,
1.43283480298249),.UNSPECIFIED.);
#795=B_SPLINE_CURVE_WITH_KNOTS('',3,(#41227,#41228,#41229,#41230,#41231,
#41232),.UNSPECIFIED.,.F.,.F.,(4,2,4),(1.43906407854219,1.47173592025355,
1.52583013408841),.UNSPECIFIED.);
#796=B_SPLINE_CURVE_WITH_KNOTS('',3,(#41234,#41235,#41236,#41237,#41238,
#41239,#41240,#41241,#41242,#41243,#41244,#41245,#41246,#41247,#41248,#41249,
#41250,#41251,#41252),.UNSPECIFIED.,.F.,.F.,(4,3,3,3,3,3,4),(2.53632937909181,
2.57775416224765,2.61898206719527,2.64590190216633,2.68717408326044,2.72876559667489,
2.75562831582288),.UNSPECIFIED.);
#797=B_SPLINE_CURVE_WITH_KNOTS('',3,(#41254,#41255,#41256,#41257,#41258,
#41259),.UNSPECIFIED.,.F.,.F.,(4,2,4),(1.43906407854219,1.47173592025355,
1.52583013408754),.UNSPECIFIED.);
#798=B_SPLINE_CURVE_WITH_KNOTS('',3,(#41260,#41261,#41262,#41263,#41264,
#41265,#41266,#41267,#41268,#41269,#41270,#41271,#41272,#41273,#41274,#41275,
#41276,#41277,#41278),.UNSPECIFIED.,.F.,.F.,(4,3,3,3,3,3,4),(-0.110253525235351,
-0.0702407414376934,-0.0308586443223274,0.,0.0392000421916682,0.0788707706427895,
0.110060546834446),.UNSPECIFIED.);
#799=B_SPLINE_CURVE_WITH_KNOTS('',3,(#41284,#41285,#41286,#41287,#41288,
#41289),.UNSPECIFIED.,.F.,.F.,(4,2,4),(-1.15327512303049,-1.04744023087766,
-0.941605338724829),.UNSPECIFIED.);
#800=B_SPLINE_CURVE_WITH_KNOTS('',3,(#41293,#41294,#41295,#41296,#41297,
#41298),.UNSPECIFIED.,.F.,.F.,(4,2,4),(0.959836356712343,1.06544831446544,
1.17106027221854),.UNSPECIFIED.);
#801=B_SPLINE_CURVE_WITH_KNOTS('',3,(#41305,#41306,#41307,#41308,#41309,
#41310,#41311),.UNSPECIFIED.,.F.,.F.,(4,3,4),(2.02528467117778,2.13089662893088,
2.23650858668398),.UNSPECIFIED.);
#802=B_SPLINE_CURVE_WITH_KNOTS('',3,(#41315,#41316,#41317,#41318,#41319,
#41320,#41321),.UNSPECIFIED.,.F.,.F.,(4,3,4),(-0.105834892152834,0.,0.105834892152833),
 .UNSPECIFIED.);
#803=B_SPLINE_CURVE_WITH_KNOTS('',3,(#41335,#41336,#41337,#41338,#41339,
#41340),.UNSPECIFIED.,.F.,.F.,(4,2,4),(0.436484426249655,0.490578640084517,
0.523250481795882),.UNSPECIFIED.);
#804=B_SPLINE_CURVE_WITH_KNOTS('',3,(#41342,#41343,#41344,#41345,#41346,
#41347,#41348,#41349,#41350,#41351,#41352,#41353,#41354,#41355,#41356,#41357,
#41358,#41359,#41360),.UNSPECIFIED.,.F.,.F.,(4,3,3,3,3,3,4),(-0.110253525235353,
-0.0702407414376493,-0.0308586443222864,0.,0.0392000421916586,0.0788707706427754,
0.110060546834447),.UNSPECIFIED.);
#805=B_SPLINE_CURVE_WITH_KNOTS('',3,(#41362,#41363,#41364,#41365,#41366,
#41367),.UNSPECIFIED.,.F.,.F.,(4,2,4),(0.436494357616821,0.49057908163088,
0.523269669927365),.UNSPECIFIED.);
#806=B_SPLINE_CURVE_WITH_KNOTS('',3,(#41368,#41369,#41370,#41371,#41372,
#41373,#41374,#41375,#41376,#41377,#41378,#41379,#41380,#41381,#41382,#41383,
#41384,#41385,#41386),.UNSPECIFIED.,.F.,.F.,(4,3,3,3,3,3,4),(2.53632937909178,
2.57775416224762,2.61898206719525,2.64590190216632,2.68717408326042,2.72876559667488,
2.75562831582289),.UNSPECIFIED.);
#807=B_SPLINE_CURVE_WITH_KNOTS('',3,(#41389,#41390,#41391,#41392,#41393,
#41394),.UNSPECIFIED.,.F.,.F.,(4,2,4),(1.43906407854219,1.47173592025355,
1.52583013408841),.UNSPECIFIED.);
#808=B_SPLINE_CURVE_WITH_KNOTS('',3,(#41396,#41397,#41398,#41399,#41400,
#41401,#41402,#41403,#41404,#41405,#41406,#41407,#41408,#41409,#41410,#41411,
#41412,#41413,#41414),.UNSPECIFIED.,.F.,.F.,(4,3,3,3,3,3,4),(1.21344063784118,
1.25510987200885,1.29073244309219,1.33189452838105,1.37317594357345,1.41463545273868,
1.43283480298247),.UNSPECIFIED.);
#809=B_SPLINE_CURVE_WITH_KNOTS('',3,(#41416,#41417,#41418,#41419,#41420,
#41421),.UNSPECIFIED.,.F.,.F.,(4,2,4),(1.43906407854219,1.47173592025355,
1.52583013408753),.UNSPECIFIED.);
#810=B_SPLINE_CURVE_WITH_KNOTS('',3,(#41422,#41423,#41424,#41425,#41426,
#41427,#41428,#41429,#41430,#41431,#41432,#41433,#41434,#41435,#41436,#41437,
#41438,#41439,#41440),.UNSPECIFIED.,.F.,.F.,(4,3,3,3,3,3,4),(-1.40481265039415,
-1.36522996541142,-1.32585540726345,-1.28679683363994,-1.26015734748852,
-1.21999608757345,-1.18433882030032),.UNSPECIFIED.);
#811=B_SPLINE_CURVE_WITH_KNOTS('',3,(#41446,#41447,#41448,#41449,#41450,
#41451),.UNSPECIFIED.,.F.,.F.,(4,2,4),(-1.15327512303049,-1.04744023087766,
-0.941605338724827),.UNSPECIFIED.);
#812=B_SPLINE_CURVE_WITH_KNOTS('',3,(#41455,#41456,#41457,#41458,#41459,
#41460),.UNSPECIFIED.,.F.,.F.,(4,2,4),(0.959836356712344,1.06544831446544,
1.17106027221854),.UNSPECIFIED.);
#813=B_SPLINE_CURVE_WITH_KNOTS('',3,(#41467,#41468,#41469,#41470,#41471,
#41472,#41473),.UNSPECIFIED.,.F.,.F.,(4,3,4),(2.02528467117779,2.13089662893088,
2.23650858668398),.UNSPECIFIED.);
#814=B_SPLINE_CURVE_WITH_KNOTS('',3,(#41477,#41478,#41479,#41480,#41481,
#41482,#41483),.UNSPECIFIED.,.F.,.F.,(4,3,4),(-0.105834892152832,0.,0.105834892152832),
 .UNSPECIFIED.);
#815=B_SPLINE_CURVE_WITH_KNOTS('',3,(#41497,#41498,#41499,#41500,#41501,
#41502),.UNSPECIFIED.,.F.,.F.,(4,2,4),(0.436494357616822,0.49057908163088,
0.523269669927398),.UNSPECIFIED.);
#816=B_SPLINE_CURVE_WITH_KNOTS('',3,(#41504,#41505,#41506,#41507,#41508,
#41509,#41510,#41511,#41512,#41513,#41514,#41515,#41516,#41517,#41518,#41519,
#41520,#41521,#41522),.UNSPECIFIED.,.F.,.F.,(4,3,3,3,3,3,4),(-0.110253525235377,
-0.070240741437708,-0.0308586443223363,0.,0.03920004219167,0.0788707706428437,
0.110060546834472),.UNSPECIFIED.);
#817=B_SPLINE_CURVE_WITH_KNOTS('',3,(#41524,#41525,#41526,#41527,#41528,
#41529),.UNSPECIFIED.,.F.,.F.,(4,2,4),(0.436484426249657,0.490578640084517,
0.523250481796065),.UNSPECIFIED.);
#818=B_SPLINE_CURVE_WITH_KNOTS('',3,(#41530,#41531,#41532,#41533,#41534,
#41535,#41536,#41537,#41538,#41539,#41540,#41541,#41542,#41543,#41544,#41545,
#41546,#41547,#41548),.UNSPECIFIED.,.F.,.F.,(4,3,3,3,3,3,4),(2.53632937909185,
2.57775416224773,2.61898206719535,2.64590190216638,2.6871740832605,2.72876559667492,
2.75562831582295),.UNSPECIFIED.);
#819=B_SPLINE_CURVE_WITH_KNOTS('',3,(#41551,#41552,#41553,#41554,#41555,
#41556),.UNSPECIFIED.,.F.,.F.,(4,2,4),(1.43904665659616,1.47173724489264,
1.52582196890669),.UNSPECIFIED.);
#820=B_SPLINE_CURVE_WITH_KNOTS('',3,(#41558,#41559,#41560,#41561,#41562,
#41563,#41564,#41565,#41566,#41567,#41568,#41569,#41570,#41571,#41572,#41573,
#41574,#41575,#41576),.UNSPECIFIED.,.F.,.F.,(4,3,3,3,3,3,4),(1.2134406378412,
1.25510987200883,1.29073244309221,1.33189452838107,1.37317594357346,1.41463545273868,
1.43283480298249),.UNSPECIFIED.);
#821=B_SPLINE_CURVE_WITH_KNOTS('',3,(#41578,#41579,#41580,#41581,#41582,
#41583),.UNSPECIFIED.,.F.,.F.,(4,2,4),(1.43904665659616,1.47173724489264,
1.52582196890583),.UNSPECIFIED.);
#822=B_SPLINE_CURVE_WITH_KNOTS('',3,(#41584,#41585,#41586,#41587,#41588,
#41589,#41590,#41591,#41592,#41593,#41594,#41595,#41596,#41597,#41598,#41599,
#41600,#41601,#41602),.UNSPECIFIED.,.F.,.F.,(4,3,3,3,3,3,4),(-1.40481265039411,
-1.36522996541141,-1.32585540726345,-1.28679683363994,-1.26015734748849,
-1.21999608757351,-1.1843388203003),.UNSPECIFIED.);
#823=B_SPLINE_CURVE_WITH_KNOTS('',3,(#41608,#41609,#41610,#41611,#41612,
#41613),.UNSPECIFIED.,.F.,.F.,(4,2,4),(-1.15327512303049,-1.04744023087766,
-0.941605338724826),.UNSPECIFIED.);
#824=B_SPLINE_CURVE_WITH_KNOTS('',3,(#41617,#41618,#41619,#41620,#41621,
#41622),.UNSPECIFIED.,.F.,.F.,(4,2,4),(0.959836356712345,1.06544831446544,
1.17106027221854),.UNSPECIFIED.);
#825=B_SPLINE_CURVE_WITH_KNOTS('',3,(#41629,#41630,#41631,#41632,#41633,
#41634,#41635),.UNSPECIFIED.,.F.,.F.,(4,3,4),(2.02528467117779,2.13089662893088,
2.23650858668398),.UNSPECIFIED.);
#826=B_SPLINE_CURVE_WITH_KNOTS('',3,(#41639,#41640,#41641,#41642,#41643,
#41644,#41645),.UNSPECIFIED.,.F.,.F.,(4,3,4),(-0.105834892152833,0.,0.105834892152832),
 .UNSPECIFIED.);
#827=B_SPLINE_CURVE_WITH_KNOTS('',3,(#41659,#41660,#41661,#41662,#41663,
#41664),.UNSPECIFIED.,.F.,.F.,(4,2,4),(0.436494357616821,0.49057908163088,
0.523269669927355),.UNSPECIFIED.);
#828=B_SPLINE_CURVE_WITH_KNOTS('',3,(#41666,#41667,#41668,#41669,#41670,
#41671,#41672,#41673,#41674,#41675,#41676,#41677,#41678,#41679,#41680,#41681,
#41682,#41683,#41684),.UNSPECIFIED.,.F.,.F.,(4,3,3,3,3,3,4),(-0.110253525235352,
-0.0702407414377446,-0.0308586443223844,0.,0.039200042191676,0.0788707706427867,
0.110060546834448),.UNSPECIFIED.);
#829=B_SPLINE_CURVE_WITH_KNOTS('',3,(#41686,#41687,#41688,#41689,#41690,
#41691),.UNSPECIFIED.,.F.,.F.,(4,2,4),(0.436494357616821,0.49057908163088,
0.523269669927355),.UNSPECIFIED.);
#830=B_SPLINE_CURVE_WITH_KNOTS('',3,(#41692,#41693,#41694,#41695,#41696,
#41697,#41698,#41699,#41700,#41701,#41702,#41703,#41704,#41705,#41706,#41707,
#41708,#41709,#41710),.UNSPECIFIED.,.F.,.F.,(4,3,3,3,3,3,4),(2.53632937909179,
2.57775416224772,2.61898206719534,2.64590190216632,2.68717408326042,2.72876559667486,
2.75562831582289),.UNSPECIFIED.);
#831=B_SPLINE_CURVE_WITH_KNOTS('',3,(#41713,#41714,#41715,#41716,#41717,
#41718),.UNSPECIFIED.,.F.,.F.,(4,2,4),(1.43904665659616,1.47173724489264,
1.5258219689067),.UNSPECIFIED.);
#832=B_SPLINE_CURVE_WITH_KNOTS('',3,(#41720,#41721,#41722,#41723,#41724,
#41725,#41726,#41727,#41728,#41729,#41730,#41731,#41732,#41733,#41734,#41735,
#41736,#41737,#41738),.UNSPECIFIED.,.F.,.F.,(4,3,3,3,3,3,4),(1.21344063784118,
1.25510987200879,1.29073244309219,1.33189452838105,1.37317594357344,1.41463545273868,
1.43283480298247),.UNSPECIFIED.);
#833=B_SPLINE_CURVE_WITH_KNOTS('',3,(#41740,#41741,#41742,#41743,#41744,
#41745),.UNSPECIFIED.,.F.,.F.,(4,2,4),(1.43904665659616,1.47173724489264,
1.52582196890582),.UNSPECIFIED.);
#834=B_SPLINE_CURVE_WITH_KNOTS('',3,(#41746,#41747,#41748,#41749,#41750,
#41751,#41752,#41753,#41754,#41755,#41756,#41757,#41758,#41759,#41760,#41761,
#41762,#41763,#41764),.UNSPECIFIED.,.F.,.F.,(4,3,3,3,3,3,4),(-1.40481265039416,
-1.36522996541145,-1.32585540726348,-1.28679683363997,-1.26015734748853,
-1.21999608757355,-1.18433882030033),.UNSPECIFIED.);
#835=B_SPLINE_CURVE_WITH_KNOTS('',3,(#41770,#41771,#41772,#41773,#41774,
#41775),.UNSPECIFIED.,.F.,.F.,(4,2,4),(-1.15327512303049,-1.04744023087766,
-0.941605338724826),.UNSPECIFIED.);
#836=B_SPLINE_CURVE_WITH_KNOTS('',3,(#41779,#41780,#41781,#41782,#41783,
#41784),.UNSPECIFIED.,.F.,.F.,(4,2,4),(0.959836356712344,1.06544831446544,
1.17106027221854),.UNSPECIFIED.);
#837=B_SPLINE_CURVE_WITH_KNOTS('',3,(#41791,#41792,#41793,#41794,#41795,
#41796,#41797),.UNSPECIFIED.,.F.,.F.,(4,3,4),(2.02528467117778,2.13089662893088,
2.23650858668398),.UNSPECIFIED.);
#838=B_SPLINE_CURVE_WITH_KNOTS('',3,(#41801,#41802,#41803,#41804,#41805,
#41806,#41807),.UNSPECIFIED.,.F.,.F.,(4,3,4),(-0.105834892152833,0.,0.105834892152832),
 .UNSPECIFIED.);
#839=B_SPLINE_CURVE_WITH_KNOTS('',3,(#41821,#41822,#41823,#41824,#41825,
#41826,#41827,#41828,#41829,#41830,#41831,#41832,#41833,#41834,#41835,#41836,
#41837,#41838,#41839),.UNSPECIFIED.,.F.,.F.,(4,3,3,3,3,3,4),(2.47883976068978,
2.51859129056809,2.55786629068885,2.58890030752247,2.62818560996811,2.66809093310445,
2.69915383275782),.UNSPECIFIED.);
#840=B_SPLINE_CURVE_WITH_KNOTS('',3,(#41841,#41842,#41843,#41844,#41845,
#41846),.UNSPECIFIED.,.F.,.F.,(4,2,4),(-0.523250481795879,-0.490578640084517,
-0.43648442624966),.UNSPECIFIED.);
#841=B_SPLINE_CURVE_WITH_KNOTS('',3,(#41848,#41849,#41850,#41851,#41852,
#41853,#41854,#41855,#41856,#41857,#41858,#41859,#41860,#41861,#41862,#41863,
#41864,#41865,#41866),.UNSPECIFIED.,.F.,.F.,(4,3,3,3,3,3,4),(-0.109726413656553,
-0.0680893754924848,-0.0267736956128723,0.,0.0412006233150074,0.082597721206199,
0.109572523074534),.UNSPECIFIED.);
#842=B_SPLINE_CURVE_WITH_KNOTS('',3,(#41867,#41868,#41869,#41870,#41871,
#41872),.UNSPECIFIED.,.F.,.F.,(4,2,4),(-0.523250481795672,-0.490578640084517,
-0.436484426249653),.UNSPECIFIED.);
#843=B_SPLINE_CURVE_WITH_KNOTS('',3,(#41875,#41876,#41877,#41878,#41879,
#41880),.UNSPECIFIED.,.F.,.F.,(4,2,4),(1.43904665659616,1.47173724489264,
1.5258219689067),.UNSPECIFIED.);
#844=B_SPLINE_CURVE_WITH_KNOTS('',3,(#41882,#41883,#41884,#41885,#41886,
#41887,#41888,#41889,#41890,#41891,#41892,#41893,#41894,#41895,#41896,#41897,
#41898,#41899,#41900),.UNSPECIFIED.,.F.,.F.,(4,3,3,3,3,3,4),(1.21344063784118,
1.25510987200878,1.29073244309219,1.33189452838105,1.37317594357344,1.41463545273868,
1.43283480298247),.UNSPECIFIED.);
#845=B_SPLINE_CURVE_WITH_KNOTS('',3,(#41902,#41903,#41904,#41905,#41906,
#41907),.UNSPECIFIED.,.F.,.F.,(4,2,4),(1.43904665659617,1.47173724489264,
1.52582196890583),.UNSPECIFIED.);
#846=B_SPLINE_CURVE_WITH_KNOTS('',3,(#41908,#41909,#41910,#41911,#41912,
#41913,#41914,#41915,#41916,#41917,#41918,#41919,#41920,#41921,#41922,#41923,
#41924,#41925,#41926),.UNSPECIFIED.,.F.,.F.,(4,3,3,3,3,3,4),(-1.40481265039414,
-1.36522996541144,-1.32585540726348,-1.28679683363997,-1.26015734748851,
-1.21999608757358,-1.18433882030032),.UNSPECIFIED.);
#847=B_SPLINE_CURVE_WITH_KNOTS('',3,(#41936,#41937,#41938,#41939,#41940,
#41941,#41942),.UNSPECIFIED.,.F.,.F.,(4,3,4),(2.02528467117778,2.13089662893088,
2.23650858668398),.UNSPECIFIED.);
#848=B_SPLINE_CURVE_WITH_KNOTS('',3,(#41946,#41947,#41948,#41949,#41950,
#41951,#41952),.UNSPECIFIED.,.F.,.F.,(4,3,4),(-0.105834892152832,0.,0.105834892152832),
 .UNSPECIFIED.);
#849=B_SPLINE_CURVE_WITH_KNOTS('',3,(#41957,#41958,#41959,#41960,#41961,
#41962),.UNSPECIFIED.,.F.,.F.,(4,2,4),(0.941605338724826,1.04744023087766,
1.15327512303049),.UNSPECIFIED.);
#850=B_SPLINE_CURVE_WITH_KNOTS('',3,(#41965,#41966,#41967,#41968,#41969,
#41970),.UNSPECIFIED.,.F.,.F.,(4,2,4),(-1.17106027221854,-1.06544831446544,
-0.959836356712344),.UNSPECIFIED.);
#851=B_SPLINE_CURVE_WITH_KNOTS('',3,(#41980,#41981,#41982,#41983,#41984,
#41985),.UNSPECIFIED.,.F.,.F.,(4,2,4),(-1.15327512303049,-1.04744023087766,
-0.941605338724827),.UNSPECIFIED.);
#852=B_SPLINE_CURVE_WITH_KNOTS('',3,(#41989,#41990,#41991,#41992,#41993,
#41994),.UNSPECIFIED.,.F.,.F.,(4,2,4),(0.959836356712344,1.06544831446544,
1.17106027221854),.UNSPECIFIED.);
#853=B_SPLINE_CURVE_WITH_KNOTS('',3,(#42001,#42002,#42003,#42004,#42005,
#42006,#42007),.UNSPECIFIED.,.F.,.F.,(4,3,4),(2.02528467117778,2.13089662893088,
2.23650858668398),.UNSPECIFIED.);
#854=B_SPLINE_CURVE_WITH_KNOTS('',3,(#42011,#42012,#42013,#42014,#42015,
#42016,#42017),.UNSPECIFIED.,.F.,.F.,(4,3,4),(-0.105834892152833,0.,0.105834892152832),
 .UNSPECIFIED.);
#855=B_SPLINE_CURVE_WITH_KNOTS('',3,(#42031,#42032,#42033,#42034,#42035,
#42036),.UNSPECIFIED.,.F.,.F.,(4,2,4),(0.43648442624966,0.490578640084517,
0.523250481795913),.UNSPECIFIED.);
#856=B_SPLINE_CURVE_WITH_KNOTS('',3,(#42038,#42039,#42040,#42041,#42042,
#42043,#42044,#42045,#42046,#42047,#42048,#42049,#42050,#42051,#42052,#42053,
#42054,#42055,#42056),.UNSPECIFIED.,.F.,.F.,(4,3,3,3,3,3,4),(-1.40481265039423,
-1.36522996541152,-1.32585540726357,-1.28679683364005,-1.26015734748857,
-1.2199960875736,-1.18433882030035),.UNSPECIFIED.);
#857=B_SPLINE_CURVE_WITH_KNOTS('',3,(#42058,#42059,#42060,#42061,#42062,
#42063),.UNSPECIFIED.,.F.,.F.,(4,2,4),(0.436494357616825,0.49057908163088,
0.523269669927497),.UNSPECIFIED.);
#858=B_SPLINE_CURVE_WITH_KNOTS('',3,(#42064,#42065,#42066,#42067,#42068,
#42069,#42070,#42071,#42072,#42073,#42074,#42075,#42076,#42077,#42078,#42079,
#42080,#42081,#42082),.UNSPECIFIED.,.F.,.F.,(4,3,3,3,3,3,4),(1.21344063784115,
1.25510987200874,1.29073244309218,1.33189452838104,1.37317594357343,1.41463545273866,
1.43283480298248),.UNSPECIFIED.);
#859=B_SPLINE_CURVE_WITH_KNOTS('',3,(#42085,#42086,#42087,#42088,#42089,
#42090),.UNSPECIFIED.,.F.,.F.,(4,2,4),(1.43906407854219,1.47173592025355,
1.52583013408841),.UNSPECIFIED.);
#860=B_SPLINE_CURVE_WITH_KNOTS('',3,(#42092,#42093,#42094,#42095,#42096,
#42097,#42098,#42099,#42100,#42101,#42102,#42103,#42104,#42105,#42106,#42107,
#42108,#42109,#42110),.UNSPECIFIED.,.F.,.F.,(4,3,3,3,3,3,4),(2.53632937909179,
2.57775416224768,2.61898206719531,2.64590190216631,2.68717408326042,2.72876559667485,
2.75562831582286),.UNSPECIFIED.);
#861=B_SPLINE_CURVE_WITH_KNOTS('',3,(#42112,#42113,#42114,#42115,#42116,
#42117),.UNSPECIFIED.,.F.,.F.,(4,2,4),(1.43906407854219,1.47173592025355,
1.52583013408754),.UNSPECIFIED.);
#862=B_SPLINE_CURVE_WITH_KNOTS('',3,(#42118,#42119,#42120,#42121,#42122,
#42123,#42124,#42125,#42126,#42127,#42128,#42129,#42130,#42131,#42132,#42133,
#42134,#42135,#42136),.UNSPECIFIED.,.F.,.F.,(4,3,3,3,3,3,4),(-0.110253525235352,
-0.0702407414376601,-0.030858644322292,0.,0.0392000421916706,0.0788707706427867,
0.110060546834447),.UNSPECIFIED.);
#863=B_SPLINE_CURVE_WITH_KNOTS('',3,(#42424,#42425,#42426,#42427,#42428,
#42429),.UNSPECIFIED.,.F.,.F.,(4,2,4),(0.436494357616827,0.49057908163088,
0.523269669927392),.UNSPECIFIED.);
#864=B_SPLINE_CURVE_WITH_KNOTS('',3,(#42431,#42432,#42433,#42434,#42435,
#42436,#42437,#42438,#42439,#42440,#42441,#42442,#42443,#42444,#42445,#42446,
#42447,#42448,#42449),.UNSPECIFIED.,.F.,.F.,(4,3,3,3,3,3,4),(-1.40481265039417,
-1.36522996541144,-1.32585540726346,-1.28679683363995,-1.26015734748852,
-1.21999608757349,-1.1843388203003),.UNSPECIFIED.);
#865=B_SPLINE_CURVE_WITH_KNOTS('',3,(#42451,#42452,#42453,#42454,#42455,
#42456),.UNSPECIFIED.,.F.,.F.,(4,2,4),(0.436494357616828,0.49057908163088,
0.523269669927516),.UNSPECIFIED.);
#866=B_SPLINE_CURVE_WITH_KNOTS('',3,(#42457,#42458,#42459,#42460,#42461,
#42462,#42463,#42464,#42465,#42466,#42467,#42468,#42469,#42470,#42471,#42472,
#42473,#42474,#42475),.UNSPECIFIED.,.F.,.F.,(4,3,3,3,3,3,4),(1.21344063784114,
1.25510987200879,1.29073244309217,1.33189452838103,1.37317594357341,1.41463545273866,
1.43283480298246),.UNSPECIFIED.);
#867=B_SPLINE_CURVE_WITH_KNOTS('',3,(#42478,#42479,#42480,#42481,#42482,
#42483),.UNSPECIFIED.,.F.,.F.,(4,2,4),(1.43904665659616,1.47173724489264,
1.52582196890669),.UNSPECIFIED.);
#868=B_SPLINE_CURVE_WITH_KNOTS('',3,(#42485,#42486,#42487,#42488,#42489,
#42490,#42491,#42492,#42493,#42494,#42495,#42496,#42497,#42498,#42499,#42500,
#42501,#42502,#42503),.UNSPECIFIED.,.F.,.F.,(4,3,3,3,3,3,4),(2.53632937909178,
2.57775416224765,2.61898206719527,2.6459019021663,2.68717408326041,2.72876559667488,
2.75562831582286),.UNSPECIFIED.);
#869=B_SPLINE_CURVE_WITH_KNOTS('',3,(#42505,#42506,#42507,#42508,#42509,
#42510),.UNSPECIFIED.,.F.,.F.,(4,2,4),(1.43904665659616,1.47173724489264,
1.52582196890582),.UNSPECIFIED.);
#870=B_SPLINE_CURVE_WITH_KNOTS('',3,(#42511,#42512,#42513,#42514,#42515,
#42516,#42517,#42518,#42519,#42520,#42521,#42522,#42523,#42524,#42525,#42526,
#42527,#42528,#42529),.UNSPECIFIED.,.F.,.F.,(4,3,3,3,3,3,4),(-0.110253525235352,
-0.070240741437667,-0.0308586443223014,0.,0.0392000421916667,0.0788707706427855,
0.110060546834446),.UNSPECIFIED.);
#871=B_SPLINE_CURVE_WITH_KNOTS('',3,(#42535,#42536,#42537,#42538,#42539,
#42540),.UNSPECIFIED.,.F.,.F.,(4,2,4),(-1.15327512303049,-1.04744023087766,
-0.941605338724827),.UNSPECIFIED.);
#872=B_SPLINE_CURVE_WITH_KNOTS('',3,(#42544,#42545,#42546,#42547,#42548,
#42549),.UNSPECIFIED.,.F.,.F.,(4,2,4),(0.959836356712345,1.06544831446544,
1.17106027221854),.UNSPECIFIED.);
#873=B_SPLINE_CURVE_WITH_KNOTS('',3,(#42556,#42557,#42558,#42559,#42560,
#42561,#42562),.UNSPECIFIED.,.F.,.F.,(4,3,4),(2.02528467117779,2.13089662893088,
2.23650858668398),.UNSPECIFIED.);
#874=B_SPLINE_CURVE_WITH_KNOTS('',3,(#42566,#42567,#42568,#42569,#42570,
#42571,#42572),.UNSPECIFIED.,.F.,.F.,(4,3,4),(-0.105834892152833,0.,0.105834892152833),
 .UNSPECIFIED.);
#875=B_SPLINE_CURVE_WITH_KNOTS('',3,(#42586,#42587,#42588,#42589,#42590,
#42591),.UNSPECIFIED.,.F.,.F.,(4,2,4),(0.436494357616816,0.49057908163088,
0.523269669927352),.UNSPECIFIED.);
#876=B_SPLINE_CURVE_WITH_KNOTS('',3,(#42593,#42594,#42595,#42596,#42597,
#42598,#42599,#42600,#42601,#42602,#42603,#42604,#42605,#42606,#42607,#42608,
#42609,#42610,#42611),.UNSPECIFIED.,.F.,.F.,(4,3,3,3,3,3,4),(-1.40481265039413,
-1.36522996541145,-1.32585540726349,-1.28679683363998,-1.2601573474885,
-1.21999608757352,-1.18433882030031),.UNSPECIFIED.);
#877=B_SPLINE_CURVE_WITH_KNOTS('',3,(#42613,#42614,#42615,#42616,#42617,
#42618),.UNSPECIFIED.,.F.,.F.,(4,2,4),(0.436484426249651,0.490578640084517,
0.523250481795878),.UNSPECIFIED.);
#878=B_SPLINE_CURVE_WITH_KNOTS('',3,(#42619,#42620,#42621,#42622,#42623,
#42624,#42625,#42626,#42627,#42628,#42629,#42630,#42631,#42632,#42633,#42634,
#42635,#42636,#42637),.UNSPECIFIED.,.F.,.F.,(4,3,3,3,3,3,4),(1.21344063784117,
1.2551098720088,1.29073244309219,1.33189452838105,1.37317594357344,1.41463545273871,
1.43283480298249),.UNSPECIFIED.);
#879=B_SPLINE_CURVE_WITH_KNOTS('',3,(#42640,#42641,#42642,#42643,#42644,
#42645),.UNSPECIFIED.,.F.,.F.,(4,2,4),(1.43906407854219,1.47173592025355,
1.52583013408841),.UNSPECIFIED.);
#880=B_SPLINE_CURVE_WITH_KNOTS('',3,(#42647,#42648,#42649,#42650,#42651,
#42652,#42653,#42654,#42655,#42656,#42657,#42658,#42659,#42660,#42661,#42662,
#42663,#42664,#42665),.UNSPECIFIED.,.F.,.F.,(4,3,3,3,3,3,4),(2.53632937909181,
2.57775416224765,2.61898206719527,2.64590190216633,2.68717408326044,2.72876559667489,
2.75562831582288),.UNSPECIFIED.);
#881=B_SPLINE_CURVE_WITH_KNOTS('',3,(#42667,#42668,#42669,#42670,#42671,
#42672),.UNSPECIFIED.,.F.,.F.,(4,2,4),(1.43906407854219,1.47173592025355,
1.52583013408754),.UNSPECIFIED.);
#882=B_SPLINE_CURVE_WITH_KNOTS('',3,(#42673,#42674,#42675,#42676,#42677,
#42678,#42679,#42680,#42681,#42682,#42683,#42684,#42685,#42686,#42687,#42688,
#42689,#42690,#42691),.UNSPECIFIED.,.F.,.F.,(4,3,3,3,3,3,4),(-0.110253525235351,
-0.0702407414376934,-0.0308586443223274,0.,0.0392000421916682,0.0788707706427895,
0.110060546834446),.UNSPECIFIED.);
#883=B_SPLINE_CURVE_WITH_KNOTS('',3,(#42697,#42698,#42699,#42700,#42701,
#42702),.UNSPECIFIED.,.F.,.F.,(4,2,4),(-1.15327512303049,-1.04744023087766,
-0.941605338724829),.UNSPECIFIED.);
#884=B_SPLINE_CURVE_WITH_KNOTS('',3,(#42706,#42707,#42708,#42709,#42710,
#42711),.UNSPECIFIED.,.F.,.F.,(4,2,4),(0.959836356712343,1.06544831446544,
1.17106027221854),.UNSPECIFIED.);
#885=B_SPLINE_CURVE_WITH_KNOTS('',3,(#42718,#42719,#42720,#42721,#42722,
#42723,#42724),.UNSPECIFIED.,.F.,.F.,(4,3,4),(2.02528467117778,2.13089662893088,
2.23650858668398),.UNSPECIFIED.);
#886=B_SPLINE_CURVE_WITH_KNOTS('',3,(#42728,#42729,#42730,#42731,#42732,
#42733,#42734),.UNSPECIFIED.,.F.,.F.,(4,3,4),(-0.105834892152834,0.,0.105834892152833),
 .UNSPECIFIED.);
#887=B_SPLINE_CURVE_WITH_KNOTS('',3,(#42748,#42749,#42750,#42751,#42752,
#42753),.UNSPECIFIED.,.F.,.F.,(4,2,4),(0.436484426249655,0.490578640084517,
0.523250481795882),.UNSPECIFIED.);
#888=B_SPLINE_CURVE_WITH_KNOTS('',3,(#42755,#42756,#42757,#42758,#42759,
#42760,#42761,#42762,#42763,#42764,#42765,#42766,#42767,#42768,#42769,#42770,
#42771,#42772,#42773),.UNSPECIFIED.,.F.,.F.,(4,3,3,3,3,3,4),(-0.110253525235353,
-0.0702407414376493,-0.0308586443222864,0.,0.0392000421916586,0.0788707706427754,
0.110060546834447),.UNSPECIFIED.);
#889=B_SPLINE_CURVE_WITH_KNOTS('',3,(#42775,#42776,#42777,#42778,#42779,
#42780),.UNSPECIFIED.,.F.,.F.,(4,2,4),(0.436494357616821,0.49057908163088,
0.523269669927365),.UNSPECIFIED.);
#890=B_SPLINE_CURVE_WITH_KNOTS('',3,(#42781,#42782,#42783,#42784,#42785,
#42786,#42787,#42788,#42789,#42790,#42791,#42792,#42793,#42794,#42795,#42796,
#42797,#42798,#42799),.UNSPECIFIED.,.F.,.F.,(4,3,3,3,3,3,4),(2.53632937909178,
2.57775416224762,2.61898206719525,2.64590190216632,2.68717408326042,2.72876559667488,
2.75562831582289),.UNSPECIFIED.);
#891=B_SPLINE_CURVE_WITH_KNOTS('',3,(#42802,#42803,#42804,#42805,#42806,
#42807),.UNSPECIFIED.,.F.,.F.,(4,2,4),(1.43906407854219,1.47173592025355,
1.52583013408841),.UNSPECIFIED.);
#892=B_SPLINE_CURVE_WITH_KNOTS('',3,(#42809,#42810,#42811,#42812,#42813,
#42814,#42815,#42816,#42817,#42818,#42819,#42820,#42821,#42822,#42823,#42824,
#42825,#42826,#42827),.UNSPECIFIED.,.F.,.F.,(4,3,3,3,3,3,4),(1.21344063784118,
1.25510987200885,1.29073244309219,1.33189452838105,1.37317594357345,1.41463545273868,
1.43283480298247),.UNSPECIFIED.);
#893=B_SPLINE_CURVE_WITH_KNOTS('',3,(#42829,#42830,#42831,#42832,#42833,
#42834),.UNSPECIFIED.,.F.,.F.,(4,2,4),(1.43906407854219,1.47173592025355,
1.52583013408753),.UNSPECIFIED.);
#894=B_SPLINE_CURVE_WITH_KNOTS('',3,(#42835,#42836,#42837,#42838,#42839,
#42840,#42841,#42842,#42843,#42844,#42845,#42846,#42847,#42848,#42849,#42850,
#42851,#42852,#42853),.UNSPECIFIED.,.F.,.F.,(4,3,3,3,3,3,4),(-1.40481265039415,
-1.36522996541142,-1.32585540726345,-1.28679683363994,-1.26015734748852,
-1.21999608757345,-1.18433882030032),.UNSPECIFIED.);
#895=B_SPLINE_CURVE_WITH_KNOTS('',3,(#42859,#42860,#42861,#42862,#42863,
#42864),.UNSPECIFIED.,.F.,.F.,(4,2,4),(-1.15327512303049,-1.04744023087766,
-0.941605338724827),.UNSPECIFIED.);
#896=B_SPLINE_CURVE_WITH_KNOTS('',3,(#42868,#42869,#42870,#42871,#42872,
#42873),.UNSPECIFIED.,.F.,.F.,(4,2,4),(0.959836356712344,1.06544831446544,
1.17106027221854),.UNSPECIFIED.);
#897=B_SPLINE_CURVE_WITH_KNOTS('',3,(#42880,#42881,#42882,#42883,#42884,
#42885,#42886),.UNSPECIFIED.,.F.,.F.,(4,3,4),(2.02528467117779,2.13089662893088,
2.23650858668398),.UNSPECIFIED.);
#898=B_SPLINE_CURVE_WITH_KNOTS('',3,(#42890,#42891,#42892,#42893,#42894,
#42895,#42896),.UNSPECIFIED.,.F.,.F.,(4,3,4),(-0.105834892152832,0.,0.105834892152832),
 .UNSPECIFIED.);
#899=B_SPLINE_CURVE_WITH_KNOTS('',3,(#42910,#42911,#42912,#42913,#42914,
#42915),.UNSPECIFIED.,.F.,.F.,(4,2,4),(0.436494357616822,0.49057908163088,
0.523269669927398),.UNSPECIFIED.);
#900=B_SPLINE_CURVE_WITH_KNOTS('',3,(#42917,#42918,#42919,#42920,#42921,
#42922,#42923,#42924,#42925,#42926,#42927,#42928,#42929,#42930,#42931,#42932,
#42933,#42934,#42935),.UNSPECIFIED.,.F.,.F.,(4,3,3,3,3,3,4),(-0.110253525235377,
-0.070240741437708,-0.0308586443223363,0.,0.03920004219167,0.0788707706428437,
0.110060546834472),.UNSPECIFIED.);
#901=B_SPLINE_CURVE_WITH_KNOTS('',3,(#42937,#42938,#42939,#42940,#42941,
#42942),.UNSPECIFIED.,.F.,.F.,(4,2,4),(0.436484426249657,0.490578640084517,
0.523250481796065),.UNSPECIFIED.);
#902=B_SPLINE_CURVE_WITH_KNOTS('',3,(#42943,#42944,#42945,#42946,#42947,
#42948,#42949,#42950,#42951,#42952,#42953,#42954,#42955,#42956,#42957,#42958,
#42959,#42960,#42961),.UNSPECIFIED.,.F.,.F.,(4,3,3,3,3,3,4),(2.53632937909185,
2.57775416224773,2.61898206719535,2.64590190216638,2.6871740832605,2.72876559667492,
2.75562831582295),.UNSPECIFIED.);
#903=B_SPLINE_CURVE_WITH_KNOTS('',3,(#42964,#42965,#42966,#42967,#42968,
#42969),.UNSPECIFIED.,.F.,.F.,(4,2,4),(1.43904665659616,1.47173724489264,
1.52582196890669),.UNSPECIFIED.);
#904=B_SPLINE_CURVE_WITH_KNOTS('',3,(#42971,#42972,#42973,#42974,#42975,
#42976,#42977,#42978,#42979,#42980,#42981,#42982,#42983,#42984,#42985,#42986,
#42987,#42988,#42989),.UNSPECIFIED.,.F.,.F.,(4,3,3,3,3,3,4),(1.2134406378412,
1.25510987200883,1.29073244309221,1.33189452838107,1.37317594357346,1.41463545273868,
1.43283480298249),.UNSPECIFIED.);
#905=B_SPLINE_CURVE_WITH_KNOTS('',3,(#42991,#42992,#42993,#42994,#42995,
#42996),.UNSPECIFIED.,.F.,.F.,(4,2,4),(1.43904665659616,1.47173724489264,
1.52582196890583),.UNSPECIFIED.);
#906=B_SPLINE_CURVE_WITH_KNOTS('',3,(#42997,#42998,#42999,#43000,#43001,
#43002,#43003,#43004,#43005,#43006,#43007,#43008,#43009,#43010,#43011,#43012,
#43013,#43014,#43015),.UNSPECIFIED.,.F.,.F.,(4,3,3,3,3,3,4),(-1.40481265039411,
-1.36522996541141,-1.32585540726345,-1.28679683363994,-1.26015734748849,
-1.21999608757351,-1.1843388203003),.UNSPECIFIED.);
#907=B_SPLINE_CURVE_WITH_KNOTS('',3,(#43021,#43022,#43023,#43024,#43025,
#43026),.UNSPECIFIED.,.F.,.F.,(4,2,4),(-1.15327512303049,-1.04744023087766,
-0.941605338724826),.UNSPECIFIED.);
#908=B_SPLINE_CURVE_WITH_KNOTS('',3,(#43030,#43031,#43032,#43033,#43034,
#43035),.UNSPECIFIED.,.F.,.F.,(4,2,4),(0.959836356712345,1.06544831446544,
1.17106027221854),.UNSPECIFIED.);
#909=B_SPLINE_CURVE_WITH_KNOTS('',3,(#43042,#43043,#43044,#43045,#43046,
#43047,#43048),.UNSPECIFIED.,.F.,.F.,(4,3,4),(2.02528467117779,2.13089662893088,
2.23650858668398),.UNSPECIFIED.);
#910=B_SPLINE_CURVE_WITH_KNOTS('',3,(#43052,#43053,#43054,#43055,#43056,
#43057,#43058),.UNSPECIFIED.,.F.,.F.,(4,3,4),(-0.105834892152833,0.,0.105834892152832),
 .UNSPECIFIED.);
#911=B_SPLINE_CURVE_WITH_KNOTS('',3,(#43072,#43073,#43074,#43075,#43076,
#43077),.UNSPECIFIED.,.F.,.F.,(4,2,4),(0.436494357616821,0.49057908163088,
0.523269669927355),.UNSPECIFIED.);
#912=B_SPLINE_CURVE_WITH_KNOTS('',3,(#43079,#43080,#43081,#43082,#43083,
#43084,#43085,#43086,#43087,#43088,#43089,#43090,#43091,#43092,#43093,#43094,
#43095,#43096,#43097),.UNSPECIFIED.,.F.,.F.,(4,3,3,3,3,3,4),(-0.110253525235352,
-0.0702407414377446,-0.0308586443223844,0.,0.039200042191676,0.0788707706427867,
0.110060546834448),.UNSPECIFIED.);
#913=B_SPLINE_CURVE_WITH_KNOTS('',3,(#43099,#43100,#43101,#43102,#43103,
#43104),.UNSPECIFIED.,.F.,.F.,(4,2,4),(0.436494357616821,0.49057908163088,
0.523269669927355),.UNSPECIFIED.);
#914=B_SPLINE_CURVE_WITH_KNOTS('',3,(#43105,#43106,#43107,#43108,#43109,
#43110,#43111,#43112,#43113,#43114,#43115,#43116,#43117,#43118,#43119,#43120,
#43121,#43122,#43123),.UNSPECIFIED.,.F.,.F.,(4,3,3,3,3,3,4),(2.53632937909179,
2.57775416224772,2.61898206719534,2.64590190216632,2.68717408326042,2.72876559667486,
2.75562831582289),.UNSPECIFIED.);
#915=B_SPLINE_CURVE_WITH_KNOTS('',3,(#43126,#43127,#43128,#43129,#43130,
#43131),.UNSPECIFIED.,.F.,.F.,(4,2,4),(1.43904665659616,1.47173724489264,
1.5258219689067),.UNSPECIFIED.);
#916=B_SPLINE_CURVE_WITH_KNOTS('',3,(#43133,#43134,#43135,#43136,#43137,
#43138,#43139,#43140,#43141,#43142,#43143,#43144,#43145,#43146,#43147,#43148,
#43149,#43150,#43151),.UNSPECIFIED.,.F.,.F.,(4,3,3,3,3,3,4),(1.21344063784118,
1.25510987200879,1.29073244309219,1.33189452838105,1.37317594357344,1.41463545273868,
1.43283480298247),.UNSPECIFIED.);
#917=B_SPLINE_CURVE_WITH_KNOTS('',3,(#43153,#43154,#43155,#43156,#43157,
#43158),.UNSPECIFIED.,.F.,.F.,(4,2,4),(1.43904665659616,1.47173724489264,
1.52582196890582),.UNSPECIFIED.);
#918=B_SPLINE_CURVE_WITH_KNOTS('',3,(#43159,#43160,#43161,#43162,#43163,
#43164,#43165,#43166,#43167,#43168,#43169,#43170,#43171,#43172,#43173,#43174,
#43175,#43176,#43177),.UNSPECIFIED.,.F.,.F.,(4,3,3,3,3,3,4),(-1.40481265039416,
-1.36522996541145,-1.32585540726348,-1.28679683363997,-1.26015734748853,
-1.21999608757355,-1.18433882030033),.UNSPECIFIED.);
#919=B_SPLINE_CURVE_WITH_KNOTS('',3,(#43183,#43184,#43185,#43186,#43187,
#43188),.UNSPECIFIED.,.F.,.F.,(4,2,4),(-1.15327512303049,-1.04744023087766,
-0.941605338724826),.UNSPECIFIED.);
#920=B_SPLINE_CURVE_WITH_KNOTS('',3,(#43192,#43193,#43194,#43195,#43196,
#43197),.UNSPECIFIED.,.F.,.F.,(4,2,4),(0.959836356712344,1.06544831446544,
1.17106027221854),.UNSPECIFIED.);
#921=B_SPLINE_CURVE_WITH_KNOTS('',3,(#43204,#43205,#43206,#43207,#43208,
#43209,#43210),.UNSPECIFIED.,.F.,.F.,(4,3,4),(2.02528467117778,2.13089662893088,
2.23650858668398),.UNSPECIFIED.);
#922=B_SPLINE_CURVE_WITH_KNOTS('',3,(#43214,#43215,#43216,#43217,#43218,
#43219,#43220),.UNSPECIFIED.,.F.,.F.,(4,3,4),(-0.105834892152833,0.,0.105834892152832),
 .UNSPECIFIED.);
#923=B_SPLINE_CURVE_WITH_KNOTS('',3,(#43234,#43235,#43236,#43237,#43238,
#43239,#43240,#43241,#43242,#43243,#43244,#43245,#43246,#43247,#43248,#43249,
#43250,#43251,#43252),.UNSPECIFIED.,.F.,.F.,(4,3,3,3,3,3,4),(2.47883976068978,
2.51859129056809,2.55786629068885,2.58890030752247,2.62818560996811,2.66809093310445,
2.69915383275782),.UNSPECIFIED.);
#924=B_SPLINE_CURVE_WITH_KNOTS('',3,(#43254,#43255,#43256,#43257,#43258,
#43259),.UNSPECIFIED.,.F.,.F.,(4,2,4),(-0.523250481795879,-0.490578640084517,
-0.43648442624966),.UNSPECIFIED.);
#925=B_SPLINE_CURVE_WITH_KNOTS('',3,(#43261,#43262,#43263,#43264,#43265,
#43266,#43267,#43268,#43269,#43270,#43271,#43272,#43273,#43274,#43275,#43276,
#43277,#43278,#43279),.UNSPECIFIED.,.F.,.F.,(4,3,3,3,3,3,4),(-0.109726413656553,
-0.0680893754924848,-0.0267736956128723,0.,0.0412006233150074,0.082597721206199,
0.109572523074534),.UNSPECIFIED.);
#926=B_SPLINE_CURVE_WITH_KNOTS('',3,(#43280,#43281,#43282,#43283,#43284,
#43285),.UNSPECIFIED.,.F.,.F.,(4,2,4),(-0.523250481795672,-0.490578640084517,
-0.436484426249653),.UNSPECIFIED.);
#927=B_SPLINE_CURVE_WITH_KNOTS('',3,(#43288,#43289,#43290,#43291,#43292,
#43293),.UNSPECIFIED.,.F.,.F.,(4,2,4),(1.43904665659616,1.47173724489264,
1.5258219689067),.UNSPECIFIED.);
#928=B_SPLINE_CURVE_WITH_KNOTS('',3,(#43295,#43296,#43297,#43298,#43299,
#43300,#43301,#43302,#43303,#43304,#43305,#43306,#43307,#43308,#43309,#43310,
#43311,#43312,#43313),.UNSPECIFIED.,.F.,.F.,(4,3,3,3,3,3,4),(1.21344063784118,
1.25510987200878,1.29073244309219,1.33189452838105,1.37317594357344,1.41463545273868,
1.43283480298247),.UNSPECIFIED.);
#929=B_SPLINE_CURVE_WITH_KNOTS('',3,(#43315,#43316,#43317,#43318,#43319,
#43320),.UNSPECIFIED.,.F.,.F.,(4,2,4),(1.43904665659617,1.47173724489264,
1.52582196890583),.UNSPECIFIED.);
#930=B_SPLINE_CURVE_WITH_KNOTS('',3,(#43321,#43322,#43323,#43324,#43325,
#43326,#43327,#43328,#43329,#43330,#43331,#43332,#43333,#43334,#43335,#43336,
#43337,#43338,#43339),.UNSPECIFIED.,.F.,.F.,(4,3,3,3,3,3,4),(-1.40481265039414,
-1.36522996541144,-1.32585540726348,-1.28679683363997,-1.26015734748851,
-1.21999608757358,-1.18433882030032),.UNSPECIFIED.);
#931=B_SPLINE_CURVE_WITH_KNOTS('',3,(#43349,#43350,#43351,#43352,#43353,
#43354,#43355),.UNSPECIFIED.,.F.,.F.,(4,3,4),(2.02528467117778,2.13089662893088,
2.23650858668398),.UNSPECIFIED.);
#932=B_SPLINE_CURVE_WITH_KNOTS('',3,(#43359,#43360,#43361,#43362,#43363,
#43364,#43365),.UNSPECIFIED.,.F.,.F.,(4,3,4),(-0.105834892152832,0.,0.105834892152832),
 .UNSPECIFIED.);
#933=B_SPLINE_CURVE_WITH_KNOTS('',3,(#43370,#43371,#43372,#43373,#43374,
#43375),.UNSPECIFIED.,.F.,.F.,(4,2,4),(0.941605338724826,1.04744023087766,
1.15327512303049),.UNSPECIFIED.);
#934=B_SPLINE_CURVE_WITH_KNOTS('',3,(#43378,#43379,#43380,#43381,#43382,
#43383),.UNSPECIFIED.,.F.,.F.,(4,2,4),(-1.17106027221854,-1.06544831446544,
-0.959836356712344),.UNSPECIFIED.);
#935=B_SPLINE_CURVE_WITH_KNOTS('',3,(#43393,#43394,#43395,#43396,#43397,
#43398),.UNSPECIFIED.,.F.,.F.,(4,2,4),(-1.15327512303049,-1.04744023087766,
-0.941605338724827),.UNSPECIFIED.);
#936=B_SPLINE_CURVE_WITH_KNOTS('',3,(#43402,#43403,#43404,#43405,#43406,
#43407),.UNSPECIFIED.,.F.,.F.,(4,2,4),(0.959836356712344,1.06544831446544,
1.17106027221854),.UNSPECIFIED.);
#937=B_SPLINE_CURVE_WITH_KNOTS('',3,(#43414,#43415,#43416,#43417,#43418,
#43419,#43420),.UNSPECIFIED.,.F.,.F.,(4,3,4),(2.02528467117778,2.13089662893088,
2.23650858668398),.UNSPECIFIED.);
#938=B_SPLINE_CURVE_WITH_KNOTS('',3,(#43424,#43425,#43426,#43427,#43428,
#43429,#43430),.UNSPECIFIED.,.F.,.F.,(4,3,4),(-0.105834892152833,0.,0.105834892152832),
 .UNSPECIFIED.);
#939=B_SPLINE_CURVE_WITH_KNOTS('',3,(#43444,#43445,#43446,#43447,#43448,
#43449),.UNSPECIFIED.,.F.,.F.,(4,2,4),(0.43648442624966,0.490578640084517,
0.523250481795913),.UNSPECIFIED.);
#940=B_SPLINE_CURVE_WITH_KNOTS('',3,(#43451,#43452,#43453,#43454,#43455,
#43456,#43457,#43458,#43459,#43460,#43461,#43462,#43463,#43464,#43465,#43466,
#43467,#43468,#43469),.UNSPECIFIED.,.F.,.F.,(4,3,3,3,3,3,4),(-1.40481265039423,
-1.36522996541152,-1.32585540726357,-1.28679683364005,-1.26015734748857,
-1.2199960875736,-1.18433882030035),.UNSPECIFIED.);
#941=B_SPLINE_CURVE_WITH_KNOTS('',3,(#43471,#43472,#43473,#43474,#43475,
#43476),.UNSPECIFIED.,.F.,.F.,(4,2,4),(0.436494357616825,0.49057908163088,
0.523269669927497),.UNSPECIFIED.);
#942=B_SPLINE_CURVE_WITH_KNOTS('',3,(#43477,#43478,#43479,#43480,#43481,
#43482,#43483,#43484,#43485,#43486,#43487,#43488,#43489,#43490,#43491,#43492,
#43493,#43494,#43495),.UNSPECIFIED.,.F.,.F.,(4,3,3,3,3,3,4),(1.21344063784115,
1.25510987200874,1.29073244309218,1.33189452838104,1.37317594357343,1.41463545273866,
1.43283480298248),.UNSPECIFIED.);
#943=B_SPLINE_CURVE_WITH_KNOTS('',3,(#43498,#43499,#43500,#43501,#43502,
#43503),.UNSPECIFIED.,.F.,.F.,(4,2,4),(1.43906407854219,1.47173592025355,
1.52583013408841),.UNSPECIFIED.);
#944=B_SPLINE_CURVE_WITH_KNOTS('',3,(#43505,#43506,#43507,#43508,#43509,
#43510,#43511,#43512,#43513,#43514,#43515,#43516,#43517,#43518,#43519,#43520,
#43521,#43522,#43523),.UNSPECIFIED.,.F.,.F.,(4,3,3,3,3,3,4),(2.53632937909179,
2.57775416224768,2.61898206719531,2.64590190216631,2.68717408326042,2.72876559667485,
2.75562831582286),.UNSPECIFIED.);
#945=B_SPLINE_CURVE_WITH_KNOTS('',3,(#43525,#43526,#43527,#43528,#43529,
#43530),.UNSPECIFIED.,.F.,.F.,(4,2,4),(1.43906407854219,1.47173592025355,
1.52583013408754),.UNSPECIFIED.);
#946=B_SPLINE_CURVE_WITH_KNOTS('',3,(#43531,#43532,#43533,#43534,#43535,
#43536,#43537,#43538,#43539,#43540,#43541,#43542,#43543,#43544,#43545,#43546,
#43547,#43548,#43549),.UNSPECIFIED.,.F.,.F.,(4,3,3,3,3,3,4),(-0.110253525235352,
-0.0702407414376601,-0.030858644322292,0.,0.0392000421916706,0.0788707706427867,
0.110060546834447),.UNSPECIFIED.);
#947=B_SPLINE_SURFACE_WITH_KNOTS('',5,1,((#19405,#19406),(#19407,#19408),
(#19409,#19410),(#19411,#19412),(#19413,#19414),(#19415,#19416),(#19417,
#19418),(#19419,#19420),(#19421,#19422),(#19423,#19424),(#19425,#19426),
(#19427,#19428),(#19429,#19430),(#19431,#19432),(#19433,#19434),(#19435,
#19436),(#19437,#19438),(#19439,#19440),(#19441,#19442),(#19443,#19444),
(#19445,#19446),(#19447,#19448),(#19449,#19450),(#19451,#19452),(#19453,
#19454),(#19455,#19456),(#19457,#19458),(#19459,#19460),(#19461,#19462),
(#19463,#19464),(#19465,#19466),(#19467,#19468),(#19469,#19470),(#19471,
#19472),(#19473,#19474),(#19475,#19476),(#19477,#19478),(#19479,#19480),
(#19481,#19482),(#19483,#19484),(#19485,#19486),(#19487,#19488),(#19489,
#19490),(#19491,#19492),(#19493,#19494),(#19495,#19496),(#19497,#19498),
(#19499,#19500),(#19501,#19502),(#19503,#19504),(#19505,#19506),(#19507,
#19508),(#19509,#19510),(#19511,#19512),(#19513,#19514),(#19515,#19516),
(#19517,#19518),(#19519,#19520),(#19521,#19522),(#19523,#19524),(#19525,
#19526),(#19527,#19528),(#19529,#19530),(#19531,#19532),(#19533,#19534),
(#19535,#19536),(#19537,#19538),(#19539,#19540),(#19541,#19542),(#19543,
#19544),(#19545,#19546),(#19547,#19548),(#19549,#19550),(#19551,#19552),
(#19553,#19554)),.UNSPECIFIED.,.F.,.F.,.F.,(6,1,1,1,1,1,1,1,1,1,1,1,1,1,
1,1,1,1,1,1,1,1,1,1,1,1,1,1,1,1,1,1,1,1,1,1,1,1,1,1,1,1,1,1,1,1,1,1,1,1,
1,1,1,1,1,1,1,1,1,1,1,1,1,1,1,1,1,1,1,1,6),(2,2),(-1.,-0.985714285714284,
-0.97142857142857,-0.957142857142856,-0.942857142857141,-0.928571428571427,
-0.914285714285713,-0.899999999999999,-0.885714285714284,-0.87142857142857,
-0.857142857142856,-0.842857142857142,-0.828571428571428,-0.814285714285713,
-0.799999999999999,-0.785714285714285,-0.771428571428571,-0.757142857142856,
-0.742857142857142,-0.728571428571428,-0.714285714285714,-0.699999999999999,
-0.685714285714285,-0.671428571428571,-0.657142857142857,-0.642857142857142,
-0.628571428571428,-0.614285714285714,-0.6,-0.585714285714286,-0.571428571428571,
-0.557142857142857,-0.542857142857143,-0.528571428571429,-0.514285714285714,
-0.5,-0.485714285714286,-0.471428571428572,-0.457142857142857,-0.442857142857143,
-0.428571428571429,-0.414285714285714,-0.4,-0.385714285714286,-0.371428571428571,
-0.357142857142857,-0.342857142857143,-0.328571428571429,-0.314285714285714,
-0.3,-0.285714285714286,-0.271428571428571,-0.257142857142857,-0.242857142857143,
-0.228571428571429,-0.214285714285714,-0.2,-0.185714285714286,-0.171428571428571,
-0.157142857142857,-0.142857142857143,-0.128571428571429,-0.114285714285714,
-0.1,-0.0857142857142857,-0.0714285714285714,-0.0571428571428571,-0.0428571428571429,
-0.0285714285714286,-0.0142857142857143,0.),(0.,1.8),.UNSPECIFIED.);
#948=B_SPLINE_SURFACE_WITH_KNOTS('',5,1,((#19713,#19714),(#19715,#19716),
(#19717,#19718),(#19719,#19720),(#19721,#19722),(#19723,#19724),(#19725,
#19726),(#19727,#19728),(#19729,#19730),(#19731,#19732),(#19733,#19734),
(#19735,#19736),(#19737,#19738),(#19739,#19740),(#19741,#19742),(#19743,
#19744),(#19745,#19746),(#19747,#19748),(#19749,#19750),(#19751,#19752),
(#19753,#19754),(#19755,#19756),(#19757,#19758),(#19759,#19760),(#19761,
#19762),(#19763,#19764),(#19765,#19766),(#19767,#19768),(#19769,#19770),
(#19771,#19772),(#19773,#19774),(#19775,#19776),(#19777,#19778),(#19779,
#19780),(#19781,#19782),(#19783,#19784),(#19785,#19786),(#19787,#19788),
(#19789,#19790),(#19791,#19792),(#19793,#19794),(#19795,#19796),(#19797,
#19798),(#19799,#19800),(#19801,#19802),(#19803,#19804),(#19805,#19806),
(#19807,#19808),(#19809,#19810),(#19811,#19812),(#19813,#19814),(#19815,
#19816),(#19817,#19818),(#19819,#19820),(#19821,#19822),(#19823,#19824),
(#19825,#19826),(#19827,#19828),(#19829,#19830),(#19831,#19832),(#19833,
#19834),(#19835,#19836),(#19837,#19838),(#19839,#19840),(#19841,#19842),
(#19843,#19844),(#19845,#19846),(#19847,#19848),(#19849,#19850),(#19851,
#19852),(#19853,#19854),(#19855,#19856),(#19857,#19858),(#19859,#19860),
(#19861,#19862)),.UNSPECIFIED.,.F.,.F.,.F.,(6,1,1,1,1,1,1,1,1,1,1,1,1,1,
1,1,1,1,1,1,1,1,1,1,1,1,1,1,1,1,1,1,1,1,1,1,1,1,1,1,1,1,1,1,1,1,1,1,1,1,
1,1,1,1,1,1,1,1,1,1,1,1,1,1,1,1,1,1,1,1,6),(2,2),(0.,0.0142857142857143,
0.0285714285714286,0.0428571428571429,0.0571428571428571,0.0714285714285714,
0.0857142857142857,0.1,0.114285714285714,0.128571428571429,0.142857142857143,
0.157142857142857,0.171428571428571,0.185714285714286,0.2,0.214285714285714,
0.228571428571429,0.242857142857143,0.257142857142857,0.271428571428571,
0.285714285714286,0.3,0.314285714285714,0.328571428571429,0.342857142857143,
0.357142857142857,0.371428571428571,0.385714285714286,0.4,0.414285714285714,
0.428571428571429,0.442857142857143,0.457142857142857,0.471428571428572,
0.485714285714286,0.5,0.514285714285714,0.528571428571429,0.542857142857143,
0.557142857142857,0.571428571428571,0.585714285714286,0.6,0.614285714285714,
0.628571428571428,0.642857142857142,0.657142857142857,0.671428571428571,
0.685714285714285,0.699999999999999,0.714285714285714,0.728571428571428,
0.742857142857142,0.757142857142856,0.771428571428571,0.785714285714285,
0.799999999999999,0.814285714285713,0.828571428571428,0.842857142857142,
0.857142857142856,0.87142857142857,0.885714285714284,0.899999999999999,
0.914285714285713,0.928571428571427,0.942857142857141,0.957142857142856,
0.97142857142857,0.985714285714284,1.),(0.,1.8),.UNSPECIFIED.);
#949=B_SPLINE_SURFACE_WITH_KNOTS('',5,1,((#20011,#20012),(#20013,#20014),
(#20015,#20016),(#20017,#20018),(#20019,#20020),(#20021,#20022),(#20023,
#20024),(#20025,#20026),(#20027,#20028),(#20029,#20030),(#20031,#20032),
(#20033,#20034),(#20035,#20036),(#20037,#20038),(#20039,#20040),(#20041,
#20042),(#20043,#20044),(#20045,#20046),(#20047,#20048),(#20049,#20050),
(#20051,#20052),(#20053,#20054),(#20055,#20056),(#20057,#20058),(#20059,
#20060),(#20061,#20062),(#20063,#20064),(#20065,#20066),(#20067,#20068),
(#20069,#20070),(#20071,#20072),(#20073,#20074),(#20075,#20076),(#20077,
#20078),(#20079,#20080),(#20081,#20082),(#20083,#20084),(#20085,#20086),
(#20087,#20088),(#20089,#20090),(#20091,#20092),(#20093,#20094),(#20095,
#20096),(#20097,#20098),(#20099,#20100),(#20101,#20102),(#20103,#20104),
(#20105,#20106),(#20107,#20108),(#20109,#20110),(#20111,#20112),(#20113,
#20114),(#20115,#20116),(#20117,#20118),(#20119,#20120),(#20121,#20122),
(#20123,#20124),(#20125,#20126),(#20127,#20128),(#20129,#20130),(#20131,
#20132),(#20133,#20134),(#20135,#20136),(#20137,#20138),(#20139,#20140),
(#20141,#20142),(#20143,#20144),(#20145,#20146),(#20147,#20148),(#20149,
#20150),(#20151,#20152),(#20153,#20154),(#20155,#20156),(#20157,#20158),
(#20159,#20160)),.UNSPECIFIED.,.F.,.F.,.F.,(6,1,1,1,1,1,1,1,1,1,1,1,1,1,
1,1,1,1,1,1,1,1,1,1,1,1,1,1,1,1,1,1,1,1,1,1,1,1,1,1,1,1,1,1,1,1,1,1,1,1,
1,1,1,1,1,1,1,1,1,1,1,1,1,1,1,1,1,1,1,1,6),(2,2),(-1.,-0.985714285714284,
-0.97142857142857,-0.957142857142856,-0.942857142857141,-0.928571428571427,
-0.914285714285713,-0.899999999999999,-0.885714285714284,-0.87142857142857,
-0.857142857142856,-0.842857142857142,-0.828571428571428,-0.814285714285713,
-0.799999999999999,-0.785714285714285,-0.771428571428571,-0.757142857142856,
-0.742857142857142,-0.728571428571428,-0.714285714285714,-0.699999999999999,
-0.685714285714285,-0.671428571428571,-0.657142857142857,-0.642857142857142,
-0.628571428571428,-0.614285714285714,-0.6,-0.585714285714286,-0.571428571428571,
-0.557142857142857,-0.542857142857143,-0.528571428571429,-0.514285714285714,
-0.5,-0.485714285714286,-0.471428571428572,-0.457142857142857,-0.442857142857143,
-0.428571428571429,-0.414285714285714,-0.4,-0.385714285714286,-0.371428571428571,
-0.357142857142857,-0.342857142857143,-0.328571428571429,-0.314285714285714,
-0.3,-0.285714285714286,-0.271428571428571,-0.257142857142857,-0.242857142857143,
-0.228571428571429,-0.214285714285714,-0.2,-0.185714285714286,-0.171428571428571,
-0.157142857142857,-0.142857142857143,-0.128571428571429,-0.114285714285714,
-0.1,-0.0857142857142857,-0.0714285714285714,-0.0571428571428571,-0.0428571428571429,
-0.0285714285714286,-0.0142857142857143,0.),(0.,1.8),.UNSPECIFIED.);
#950=B_SPLINE_SURFACE_WITH_KNOTS('',5,1,((#20319,#20320),(#20321,#20322),
(#20323,#20324),(#20325,#20326),(#20327,#20328),(#20329,#20330),(#20331,
#20332),(#20333,#20334),(#20335,#20336),(#20337,#20338),(#20339,#20340),
(#20341,#20342),(#20343,#20344),(#20345,#20346),(#20347,#20348),(#20349,
#20350),(#20351,#20352),(#20353,#20354),(#20355,#20356),(#20357,#20358),
(#20359,#20360),(#20361,#20362),(#20363,#20364),(#20365,#20366),(#20367,
#20368),(#20369,#20370),(#20371,#20372),(#20373,#20374),(#20375,#20376),
(#20377,#20378),(#20379,#20380),(#20381,#20382),(#20383,#20384),(#20385,
#20386),(#20387,#20388),(#20389,#20390),(#20391,#20392),(#20393,#20394),
(#20395,#20396),(#20397,#20398),(#20399,#20400),(#20401,#20402),(#20403,
#20404),(#20405,#20406),(#20407,#20408),(#20409,#20410),(#20411,#20412),
(#20413,#20414),(#20415,#20416),(#20417,#20418),(#20419,#20420),(#20421,
#20422),(#20423,#20424),(#20425,#20426),(#20427,#20428),(#20429,#20430),
(#20431,#20432),(#20433,#20434),(#20435,#20436),(#20437,#20438),(#20439,
#20440),(#20441,#20442),(#20443,#20444),(#20445,#20446),(#20447,#20448),
(#20449,#20450),(#20451,#20452),(#20453,#20454),(#20455,#20456),(#20457,
#20458),(#20459,#20460),(#20461,#20462),(#20463,#20464),(#20465,#20466),
(#20467,#20468)),.UNSPECIFIED.,.F.,.F.,.F.,(6,1,1,1,1,1,1,1,1,1,1,1,1,1,
1,1,1,1,1,1,1,1,1,1,1,1,1,1,1,1,1,1,1,1,1,1,1,1,1,1,1,1,1,1,1,1,1,1,1,1,
1,1,1,1,1,1,1,1,1,1,1,1,1,1,1,1,1,1,1,1,6),(2,2),(0.,0.0142857142857143,
0.0285714285714286,0.0428571428571429,0.0571428571428571,0.0714285714285714,
0.0857142857142857,0.1,0.114285714285714,0.128571428571429,0.142857142857143,
0.157142857142857,0.171428571428571,0.185714285714286,0.2,0.214285714285714,
0.228571428571429,0.242857142857143,0.257142857142857,0.271428571428571,
0.285714285714286,0.3,0.314285714285714,0.328571428571429,0.342857142857143,
0.357142857142857,0.371428571428571,0.385714285714286,0.4,0.414285714285714,
0.428571428571429,0.442857142857143,0.457142857142857,0.471428571428572,
0.485714285714286,0.5,0.514285714285714,0.528571428571429,0.542857142857143,
0.557142857142857,0.571428571428571,0.585714285714286,0.6,0.614285714285714,
0.628571428571428,0.642857142857142,0.657142857142857,0.671428571428571,
0.685714285714285,0.699999999999999,0.714285714285714,0.728571428571428,
0.742857142857142,0.757142857142856,0.771428571428571,0.785714285714285,
0.799999999999999,0.814285714285713,0.828571428571428,0.842857142857142,
0.857142857142856,0.87142857142857,0.885714285714284,0.899999999999999,
0.914285714285713,0.928571428571427,0.942857142857141,0.957142857142856,
0.97142857142857,0.985714285714284,1.),(0.,1.8),.UNSPECIFIED.);
#951=B_SPLINE_SURFACE_WITH_KNOTS('',5,1,((#20617,#20618),(#20619,#20620),
(#20621,#20622),(#20623,#20624),(#20625,#20626),(#20627,#20628),(#20629,
#20630),(#20631,#20632),(#20633,#20634),(#20635,#20636),(#20637,#20638),
(#20639,#20640),(#20641,#20642),(#20643,#20644),(#20645,#20646),(#20647,
#20648),(#20649,#20650),(#20651,#20652),(#20653,#20654),(#20655,#20656),
(#20657,#20658),(#20659,#20660),(#20661,#20662),(#20663,#20664),(#20665,
#20666),(#20667,#20668),(#20669,#20670),(#20671,#20672),(#20673,#20674),
(#20675,#20676),(#20677,#20678),(#20679,#20680),(#20681,#20682),(#20683,
#20684),(#20685,#20686),(#20687,#20688),(#20689,#20690),(#20691,#20692),
(#20693,#20694),(#20695,#20696),(#20697,#20698),(#20699,#20700),(#20701,
#20702),(#20703,#20704),(#20705,#20706),(#20707,#20708),(#20709,#20710),
(#20711,#20712),(#20713,#20714),(#20715,#20716),(#20717,#20718),(#20719,
#20720),(#20721,#20722),(#20723,#20724),(#20725,#20726),(#20727,#20728),
(#20729,#20730),(#20731,#20732),(#20733,#20734),(#20735,#20736),(#20737,
#20738),(#20739,#20740),(#20741,#20742),(#20743,#20744),(#20745,#20746),
(#20747,#20748),(#20749,#20750),(#20751,#20752),(#20753,#20754),(#20755,
#20756),(#20757,#20758),(#20759,#20760),(#20761,#20762),(#20763,#20764),
(#20765,#20766)),.UNSPECIFIED.,.F.,.F.,.F.,(6,1,1,1,1,1,1,1,1,1,1,1,1,1,
1,1,1,1,1,1,1,1,1,1,1,1,1,1,1,1,1,1,1,1,1,1,1,1,1,1,1,1,1,1,1,1,1,1,1,1,
1,1,1,1,1,1,1,1,1,1,1,1,1,1,1,1,1,1,1,1,6),(2,2),(-1.,-0.985714285714284,
-0.97142857142857,-0.957142857142856,-0.942857142857141,-0.928571428571427,
-0.914285714285713,-0.899999999999999,-0.885714285714284,-0.87142857142857,
-0.857142857142856,-0.842857142857142,-0.828571428571428,-0.814285714285713,
-0.799999999999999,-0.785714285714285,-0.771428571428571,-0.757142857142856,
-0.742857142857142,-0.728571428571428,-0.714285714285714,-0.699999999999999,
-0.685714285714285,-0.671428571428571,-0.657142857142857,-0.642857142857142,
-0.628571428571428,-0.614285714285714,-0.6,-0.585714285714286,-0.571428571428571,
-0.557142857142857,-0.542857142857143,-0.528571428571429,-0.514285714285714,
-0.5,-0.485714285714286,-0.471428571428572,-0.457142857142857,-0.442857142857143,
-0.428571428571429,-0.414285714285714,-0.4,-0.385714285714286,-0.371428571428571,
-0.357142857142857,-0.342857142857143,-0.328571428571429,-0.314285714285714,
-0.3,-0.285714285714286,-0.271428571428571,-0.257142857142857,-0.242857142857143,
-0.228571428571429,-0.214285714285714,-0.2,-0.185714285714286,-0.171428571428571,
-0.157142857142857,-0.142857142857143,-0.128571428571429,-0.114285714285714,
-0.1,-0.0857142857142857,-0.0714285714285714,-0.0571428571428571,-0.0428571428571429,
-0.0285714285714286,-0.0142857142857143,0.),(0.,1.8),.UNSPECIFIED.);
#952=B_SPLINE_SURFACE_WITH_KNOTS('',5,1,((#20925,#20926),(#20927,#20928),
(#20929,#20930),(#20931,#20932),(#20933,#20934),(#20935,#20936),(#20937,
#20938),(#20939,#20940),(#20941,#20942),(#20943,#20944),(#20945,#20946),
(#20947,#20948),(#20949,#20950),(#20951,#20952),(#20953,#20954),(#20955,
#20956),(#20957,#20958),(#20959,#20960),(#20961,#20962),(#20963,#20964),
(#20965,#20966),(#20967,#20968),(#20969,#20970),(#20971,#20972),(#20973,
#20974),(#20975,#20976),(#20977,#20978),(#20979,#20980),(#20981,#20982),
(#20983,#20984),(#20985,#20986),(#20987,#20988),(#20989,#20990),(#20991,
#20992),(#20993,#20994),(#20995,#20996),(#20997,#20998),(#20999,#21000),
(#21001,#21002),(#21003,#21004),(#21005,#21006),(#21007,#21008),(#21009,
#21010),(#21011,#21012),(#21013,#21014),(#21015,#21016),(#21017,#21018),
(#21019,#21020),(#21021,#21022),(#21023,#21024),(#21025,#21026),(#21027,
#21028),(#21029,#21030),(#21031,#21032),(#21033,#21034),(#21035,#21036),
(#21037,#21038),(#21039,#21040),(#21041,#21042),(#21043,#21044),(#21045,
#21046),(#21047,#21048),(#21049,#21050),(#21051,#21052),(#21053,#21054),
(#21055,#21056),(#21057,#21058),(#21059,#21060),(#21061,#21062),(#21063,
#21064),(#21065,#21066),(#21067,#21068),(#21069,#21070),(#21071,#21072),
(#21073,#21074)),.UNSPECIFIED.,.F.,.F.,.F.,(6,1,1,1,1,1,1,1,1,1,1,1,1,1,
1,1,1,1,1,1,1,1,1,1,1,1,1,1,1,1,1,1,1,1,1,1,1,1,1,1,1,1,1,1,1,1,1,1,1,1,
1,1,1,1,1,1,1,1,1,1,1,1,1,1,1,1,1,1,1,1,6),(2,2),(0.,0.0142857142857143,
0.0285714285714286,0.0428571428571429,0.0571428571428571,0.0714285714285714,
0.0857142857142857,0.1,0.114285714285714,0.128571428571429,0.142857142857143,
0.157142857142857,0.171428571428571,0.185714285714286,0.2,0.214285714285714,
0.228571428571429,0.242857142857143,0.257142857142857,0.271428571428571,
0.285714285714286,0.3,0.314285714285714,0.328571428571429,0.342857142857143,
0.357142857142857,0.371428571428571,0.385714285714286,0.4,0.414285714285714,
0.428571428571429,0.442857142857143,0.457142857142857,0.471428571428572,
0.485714285714286,0.5,0.514285714285714,0.528571428571429,0.542857142857143,
0.557142857142857,0.571428571428571,0.585714285714286,0.6,0.614285714285714,
0.628571428571428,0.642857142857142,0.657142857142857,0.671428571428571,
0.685714285714285,0.699999999999999,0.714285714285714,0.728571428571428,
0.742857142857142,0.757142857142856,0.771428571428571,0.785714285714285,
0.799999999999999,0.814285714285713,0.828571428571428,0.842857142857142,
0.857142857142856,0.87142857142857,0.885714285714284,0.899999999999999,
0.914285714285713,0.928571428571427,0.942857142857141,0.957142857142856,
0.97142857142857,0.985714285714284,1.),(0.,1.8),.UNSPECIFIED.);
#953=B_SPLINE_SURFACE_WITH_KNOTS('',5,1,((#21223,#21224),(#21225,#21226),
(#21227,#21228),(#21229,#21230),(#21231,#21232),(#21233,#21234),(#21235,
#21236),(#21237,#21238),(#21239,#21240),(#21241,#21242),(#21243,#21244),
(#21245,#21246),(#21247,#21248),(#21249,#21250),(#21251,#21252),(#21253,
#21254),(#21255,#21256),(#21257,#21258),(#21259,#21260),(#21261,#21262),
(#21263,#21264),(#21265,#21266),(#21267,#21268),(#21269,#21270),(#21271,
#21272),(#21273,#21274),(#21275,#21276),(#21277,#21278),(#21279,#21280),
(#21281,#21282),(#21283,#21284),(#21285,#21286),(#21287,#21288),(#21289,
#21290),(#21291,#21292),(#21293,#21294),(#21295,#21296),(#21297,#21298),
(#21299,#21300),(#21301,#21302),(#21303,#21304),(#21305,#21306),(#21307,
#21308),(#21309,#21310),(#21311,#21312),(#21313,#21314),(#21315,#21316),
(#21317,#21318),(#21319,#21320),(#21321,#21322),(#21323,#21324),(#21325,
#21326),(#21327,#21328),(#21329,#21330),(#21331,#21332),(#21333,#21334),
(#21335,#21336),(#21337,#21338),(#21339,#21340),(#21341,#21342),(#21343,
#21344),(#21345,#21346),(#21347,#21348),(#21349,#21350),(#21351,#21352),
(#21353,#21354),(#21355,#21356),(#21357,#21358),(#21359,#21360),(#21361,
#21362),(#21363,#21364),(#21365,#21366),(#21367,#21368),(#21369,#21370),
(#21371,#21372)),.UNSPECIFIED.,.F.,.F.,.F.,(6,1,1,1,1,1,1,1,1,1,1,1,1,1,
1,1,1,1,1,1,1,1,1,1,1,1,1,1,1,1,1,1,1,1,1,1,1,1,1,1,1,1,1,1,1,1,1,1,1,1,
1,1,1,1,1,1,1,1,1,1,1,1,1,1,1,1,1,1,1,1,6),(2,2),(-1.,-0.985714285714284,
-0.97142857142857,-0.957142857142856,-0.942857142857141,-0.928571428571427,
-0.914285714285713,-0.899999999999999,-0.885714285714284,-0.87142857142857,
-0.857142857142856,-0.842857142857142,-0.828571428571428,-0.814285714285713,
-0.799999999999999,-0.785714285714285,-0.771428571428571,-0.757142857142856,
-0.742857142857142,-0.728571428571428,-0.714285714285714,-0.699999999999999,
-0.685714285714285,-0.671428571428571,-0.657142857142857,-0.642857142857142,
-0.628571428571428,-0.614285714285714,-0.6,-0.585714285714286,-0.571428571428571,
-0.557142857142857,-0.542857142857143,-0.528571428571429,-0.514285714285714,
-0.5,-0.485714285714286,-0.471428571428572,-0.457142857142857,-0.442857142857143,
-0.428571428571429,-0.414285714285714,-0.4,-0.385714285714286,-0.371428571428571,
-0.357142857142857,-0.342857142857143,-0.328571428571429,-0.314285714285714,
-0.3,-0.285714285714286,-0.271428571428571,-0.257142857142857,-0.242857142857143,
-0.228571428571429,-0.214285714285714,-0.2,-0.185714285714286,-0.171428571428571,
-0.157142857142857,-0.142857142857143,-0.128571428571429,-0.114285714285714,
-0.1,-0.0857142857142857,-0.0714285714285714,-0.0571428571428571,-0.0428571428571429,
-0.0285714285714286,-0.0142857142857143,0.),(0.,1.8),.UNSPECIFIED.);
#954=B_SPLINE_SURFACE_WITH_KNOTS('',5,1,((#21531,#21532),(#21533,#21534),
(#21535,#21536),(#21537,#21538),(#21539,#21540),(#21541,#21542),(#21543,
#21544),(#21545,#21546),(#21547,#21548),(#21549,#21550),(#21551,#21552),
(#21553,#21554),(#21555,#21556),(#21557,#21558),(#21559,#21560),(#21561,
#21562),(#21563,#21564),(#21565,#21566),(#21567,#21568),(#21569,#21570),
(#21571,#21572),(#21573,#21574),(#21575,#21576),(#21577,#21578),(#21579,
#21580),(#21581,#21582),(#21583,#21584),(#21585,#21586),(#21587,#21588),
(#21589,#21590),(#21591,#21592),(#21593,#21594),(#21595,#21596),(#21597,
#21598),(#21599,#21600),(#21601,#21602),(#21603,#21604),(#21605,#21606),
(#21607,#21608),(#21609,#21610),(#21611,#21612),(#21613,#21614),(#21615,
#21616),(#21617,#21618),(#21619,#21620),(#21621,#21622),(#21623,#21624),
(#21625,#21626),(#21627,#21628),(#21629,#21630),(#21631,#21632),(#21633,
#21634),(#21635,#21636),(#21637,#21638),(#21639,#21640),(#21641,#21642),
(#21643,#21644),(#21645,#21646),(#21647,#21648),(#21649,#21650),(#21651,
#21652),(#21653,#21654),(#21655,#21656),(#21657,#21658),(#21659,#21660),
(#21661,#21662),(#21663,#21664),(#21665,#21666),(#21667,#21668),(#21669,
#21670),(#21671,#21672),(#21673,#21674),(#21675,#21676),(#21677,#21678),
(#21679,#21680)),.UNSPECIFIED.,.F.,.F.,.F.,(6,1,1,1,1,1,1,1,1,1,1,1,1,1,
1,1,1,1,1,1,1,1,1,1,1,1,1,1,1,1,1,1,1,1,1,1,1,1,1,1,1,1,1,1,1,1,1,1,1,1,
1,1,1,1,1,1,1,1,1,1,1,1,1,1,1,1,1,1,1,1,6),(2,2),(0.,0.0142857142857143,
0.0285714285714286,0.0428571428571429,0.0571428571428571,0.0714285714285714,
0.0857142857142857,0.1,0.114285714285714,0.128571428571429,0.142857142857143,
0.157142857142857,0.171428571428571,0.185714285714286,0.2,0.214285714285714,
0.228571428571429,0.242857142857143,0.257142857142857,0.271428571428571,
0.285714285714286,0.3,0.314285714285714,0.328571428571429,0.342857142857143,
0.357142857142857,0.371428571428571,0.385714285714286,0.4,0.414285714285714,
0.428571428571429,0.442857142857143,0.457142857142857,0.471428571428572,
0.485714285714286,0.5,0.514285714285714,0.528571428571429,0.542857142857143,
0.557142857142857,0.571428571428571,0.585714285714286,0.6,0.614285714285714,
0.628571428571428,0.642857142857142,0.657142857142857,0.671428571428571,
0.685714285714285,0.699999999999999,0.714285714285714,0.728571428571428,
0.742857142857142,0.757142857142856,0.771428571428571,0.785714285714285,
0.799999999999999,0.814285714285713,0.828571428571428,0.842857142857142,
0.857142857142856,0.87142857142857,0.885714285714284,0.899999999999999,
0.914285714285713,0.928571428571427,0.942857142857141,0.957142857142856,
0.97142857142857,0.985714285714284,1.),(0.,1.8),.UNSPECIFIED.);
#955=B_SPLINE_SURFACE_WITH_KNOTS('',5,1,((#21829,#21830),(#21831,#21832),
(#21833,#21834),(#21835,#21836),(#21837,#21838),(#21839,#21840),(#21841,
#21842),(#21843,#21844),(#21845,#21846),(#21847,#21848),(#21849,#21850),
(#21851,#21852),(#21853,#21854),(#21855,#21856),(#21857,#21858),(#21859,
#21860),(#21861,#21862),(#21863,#21864),(#21865,#21866),(#21867,#21868),
(#21869,#21870),(#21871,#21872),(#21873,#21874),(#21875,#21876),(#21877,
#21878),(#21879,#21880),(#21881,#21882),(#21883,#21884),(#21885,#21886),
(#21887,#21888),(#21889,#21890),(#21891,#21892),(#21893,#21894),(#21895,
#21896),(#21897,#21898),(#21899,#21900),(#21901,#21902),(#21903,#21904),
(#21905,#21906),(#21907,#21908),(#21909,#21910),(#21911,#21912),(#21913,
#21914),(#21915,#21916),(#21917,#21918),(#21919,#21920),(#21921,#21922),
(#21923,#21924),(#21925,#21926),(#21927,#21928),(#21929,#21930),(#21931,
#21932),(#21933,#21934),(#21935,#21936),(#21937,#21938),(#21939,#21940),
(#21941,#21942),(#21943,#21944),(#21945,#21946),(#21947,#21948),(#21949,
#21950),(#21951,#21952),(#21953,#21954),(#21955,#21956),(#21957,#21958),
(#21959,#21960),(#21961,#21962),(#21963,#21964),(#21965,#21966),(#21967,
#21968),(#21969,#21970),(#21971,#21972),(#21973,#21974),(#21975,#21976),
(#21977,#21978)),.UNSPECIFIED.,.F.,.F.,.F.,(6,1,1,1,1,1,1,1,1,1,1,1,1,1,
1,1,1,1,1,1,1,1,1,1,1,1,1,1,1,1,1,1,1,1,1,1,1,1,1,1,1,1,1,1,1,1,1,1,1,1,
1,1,1,1,1,1,1,1,1,1,1,1,1,1,1,1,1,1,1,1,6),(2,2),(-1.,-0.985714285714284,
-0.97142857142857,-0.957142857142856,-0.942857142857141,-0.928571428571427,
-0.914285714285713,-0.899999999999999,-0.885714285714284,-0.87142857142857,
-0.857142857142856,-0.842857142857142,-0.828571428571428,-0.814285714285713,
-0.799999999999999,-0.785714285714285,-0.771428571428571,-0.757142857142856,
-0.742857142857142,-0.728571428571428,-0.714285714285714,-0.699999999999999,
-0.685714285714285,-0.671428571428571,-0.657142857142857,-0.642857142857142,
-0.628571428571428,-0.614285714285714,-0.6,-0.585714285714286,-0.571428571428571,
-0.557142857142857,-0.542857142857143,-0.528571428571429,-0.514285714285714,
-0.5,-0.485714285714286,-0.471428571428572,-0.457142857142857,-0.442857142857143,
-0.428571428571429,-0.414285714285714,-0.4,-0.385714285714286,-0.371428571428571,
-0.357142857142857,-0.342857142857143,-0.328571428571429,-0.314285714285714,
-0.3,-0.285714285714286,-0.271428571428571,-0.257142857142857,-0.242857142857143,
-0.228571428571429,-0.214285714285714,-0.2,-0.185714285714286,-0.171428571428571,
-0.157142857142857,-0.142857142857143,-0.128571428571429,-0.114285714285714,
-0.1,-0.0857142857142857,-0.0714285714285714,-0.0571428571428571,-0.0428571428571429,
-0.0285714285714286,-0.0142857142857143,0.),(0.,1.8),.UNSPECIFIED.);
#956=B_SPLINE_SURFACE_WITH_KNOTS('',5,1,((#22137,#22138),(#22139,#22140),
(#22141,#22142),(#22143,#22144),(#22145,#22146),(#22147,#22148),(#22149,
#22150),(#22151,#22152),(#22153,#22154),(#22155,#22156),(#22157,#22158),
(#22159,#22160),(#22161,#22162),(#22163,#22164),(#22165,#22166),(#22167,
#22168),(#22169,#22170),(#22171,#22172),(#22173,#22174),(#22175,#22176),
(#22177,#22178),(#22179,#22180),(#22181,#22182),(#22183,#22184),(#22185,
#22186),(#22187,#22188),(#22189,#22190),(#22191,#22192),(#22193,#22194),
(#22195,#22196),(#22197,#22198),(#22199,#22200),(#22201,#22202),(#22203,
#22204),(#22205,#22206),(#22207,#22208),(#22209,#22210),(#22211,#22212),
(#22213,#22214),(#22215,#22216),(#22217,#22218),(#22219,#22220),(#22221,
#22222),(#22223,#22224),(#22225,#22226),(#22227,#22228),(#22229,#22230),
(#22231,#22232),(#22233,#22234),(#22235,#22236),(#22237,#22238),(#22239,
#22240),(#22241,#22242),(#22243,#22244),(#22245,#22246),(#22247,#22248),
(#22249,#22250),(#22251,#22252),(#22253,#22254),(#22255,#22256),(#22257,
#22258),(#22259,#22260),(#22261,#22262),(#22263,#22264),(#22265,#22266),
(#22267,#22268),(#22269,#22270),(#22271,#22272),(#22273,#22274),(#22275,
#22276),(#22277,#22278),(#22279,#22280),(#22281,#22282),(#22283,#22284),
(#22285,#22286)),.UNSPECIFIED.,.F.,.F.,.F.,(6,1,1,1,1,1,1,1,1,1,1,1,1,1,
1,1,1,1,1,1,1,1,1,1,1,1,1,1,1,1,1,1,1,1,1,1,1,1,1,1,1,1,1,1,1,1,1,1,1,1,
1,1,1,1,1,1,1,1,1,1,1,1,1,1,1,1,1,1,1,1,6),(2,2),(0.,0.0142857142857143,
0.0285714285714286,0.0428571428571429,0.0571428571428571,0.0714285714285714,
0.0857142857142857,0.1,0.114285714285714,0.128571428571429,0.142857142857143,
0.157142857142857,0.171428571428571,0.185714285714286,0.2,0.214285714285714,
0.228571428571429,0.242857142857143,0.257142857142857,0.271428571428571,
0.285714285714286,0.3,0.314285714285714,0.328571428571429,0.342857142857143,
0.357142857142857,0.371428571428571,0.385714285714286,0.4,0.414285714285714,
0.428571428571429,0.442857142857143,0.457142857142857,0.471428571428572,
0.485714285714286,0.5,0.514285714285714,0.528571428571429,0.542857142857143,
0.557142857142857,0.571428571428571,0.585714285714286,0.6,0.614285714285714,
0.628571428571428,0.642857142857142,0.657142857142857,0.671428571428571,
0.685714285714285,0.699999999999999,0.714285714285714,0.728571428571428,
0.742857142857142,0.757142857142856,0.771428571428571,0.785714285714285,
0.799999999999999,0.814285714285713,0.828571428571428,0.842857142857142,
0.857142857142856,0.87142857142857,0.885714285714284,0.899999999999999,
0.914285714285713,0.928571428571427,0.942857142857141,0.957142857142856,
0.97142857142857,0.985714285714284,1.),(0.,1.8),.UNSPECIFIED.);
#957=B_SPLINE_SURFACE_WITH_KNOTS('',5,1,((#22435,#22436),(#22437,#22438),
(#22439,#22440),(#22441,#22442),(#22443,#22444),(#22445,#22446),(#22447,
#22448),(#22449,#22450),(#22451,#22452),(#22453,#22454),(#22455,#22456),
(#22457,#22458),(#22459,#22460),(#22461,#22462),(#22463,#22464),(#22465,
#22466),(#22467,#22468),(#22469,#22470),(#22471,#22472),(#22473,#22474),
(#22475,#22476),(#22477,#22478),(#22479,#22480),(#22481,#22482),(#22483,
#22484),(#22485,#22486),(#22487,#22488),(#22489,#22490),(#22491,#22492),
(#22493,#22494),(#22495,#22496),(#22497,#22498),(#22499,#22500),(#22501,
#22502),(#22503,#22504),(#22505,#22506),(#22507,#22508),(#22509,#22510),
(#22511,#22512),(#22513,#22514),(#22515,#22516),(#22517,#22518),(#22519,
#22520),(#22521,#22522),(#22523,#22524),(#22525,#22526),(#22527,#22528),
(#22529,#22530),(#22531,#22532),(#22533,#22534),(#22535,#22536),(#22537,
#22538),(#22539,#22540),(#22541,#22542),(#22543,#22544),(#22545,#22546),
(#22547,#22548),(#22549,#22550),(#22551,#22552),(#22553,#22554),(#22555,
#22556),(#22557,#22558),(#22559,#22560),(#22561,#22562),(#22563,#22564),
(#22565,#22566),(#22567,#22568),(#22569,#22570),(#22571,#22572),(#22573,
#22574),(#22575,#22576),(#22577,#22578),(#22579,#22580),(#22581,#22582),
(#22583,#22584)),.UNSPECIFIED.,.F.,.F.,.F.,(6,1,1,1,1,1,1,1,1,1,1,1,1,1,
1,1,1,1,1,1,1,1,1,1,1,1,1,1,1,1,1,1,1,1,1,1,1,1,1,1,1,1,1,1,1,1,1,1,1,1,
1,1,1,1,1,1,1,1,1,1,1,1,1,1,1,1,1,1,1,1,6),(2,2),(-1.,-0.985714285714284,
-0.97142857142857,-0.957142857142856,-0.942857142857141,-0.928571428571427,
-0.914285714285713,-0.899999999999999,-0.885714285714284,-0.87142857142857,
-0.857142857142856,-0.842857142857142,-0.828571428571428,-0.814285714285713,
-0.799999999999999,-0.785714285714285,-0.771428571428571,-0.757142857142856,
-0.742857142857142,-0.728571428571428,-0.714285714285714,-0.699999999999999,
-0.685714285714285,-0.671428571428571,-0.657142857142857,-0.642857142857142,
-0.628571428571428,-0.614285714285714,-0.6,-0.585714285714286,-0.571428571428571,
-0.557142857142857,-0.542857142857143,-0.528571428571429,-0.514285714285714,
-0.5,-0.485714285714286,-0.471428571428572,-0.457142857142857,-0.442857142857143,
-0.428571428571429,-0.414285714285714,-0.4,-0.385714285714286,-0.371428571428571,
-0.357142857142857,-0.342857142857143,-0.328571428571429,-0.314285714285714,
-0.3,-0.285714285714286,-0.271428571428571,-0.257142857142857,-0.242857142857143,
-0.228571428571429,-0.214285714285714,-0.2,-0.185714285714286,-0.171428571428571,
-0.157142857142857,-0.142857142857143,-0.128571428571429,-0.114285714285714,
-0.1,-0.0857142857142857,-0.0714285714285714,-0.0571428571428571,-0.0428571428571429,
-0.0285714285714286,-0.0142857142857143,0.),(0.,1.8),.UNSPECIFIED.);
#958=B_SPLINE_SURFACE_WITH_KNOTS('',5,1,((#22743,#22744),(#22745,#22746),
(#22747,#22748),(#22749,#22750),(#22751,#22752),(#22753,#22754),(#22755,
#22756),(#22757,#22758),(#22759,#22760),(#22761,#22762),(#22763,#22764),
(#22765,#22766),(#22767,#22768),(#22769,#22770),(#22771,#22772),(#22773,
#22774),(#22775,#22776),(#22777,#22778),(#22779,#22780),(#22781,#22782),
(#22783,#22784),(#22785,#22786),(#22787,#22788),(#22789,#22790),(#22791,
#22792),(#22793,#22794),(#22795,#22796),(#22797,#22798),(#22799,#22800),
(#22801,#22802),(#22803,#22804),(#22805,#22806),(#22807,#22808),(#22809,
#22810),(#22811,#22812),(#22813,#22814),(#22815,#22816),(#22817,#22818),
(#22819,#22820),(#22821,#22822),(#22823,#22824),(#22825,#22826),(#22827,
#22828),(#22829,#22830),(#22831,#22832),(#22833,#22834),(#22835,#22836),
(#22837,#22838),(#22839,#22840),(#22841,#22842),(#22843,#22844),(#22845,
#22846),(#22847,#22848),(#22849,#22850),(#22851,#22852),(#22853,#22854),
(#22855,#22856),(#22857,#22858),(#22859,#22860),(#22861,#22862),(#22863,
#22864),(#22865,#22866),(#22867,#22868),(#22869,#22870),(#22871,#22872),
(#22873,#22874),(#22875,#22876),(#22877,#22878),(#22879,#22880),(#22881,
#22882),(#22883,#22884),(#22885,#22886),(#22887,#22888),(#22889,#22890),
(#22891,#22892)),.UNSPECIFIED.,.F.,.F.,.F.,(6,1,1,1,1,1,1,1,1,1,1,1,1,1,
1,1,1,1,1,1,1,1,1,1,1,1,1,1,1,1,1,1,1,1,1,1,1,1,1,1,1,1,1,1,1,1,1,1,1,1,
1,1,1,1,1,1,1,1,1,1,1,1,1,1,1,1,1,1,1,1,6),(2,2),(0.,0.0142857142857143,
0.0285714285714286,0.0428571428571429,0.0571428571428571,0.0714285714285714,
0.0857142857142857,0.1,0.114285714285714,0.128571428571429,0.142857142857143,
0.157142857142857,0.171428571428571,0.185714285714286,0.2,0.214285714285714,
0.228571428571429,0.242857142857143,0.257142857142857,0.271428571428571,
0.285714285714286,0.3,0.314285714285714,0.328571428571429,0.342857142857143,
0.357142857142857,0.371428571428571,0.385714285714286,0.4,0.414285714285714,
0.428571428571429,0.442857142857143,0.457142857142857,0.471428571428572,
0.485714285714286,0.5,0.514285714285714,0.528571428571429,0.542857142857143,
0.557142857142857,0.571428571428571,0.585714285714286,0.6,0.614285714285714,
0.628571428571428,0.642857142857142,0.657142857142857,0.671428571428571,
0.685714285714285,0.699999999999999,0.714285714285714,0.728571428571428,
0.742857142857142,0.757142857142856,0.771428571428571,0.785714285714285,
0.799999999999999,0.814285714285713,0.828571428571428,0.842857142857142,
0.857142857142856,0.87142857142857,0.885714285714284,0.899999999999999,
0.914285714285713,0.928571428571427,0.942857142857141,0.957142857142856,
0.97142857142857,0.985714285714284,1.),(0.,1.8),.UNSPECIFIED.);
#959=B_SPLINE_SURFACE_WITH_KNOTS('',5,1,((#23041,#23042),(#23043,#23044),
(#23045,#23046),(#23047,#23048),(#23049,#23050),(#23051,#23052),(#23053,
#23054),(#23055,#23056),(#23057,#23058),(#23059,#23060),(#23061,#23062),
(#23063,#23064),(#23065,#23066),(#23067,#23068),(#23069,#23070),(#23071,
#23072),(#23073,#23074),(#23075,#23076),(#23077,#23078),(#23079,#23080),
(#23081,#23082),(#23083,#23084),(#23085,#23086),(#23087,#23088),(#23089,
#23090),(#23091,#23092),(#23093,#23094),(#23095,#23096),(#23097,#23098),
(#23099,#23100),(#23101,#23102),(#23103,#23104),(#23105,#23106),(#23107,
#23108),(#23109,#23110),(#23111,#23112),(#23113,#23114),(#23115,#23116),
(#23117,#23118),(#23119,#23120),(#23121,#23122),(#23123,#23124),(#23125,
#23126),(#23127,#23128),(#23129,#23130),(#23131,#23132),(#23133,#23134),
(#23135,#23136),(#23137,#23138),(#23139,#23140),(#23141,#23142),(#23143,
#23144),(#23145,#23146),(#23147,#23148),(#23149,#23150),(#23151,#23152),
(#23153,#23154),(#23155,#23156),(#23157,#23158),(#23159,#23160),(#23161,
#23162),(#23163,#23164),(#23165,#23166),(#23167,#23168),(#23169,#23170),
(#23171,#23172),(#23173,#23174),(#23175,#23176),(#23177,#23178),(#23179,
#23180),(#23181,#23182),(#23183,#23184),(#23185,#23186),(#23187,#23188),
(#23189,#23190)),.UNSPECIFIED.,.F.,.F.,.F.,(6,1,1,1,1,1,1,1,1,1,1,1,1,1,
1,1,1,1,1,1,1,1,1,1,1,1,1,1,1,1,1,1,1,1,1,1,1,1,1,1,1,1,1,1,1,1,1,1,1,1,
1,1,1,1,1,1,1,1,1,1,1,1,1,1,1,1,1,1,1,1,6),(2,2),(-1.,-0.985714285714284,
-0.97142857142857,-0.957142857142856,-0.942857142857141,-0.928571428571427,
-0.914285714285713,-0.899999999999999,-0.885714285714284,-0.87142857142857,
-0.857142857142856,-0.842857142857142,-0.828571428571428,-0.814285714285713,
-0.799999999999999,-0.785714285714285,-0.771428571428571,-0.757142857142856,
-0.742857142857142,-0.728571428571428,-0.714285714285714,-0.699999999999999,
-0.685714285714285,-0.671428571428571,-0.657142857142857,-0.642857142857142,
-0.628571428571428,-0.614285714285714,-0.6,-0.585714285714286,-0.571428571428571,
-0.557142857142857,-0.542857142857143,-0.528571428571429,-0.514285714285714,
-0.5,-0.485714285714286,-0.471428571428572,-0.457142857142857,-0.442857142857143,
-0.428571428571429,-0.414285714285714,-0.4,-0.385714285714286,-0.371428571428571,
-0.357142857142857,-0.342857142857143,-0.328571428571429,-0.314285714285714,
-0.3,-0.285714285714286,-0.271428571428571,-0.257142857142857,-0.242857142857143,
-0.228571428571429,-0.214285714285714,-0.2,-0.185714285714286,-0.171428571428571,
-0.157142857142857,-0.142857142857143,-0.128571428571429,-0.114285714285714,
-0.1,-0.0857142857142857,-0.0714285714285714,-0.0571428571428571,-0.0428571428571429,
-0.0285714285714286,-0.0142857142857143,0.),(0.,1.8),.UNSPECIFIED.);
#960=B_SPLINE_SURFACE_WITH_KNOTS('',5,1,((#23349,#23350),(#23351,#23352),
(#23353,#23354),(#23355,#23356),(#23357,#23358),(#23359,#23360),(#23361,
#23362),(#23363,#23364),(#23365,#23366),(#23367,#23368),(#23369,#23370),
(#23371,#23372),(#23373,#23374),(#23375,#23376),(#23377,#23378),(#23379,
#23380),(#23381,#23382),(#23383,#23384),(#23385,#23386),(#23387,#23388),
(#23389,#23390),(#23391,#23392),(#23393,#23394),(#23395,#23396),(#23397,
#23398),(#23399,#23400),(#23401,#23402),(#23403,#23404),(#23405,#23406),
(#23407,#23408),(#23409,#23410),(#23411,#23412),(#23413,#23414),(#23415,
#23416),(#23417,#23418),(#23419,#23420),(#23421,#23422),(#23423,#23424),
(#23425,#23426),(#23427,#23428),(#23429,#23430),(#23431,#23432),(#23433,
#23434),(#23435,#23436),(#23437,#23438),(#23439,#23440),(#23441,#23442),
(#23443,#23444),(#23445,#23446),(#23447,#23448),(#23449,#23450),(#23451,
#23452),(#23453,#23454),(#23455,#23456),(#23457,#23458),(#23459,#23460),
(#23461,#23462),(#23463,#23464),(#23465,#23466),(#23467,#23468),(#23469,
#23470),(#23471,#23472),(#23473,#23474),(#23475,#23476),(#23477,#23478),
(#23479,#23480),(#23481,#23482),(#23483,#23484),(#23485,#23486),(#23487,
#23488),(#23489,#23490),(#23491,#23492),(#23493,#23494),(#23495,#23496),
(#23497,#23498)),.UNSPECIFIED.,.F.,.F.,.F.,(6,1,1,1,1,1,1,1,1,1,1,1,1,1,
1,1,1,1,1,1,1,1,1,1,1,1,1,1,1,1,1,1,1,1,1,1,1,1,1,1,1,1,1,1,1,1,1,1,1,1,
1,1,1,1,1,1,1,1,1,1,1,1,1,1,1,1,1,1,1,1,6),(2,2),(0.,0.0142857142857143,
0.0285714285714286,0.0428571428571429,0.0571428571428571,0.0714285714285714,
0.0857142857142857,0.1,0.114285714285714,0.128571428571429,0.142857142857143,
0.157142857142857,0.171428571428571,0.185714285714286,0.2,0.214285714285714,
0.228571428571429,0.242857142857143,0.257142857142857,0.271428571428571,
0.285714285714286,0.3,0.314285714285714,0.328571428571429,0.342857142857143,
0.357142857142857,0.371428571428571,0.385714285714286,0.4,0.414285714285714,
0.428571428571429,0.442857142857143,0.457142857142857,0.471428571428572,
0.485714285714286,0.5,0.514285714285714,0.528571428571429,0.542857142857143,
0.557142857142857,0.571428571428571,0.585714285714286,0.6,0.614285714285714,
0.628571428571428,0.642857142857142,0.657142857142857,0.671428571428571,
0.685714285714285,0.699999999999999,0.714285714285714,0.728571428571428,
0.742857142857142,0.757142857142856,0.771428571428571,0.785714285714285,
0.799999999999999,0.814285714285713,0.828571428571428,0.842857142857142,
0.857142857142856,0.87142857142857,0.885714285714284,0.899999999999999,
0.914285714285713,0.928571428571427,0.942857142857141,0.957142857142856,
0.97142857142857,0.985714285714284,1.),(0.,1.8),.UNSPECIFIED.);
#961=B_SPLINE_SURFACE_WITH_KNOTS('',5,1,((#23647,#23648),(#23649,#23650),
(#23651,#23652),(#23653,#23654),(#23655,#23656),(#23657,#23658),(#23659,
#23660),(#23661,#23662),(#23663,#23664),(#23665,#23666),(#23667,#23668),
(#23669,#23670),(#23671,#23672),(#23673,#23674),(#23675,#23676),(#23677,
#23678),(#23679,#23680),(#23681,#23682),(#23683,#23684),(#23685,#23686),
(#23687,#23688),(#23689,#23690),(#23691,#23692),(#23693,#23694),(#23695,
#23696),(#23697,#23698),(#23699,#23700),(#23701,#23702),(#23703,#23704),
(#23705,#23706),(#23707,#23708),(#23709,#23710),(#23711,#23712),(#23713,
#23714),(#23715,#23716),(#23717,#23718),(#23719,#23720),(#23721,#23722),
(#23723,#23724),(#23725,#23726),(#23727,#23728),(#23729,#23730),(#23731,
#23732),(#23733,#23734),(#23735,#23736),(#23737,#23738),(#23739,#23740),
(#23741,#23742),(#23743,#23744),(#23745,#23746),(#23747,#23748),(#23749,
#23750),(#23751,#23752),(#23753,#23754),(#23755,#23756),(#23757,#23758),
(#23759,#23760),(#23761,#23762),(#23763,#23764),(#23765,#23766),(#23767,
#23768),(#23769,#23770),(#23771,#23772),(#23773,#23774),(#23775,#23776),
(#23777,#23778),(#23779,#23780),(#23781,#23782),(#23783,#23784),(#23785,
#23786),(#23787,#23788),(#23789,#23790),(#23791,#23792),(#23793,#23794),
(#23795,#23796)),.UNSPECIFIED.,.F.,.F.,.F.,(6,1,1,1,1,1,1,1,1,1,1,1,1,1,
1,1,1,1,1,1,1,1,1,1,1,1,1,1,1,1,1,1,1,1,1,1,1,1,1,1,1,1,1,1,1,1,1,1,1,1,
1,1,1,1,1,1,1,1,1,1,1,1,1,1,1,1,1,1,1,1,6),(2,2),(-1.,-0.985714285714284,
-0.97142857142857,-0.957142857142856,-0.942857142857141,-0.928571428571427,
-0.914285714285713,-0.899999999999999,-0.885714285714284,-0.87142857142857,
-0.857142857142856,-0.842857142857142,-0.828571428571428,-0.814285714285713,
-0.799999999999999,-0.785714285714285,-0.771428571428571,-0.757142857142856,
-0.742857142857142,-0.728571428571428,-0.714285714285714,-0.699999999999999,
-0.685714285714285,-0.671428571428571,-0.657142857142857,-0.642857142857142,
-0.628571428571428,-0.614285714285714,-0.6,-0.585714285714286,-0.571428571428571,
-0.557142857142857,-0.542857142857143,-0.528571428571429,-0.514285714285714,
-0.5,-0.485714285714286,-0.471428571428572,-0.457142857142857,-0.442857142857143,
-0.428571428571429,-0.414285714285714,-0.4,-0.385714285714286,-0.371428571428571,
-0.357142857142857,-0.342857142857143,-0.328571428571429,-0.314285714285714,
-0.3,-0.285714285714286,-0.271428571428571,-0.257142857142857,-0.242857142857143,
-0.228571428571429,-0.214285714285714,-0.2,-0.185714285714286,-0.171428571428571,
-0.157142857142857,-0.142857142857143,-0.128571428571429,-0.114285714285714,
-0.1,-0.0857142857142857,-0.0714285714285714,-0.0571428571428571,-0.0428571428571429,
-0.0285714285714286,-0.0142857142857143,0.),(0.,1.8),.UNSPECIFIED.);
#962=B_SPLINE_SURFACE_WITH_KNOTS('',5,1,((#23955,#23956),(#23957,#23958),
(#23959,#23960),(#23961,#23962),(#23963,#23964),(#23965,#23966),(#23967,
#23968),(#23969,#23970),(#23971,#23972),(#23973,#23974),(#23975,#23976),
(#23977,#23978),(#23979,#23980),(#23981,#23982),(#23983,#23984),(#23985,
#23986),(#23987,#23988),(#23989,#23990),(#23991,#23992),(#23993,#23994),
(#23995,#23996),(#23997,#23998),(#23999,#24000),(#24001,#24002),(#24003,
#24004),(#24005,#24006),(#24007,#24008),(#24009,#24010),(#24011,#24012),
(#24013,#24014),(#24015,#24016),(#24017,#24018),(#24019,#24020),(#24021,
#24022),(#24023,#24024),(#24025,#24026),(#24027,#24028),(#24029,#24030),
(#24031,#24032),(#24033,#24034),(#24035,#24036),(#24037,#24038),(#24039,
#24040),(#24041,#24042),(#24043,#24044),(#24045,#24046),(#24047,#24048),
(#24049,#24050),(#24051,#24052),(#24053,#24054),(#24055,#24056),(#24057,
#24058),(#24059,#24060),(#24061,#24062),(#24063,#24064),(#24065,#24066),
(#24067,#24068),(#24069,#24070),(#24071,#24072),(#24073,#24074),(#24075,
#24076),(#24077,#24078),(#24079,#24080),(#24081,#24082),(#24083,#24084),
(#24085,#24086),(#24087,#24088),(#24089,#24090),(#24091,#24092),(#24093,
#24094),(#24095,#24096),(#24097,#24098),(#24099,#24100),(#24101,#24102),
(#24103,#24104)),.UNSPECIFIED.,.F.,.F.,.F.,(6,1,1,1,1,1,1,1,1,1,1,1,1,1,
1,1,1,1,1,1,1,1,1,1,1,1,1,1,1,1,1,1,1,1,1,1,1,1,1,1,1,1,1,1,1,1,1,1,1,1,
1,1,1,1,1,1,1,1,1,1,1,1,1,1,1,1,1,1,1,1,6),(2,2),(0.,0.0142857142857143,
0.0285714285714286,0.0428571428571429,0.0571428571428571,0.0714285714285714,
0.0857142857142857,0.1,0.114285714285714,0.128571428571429,0.142857142857143,
0.157142857142857,0.171428571428571,0.185714285714286,0.2,0.214285714285714,
0.228571428571429,0.242857142857143,0.257142857142857,0.271428571428571,
0.285714285714286,0.3,0.314285714285714,0.328571428571429,0.342857142857143,
0.357142857142857,0.371428571428571,0.385714285714286,0.4,0.414285714285714,
0.428571428571429,0.442857142857143,0.457142857142857,0.471428571428572,
0.485714285714286,0.5,0.514285714285714,0.528571428571429,0.542857142857143,
0.557142857142857,0.571428571428571,0.585714285714286,0.6,0.614285714285714,
0.628571428571428,0.642857142857142,0.657142857142857,0.671428571428571,
0.685714285714285,0.699999999999999,0.714285714285714,0.728571428571428,
0.742857142857142,0.757142857142856,0.771428571428571,0.785714285714285,
0.799999999999999,0.814285714285713,0.828571428571428,0.842857142857142,
0.857142857142856,0.87142857142857,0.885714285714284,0.899999999999999,
0.914285714285713,0.928571428571427,0.942857142857141,0.957142857142856,
0.97142857142857,0.985714285714284,1.),(0.,1.8),.UNSPECIFIED.);
#963=B_SPLINE_SURFACE_WITH_KNOTS('',5,1,((#24253,#24254),(#24255,#24256),
(#24257,#24258),(#24259,#24260),(#24261,#24262),(#24263,#24264),(#24265,
#24266),(#24267,#24268),(#24269,#24270),(#24271,#24272),(#24273,#24274),
(#24275,#24276),(#24277,#24278),(#24279,#24280),(#24281,#24282),(#24283,
#24284),(#24285,#24286),(#24287,#24288),(#24289,#24290),(#24291,#24292),
(#24293,#24294),(#24295,#24296),(#24297,#24298),(#24299,#24300),(#24301,
#24302),(#24303,#24304),(#24305,#24306),(#24307,#24308),(#24309,#24310),
(#24311,#24312),(#24313,#24314),(#24315,#24316),(#24317,#24318),(#24319,
#24320),(#24321,#24322),(#24323,#24324),(#24325,#24326),(#24327,#24328),
(#24329,#24330),(#24331,#24332),(#24333,#24334),(#24335,#24336),(#24337,
#24338),(#24339,#24340),(#24341,#24342),(#24343,#24344),(#24345,#24346),
(#24347,#24348),(#24349,#24350),(#24351,#24352),(#24353,#24354),(#24355,
#24356),(#24357,#24358),(#24359,#24360),(#24361,#24362),(#24363,#24364),
(#24365,#24366),(#24367,#24368),(#24369,#24370),(#24371,#24372),(#24373,
#24374),(#24375,#24376),(#24377,#24378),(#24379,#24380),(#24381,#24382),
(#24383,#24384),(#24385,#24386),(#24387,#24388),(#24389,#24390),(#24391,
#24392),(#24393,#24394),(#24395,#24396),(#24397,#24398),(#24399,#24400),
(#24401,#24402)),.UNSPECIFIED.,.F.,.F.,.F.,(6,1,1,1,1,1,1,1,1,1,1,1,1,1,
1,1,1,1,1,1,1,1,1,1,1,1,1,1,1,1,1,1,1,1,1,1,1,1,1,1,1,1,1,1,1,1,1,1,1,1,
1,1,1,1,1,1,1,1,1,1,1,1,1,1,1,1,1,1,1,1,6),(2,2),(-1.,-0.985714285714284,
-0.97142857142857,-0.957142857142856,-0.942857142857141,-0.928571428571427,
-0.914285714285713,-0.899999999999999,-0.885714285714284,-0.87142857142857,
-0.857142857142856,-0.842857142857142,-0.828571428571428,-0.814285714285713,
-0.799999999999999,-0.785714285714285,-0.771428571428571,-0.757142857142856,
-0.742857142857142,-0.728571428571428,-0.714285714285714,-0.699999999999999,
-0.685714285714285,-0.671428571428571,-0.657142857142857,-0.642857142857142,
-0.628571428571428,-0.614285714285714,-0.6,-0.585714285714286,-0.571428571428571,
-0.557142857142857,-0.542857142857143,-0.528571428571429,-0.514285714285714,
-0.5,-0.485714285714286,-0.471428571428572,-0.457142857142857,-0.442857142857143,
-0.428571428571429,-0.414285714285714,-0.4,-0.385714285714286,-0.371428571428571,
-0.357142857142857,-0.342857142857143,-0.328571428571429,-0.314285714285714,
-0.3,-0.285714285714286,-0.271428571428571,-0.257142857142857,-0.242857142857143,
-0.228571428571429,-0.214285714285714,-0.2,-0.185714285714286,-0.171428571428571,
-0.157142857142857,-0.142857142857143,-0.128571428571429,-0.114285714285714,
-0.1,-0.0857142857142857,-0.0714285714285714,-0.0571428571428571,-0.0428571428571429,
-0.0285714285714286,-0.0142857142857143,0.),(0.,1.8),.UNSPECIFIED.);
#964=B_SPLINE_SURFACE_WITH_KNOTS('',5,1,((#24561,#24562),(#24563,#24564),
(#24565,#24566),(#24567,#24568),(#24569,#24570),(#24571,#24572),(#24573,
#24574),(#24575,#24576),(#24577,#24578),(#24579,#24580),(#24581,#24582),
(#24583,#24584),(#24585,#24586),(#24587,#24588),(#24589,#24590),(#24591,
#24592),(#24593,#24594),(#24595,#24596),(#24597,#24598),(#24599,#24600),
(#24601,#24602),(#24603,#24604),(#24605,#24606),(#24607,#24608),(#24609,
#24610),(#24611,#24612),(#24613,#24614),(#24615,#24616),(#24617,#24618),
(#24619,#24620),(#24621,#24622),(#24623,#24624),(#24625,#24626),(#24627,
#24628),(#24629,#24630),(#24631,#24632),(#24633,#24634),(#24635,#24636),
(#24637,#24638),(#24639,#24640),(#24641,#24642),(#24643,#24644),(#24645,
#24646),(#24647,#24648),(#24649,#24650),(#24651,#24652),(#24653,#24654),
(#24655,#24656),(#24657,#24658),(#24659,#24660),(#24661,#24662),(#24663,
#24664),(#24665,#24666),(#24667,#24668),(#24669,#24670),(#24671,#24672),
(#24673,#24674),(#24675,#24676),(#24677,#24678),(#24679,#24680),(#24681,
#24682),(#24683,#24684),(#24685,#24686),(#24687,#24688),(#24689,#24690),
(#24691,#24692),(#24693,#24694),(#24695,#24696),(#24697,#24698),(#24699,
#24700),(#24701,#24702),(#24703,#24704),(#24705,#24706),(#24707,#24708),
(#24709,#24710)),.UNSPECIFIED.,.F.,.F.,.F.,(6,1,1,1,1,1,1,1,1,1,1,1,1,1,
1,1,1,1,1,1,1,1,1,1,1,1,1,1,1,1,1,1,1,1,1,1,1,1,1,1,1,1,1,1,1,1,1,1,1,1,
1,1,1,1,1,1,1,1,1,1,1,1,1,1,1,1,1,1,1,1,6),(2,2),(0.,0.0142857142857143,
0.0285714285714286,0.0428571428571429,0.0571428571428571,0.0714285714285714,
0.0857142857142857,0.1,0.114285714285714,0.128571428571429,0.142857142857143,
0.157142857142857,0.171428571428571,0.185714285714286,0.2,0.214285714285714,
0.228571428571429,0.242857142857143,0.257142857142857,0.271428571428571,
0.285714285714286,0.3,0.314285714285714,0.328571428571429,0.342857142857143,
0.357142857142857,0.371428571428571,0.385714285714286,0.4,0.414285714285714,
0.428571428571429,0.442857142857143,0.457142857142857,0.471428571428572,
0.485714285714286,0.5,0.514285714285714,0.528571428571429,0.542857142857143,
0.557142857142857,0.571428571428571,0.585714285714286,0.6,0.614285714285714,
0.628571428571428,0.642857142857142,0.657142857142857,0.671428571428571,
0.685714285714285,0.699999999999999,0.714285714285714,0.728571428571428,
0.742857142857142,0.757142857142856,0.771428571428571,0.785714285714285,
0.799999999999999,0.814285714285713,0.828571428571428,0.842857142857142,
0.857142857142856,0.87142857142857,0.885714285714284,0.899999999999999,
0.914285714285713,0.928571428571427,0.942857142857141,0.957142857142856,
0.97142857142857,0.985714285714284,1.),(0.,1.8),.UNSPECIFIED.);
#965=B_SPLINE_SURFACE_WITH_KNOTS('',5,1,((#24859,#24860),(#24861,#24862),
(#24863,#24864),(#24865,#24866),(#24867,#24868),(#24869,#24870),(#24871,
#24872),(#24873,#24874),(#24875,#24876),(#24877,#24878),(#24879,#24880),
(#24881,#24882),(#24883,#24884),(#24885,#24886),(#24887,#24888),(#24889,
#24890),(#24891,#24892),(#24893,#24894),(#24895,#24896),(#24897,#24898),
(#24899,#24900),(#24901,#24902),(#24903,#24904),(#24905,#24906),(#24907,
#24908),(#24909,#24910),(#24911,#24912),(#24913,#24914),(#24915,#24916),
(#24917,#24918),(#24919,#24920),(#24921,#24922),(#24923,#24924),(#24925,
#24926),(#24927,#24928),(#24929,#24930),(#24931,#24932),(#24933,#24934),
(#24935,#24936),(#24937,#24938),(#24939,#24940),(#24941,#24942),(#24943,
#24944),(#24945,#24946),(#24947,#24948),(#24949,#24950),(#24951,#24952),
(#24953,#24954),(#24955,#24956),(#24957,#24958),(#24959,#24960),(#24961,
#24962),(#24963,#24964),(#24965,#24966),(#24967,#24968),(#24969,#24970),
(#24971,#24972),(#24973,#24974),(#24975,#24976),(#24977,#24978),(#24979,
#24980),(#24981,#24982),(#24983,#24984),(#24985,#24986),(#24987,#24988),
(#24989,#24990),(#24991,#24992),(#24993,#24994),(#24995,#24996),(#24997,
#24998),(#24999,#25000),(#25001,#25002),(#25003,#25004),(#25005,#25006),
(#25007,#25008)),.UNSPECIFIED.,.F.,.F.,.F.,(6,1,1,1,1,1,1,1,1,1,1,1,1,1,
1,1,1,1,1,1,1,1,1,1,1,1,1,1,1,1,1,1,1,1,1,1,1,1,1,1,1,1,1,1,1,1,1,1,1,1,
1,1,1,1,1,1,1,1,1,1,1,1,1,1,1,1,1,1,1,1,6),(2,2),(-1.,-0.985714285714284,
-0.97142857142857,-0.957142857142856,-0.942857142857141,-0.928571428571427,
-0.914285714285713,-0.899999999999999,-0.885714285714284,-0.87142857142857,
-0.857142857142856,-0.842857142857142,-0.828571428571428,-0.814285714285713,
-0.799999999999999,-0.785714285714285,-0.771428571428571,-0.757142857142856,
-0.742857142857142,-0.728571428571428,-0.714285714285714,-0.699999999999999,
-0.685714285714285,-0.671428571428571,-0.657142857142857,-0.642857142857142,
-0.628571428571428,-0.614285714285714,-0.6,-0.585714285714286,-0.571428571428571,
-0.557142857142857,-0.542857142857143,-0.528571428571429,-0.514285714285714,
-0.5,-0.485714285714286,-0.471428571428572,-0.457142857142857,-0.442857142857143,
-0.428571428571429,-0.414285714285714,-0.4,-0.385714285714286,-0.371428571428571,
-0.357142857142857,-0.342857142857143,-0.328571428571429,-0.314285714285714,
-0.3,-0.285714285714286,-0.271428571428571,-0.257142857142857,-0.242857142857143,
-0.228571428571429,-0.214285714285714,-0.2,-0.185714285714286,-0.171428571428571,
-0.157142857142857,-0.142857142857143,-0.128571428571429,-0.114285714285714,
-0.1,-0.0857142857142857,-0.0714285714285714,-0.0571428571428571,-0.0428571428571429,
-0.0285714285714286,-0.0142857142857143,0.),(0.,1.8),.UNSPECIFIED.);
#966=B_SPLINE_SURFACE_WITH_KNOTS('',5,1,((#25167,#25168),(#25169,#25170),
(#25171,#25172),(#25173,#25174),(#25175,#25176),(#25177,#25178),(#25179,
#25180),(#25181,#25182),(#25183,#25184),(#25185,#25186),(#25187,#25188),
(#25189,#25190),(#25191,#25192),(#25193,#25194),(#25195,#25196),(#25197,
#25198),(#25199,#25200),(#25201,#25202),(#25203,#25204),(#25205,#25206),
(#25207,#25208),(#25209,#25210),(#25211,#25212),(#25213,#25214),(#25215,
#25216),(#25217,#25218),(#25219,#25220),(#25221,#25222),(#25223,#25224),
(#25225,#25226),(#25227,#25228),(#25229,#25230),(#25231,#25232),(#25233,
#25234),(#25235,#25236),(#25237,#25238),(#25239,#25240),(#25241,#25242),
(#25243,#25244),(#25245,#25246),(#25247,#25248),(#25249,#25250),(#25251,
#25252),(#25253,#25254),(#25255,#25256),(#25257,#25258),(#25259,#25260),
(#25261,#25262),(#25263,#25264),(#25265,#25266),(#25267,#25268),(#25269,
#25270),(#25271,#25272),(#25273,#25274),(#25275,#25276),(#25277,#25278),
(#25279,#25280),(#25281,#25282),(#25283,#25284),(#25285,#25286),(#25287,
#25288),(#25289,#25290),(#25291,#25292),(#25293,#25294),(#25295,#25296),
(#25297,#25298),(#25299,#25300),(#25301,#25302),(#25303,#25304),(#25305,
#25306),(#25307,#25308),(#25309,#25310),(#25311,#25312),(#25313,#25314),
(#25315,#25316)),.UNSPECIFIED.,.F.,.F.,.F.,(6,1,1,1,1,1,1,1,1,1,1,1,1,1,
1,1,1,1,1,1,1,1,1,1,1,1,1,1,1,1,1,1,1,1,1,1,1,1,1,1,1,1,1,1,1,1,1,1,1,1,
1,1,1,1,1,1,1,1,1,1,1,1,1,1,1,1,1,1,1,1,6),(2,2),(0.,0.0142857142857143,
0.0285714285714286,0.0428571428571429,0.0571428571428571,0.0714285714285714,
0.0857142857142857,0.1,0.114285714285714,0.128571428571429,0.142857142857143,
0.157142857142857,0.171428571428571,0.185714285714286,0.2,0.214285714285714,
0.228571428571429,0.242857142857143,0.257142857142857,0.271428571428571,
0.285714285714286,0.3,0.314285714285714,0.328571428571429,0.342857142857143,
0.357142857142857,0.371428571428571,0.385714285714286,0.4,0.414285714285714,
0.428571428571429,0.442857142857143,0.457142857142857,0.471428571428572,
0.485714285714286,0.5,0.514285714285714,0.528571428571429,0.542857142857143,
0.557142857142857,0.571428571428571,0.585714285714286,0.6,0.614285714285714,
0.628571428571428,0.642857142857142,0.657142857142857,0.671428571428571,
0.685714285714285,0.699999999999999,0.714285714285714,0.728571428571428,
0.742857142857142,0.757142857142856,0.771428571428571,0.785714285714285,
0.799999999999999,0.814285714285713,0.828571428571428,0.842857142857142,
0.857142857142856,0.87142857142857,0.885714285714284,0.899999999999999,
0.914285714285713,0.928571428571427,0.942857142857141,0.957142857142856,
0.97142857142857,0.985714285714284,1.),(0.,1.8),.UNSPECIFIED.);
#967=B_SPLINE_SURFACE_WITH_KNOTS('',5,1,((#25465,#25466),(#25467,#25468),
(#25469,#25470),(#25471,#25472),(#25473,#25474),(#25475,#25476),(#25477,
#25478),(#25479,#25480),(#25481,#25482),(#25483,#25484),(#25485,#25486),
(#25487,#25488),(#25489,#25490),(#25491,#25492),(#25493,#25494),(#25495,
#25496),(#25497,#25498),(#25499,#25500),(#25501,#25502),(#25503,#25504),
(#25505,#25506),(#25507,#25508),(#25509,#25510),(#25511,#25512),(#25513,
#25514),(#25515,#25516),(#25517,#25518),(#25519,#25520),(#25521,#25522),
(#25523,#25524),(#25525,#25526),(#25527,#25528),(#25529,#25530),(#25531,
#25532),(#25533,#25534),(#25535,#25536),(#25537,#25538),(#25539,#25540),
(#25541,#25542),(#25543,#25544),(#25545,#25546),(#25547,#25548),(#25549,
#25550),(#25551,#25552),(#25553,#25554),(#25555,#25556),(#25557,#25558),
(#25559,#25560),(#25561,#25562),(#25563,#25564),(#25565,#25566),(#25567,
#25568),(#25569,#25570),(#25571,#25572),(#25573,#25574),(#25575,#25576),
(#25577,#25578),(#25579,#25580),(#25581,#25582),(#25583,#25584),(#25585,
#25586),(#25587,#25588),(#25589,#25590),(#25591,#25592),(#25593,#25594),
(#25595,#25596),(#25597,#25598),(#25599,#25600),(#25601,#25602),(#25603,
#25604),(#25605,#25606),(#25607,#25608),(#25609,#25610),(#25611,#25612),
(#25613,#25614)),.UNSPECIFIED.,.F.,.F.,.F.,(6,1,1,1,1,1,1,1,1,1,1,1,1,1,
1,1,1,1,1,1,1,1,1,1,1,1,1,1,1,1,1,1,1,1,1,1,1,1,1,1,1,1,1,1,1,1,1,1,1,1,
1,1,1,1,1,1,1,1,1,1,1,1,1,1,1,1,1,1,1,1,6),(2,2),(-1.,-0.985714285714284,
-0.97142857142857,-0.957142857142856,-0.942857142857141,-0.928571428571427,
-0.914285714285713,-0.899999999999999,-0.885714285714284,-0.87142857142857,
-0.857142857142856,-0.842857142857142,-0.828571428571428,-0.814285714285713,
-0.799999999999999,-0.785714285714285,-0.771428571428571,-0.757142857142856,
-0.742857142857142,-0.728571428571428,-0.714285714285714,-0.699999999999999,
-0.685714285714285,-0.671428571428571,-0.657142857142857,-0.642857142857142,
-0.628571428571428,-0.614285714285714,-0.6,-0.585714285714286,-0.571428571428571,
-0.557142857142857,-0.542857142857143,-0.528571428571429,-0.514285714285714,
-0.5,-0.485714285714286,-0.471428571428572,-0.457142857142857,-0.442857142857143,
-0.428571428571429,-0.414285714285714,-0.4,-0.385714285714286,-0.371428571428571,
-0.357142857142857,-0.342857142857143,-0.328571428571429,-0.314285714285714,
-0.3,-0.285714285714286,-0.271428571428571,-0.257142857142857,-0.242857142857143,
-0.228571428571429,-0.214285714285714,-0.2,-0.185714285714286,-0.171428571428571,
-0.157142857142857,-0.142857142857143,-0.128571428571429,-0.114285714285714,
-0.1,-0.0857142857142857,-0.0714285714285714,-0.0571428571428571,-0.0428571428571429,
-0.0285714285714286,-0.0142857142857143,0.),(0.,1.8),.UNSPECIFIED.);
#968=B_SPLINE_SURFACE_WITH_KNOTS('',5,1,((#25773,#25774),(#25775,#25776),
(#25777,#25778),(#25779,#25780),(#25781,#25782),(#25783,#25784),(#25785,
#25786),(#25787,#25788),(#25789,#25790),(#25791,#25792),(#25793,#25794),
(#25795,#25796),(#25797,#25798),(#25799,#25800),(#25801,#25802),(#25803,
#25804),(#25805,#25806),(#25807,#25808),(#25809,#25810),(#25811,#25812),
(#25813,#25814),(#25815,#25816),(#25817,#25818),(#25819,#25820),(#25821,
#25822),(#25823,#25824),(#25825,#25826),(#25827,#25828),(#25829,#25830),
(#25831,#25832),(#25833,#25834),(#25835,#25836),(#25837,#25838),(#25839,
#25840),(#25841,#25842),(#25843,#25844),(#25845,#25846),(#25847,#25848),
(#25849,#25850),(#25851,#25852),(#25853,#25854),(#25855,#25856),(#25857,
#25858),(#25859,#25860),(#25861,#25862),(#25863,#25864),(#25865,#25866),
(#25867,#25868),(#25869,#25870),(#25871,#25872),(#25873,#25874),(#25875,
#25876),(#25877,#25878),(#25879,#25880),(#25881,#25882),(#25883,#25884),
(#25885,#25886),(#25887,#25888),(#25889,#25890),(#25891,#25892),(#25893,
#25894),(#25895,#25896),(#25897,#25898),(#25899,#25900),(#25901,#25902),
(#25903,#25904),(#25905,#25906),(#25907,#25908),(#25909,#25910),(#25911,
#25912),(#25913,#25914),(#25915,#25916),(#25917,#25918),(#25919,#25920),
(#25921,#25922)),.UNSPECIFIED.,.F.,.F.,.F.,(6,1,1,1,1,1,1,1,1,1,1,1,1,1,
1,1,1,1,1,1,1,1,1,1,1,1,1,1,1,1,1,1,1,1,1,1,1,1,1,1,1,1,1,1,1,1,1,1,1,1,
1,1,1,1,1,1,1,1,1,1,1,1,1,1,1,1,1,1,1,1,6),(2,2),(0.,0.0142857142857143,
0.0285714285714286,0.0428571428571429,0.0571428571428571,0.0714285714285714,
0.0857142857142857,0.1,0.114285714285714,0.128571428571429,0.142857142857143,
0.157142857142857,0.171428571428571,0.185714285714286,0.2,0.214285714285714,
0.228571428571429,0.242857142857143,0.257142857142857,0.271428571428571,
0.285714285714286,0.3,0.314285714285714,0.328571428571429,0.342857142857143,
0.357142857142857,0.371428571428571,0.385714285714286,0.4,0.414285714285714,
0.428571428571429,0.442857142857143,0.457142857142857,0.471428571428572,
0.485714285714286,0.5,0.514285714285714,0.528571428571429,0.542857142857143,
0.557142857142857,0.571428571428571,0.585714285714286,0.6,0.614285714285714,
0.628571428571428,0.642857142857142,0.657142857142857,0.671428571428571,
0.685714285714285,0.699999999999999,0.714285714285714,0.728571428571428,
0.742857142857142,0.757142857142856,0.771428571428571,0.785714285714285,
0.799999999999999,0.814285714285713,0.828571428571428,0.842857142857142,
0.857142857142856,0.87142857142857,0.885714285714284,0.899999999999999,
0.914285714285713,0.928571428571427,0.942857142857141,0.957142857142856,
0.97142857142857,0.985714285714284,1.),(0.,1.8),.UNSPECIFIED.);
#969=B_SPLINE_SURFACE_WITH_KNOTS('',5,1,((#26071,#26072),(#26073,#26074),
(#26075,#26076),(#26077,#26078),(#26079,#26080),(#26081,#26082),(#26083,
#26084),(#26085,#26086),(#26087,#26088),(#26089,#26090),(#26091,#26092),
(#26093,#26094),(#26095,#26096),(#26097,#26098),(#26099,#26100),(#26101,
#26102),(#26103,#26104),(#26105,#26106),(#26107,#26108),(#26109,#26110),
(#26111,#26112),(#26113,#26114),(#26115,#26116),(#26117,#26118),(#26119,
#26120),(#26121,#26122),(#26123,#26124),(#26125,#26126),(#26127,#26128),
(#26129,#26130),(#26131,#26132),(#26133,#26134),(#26135,#26136),(#26137,
#26138),(#26139,#26140),(#26141,#26142),(#26143,#26144),(#26145,#26146),
(#26147,#26148),(#26149,#26150),(#26151,#26152),(#26153,#26154),(#26155,
#26156),(#26157,#26158),(#26159,#26160),(#26161,#26162),(#26163,#26164),
(#26165,#26166),(#26167,#26168),(#26169,#26170),(#26171,#26172),(#26173,
#26174),(#26175,#26176),(#26177,#26178),(#26179,#26180),(#26181,#26182),
(#26183,#26184),(#26185,#26186),(#26187,#26188),(#26189,#26190),(#26191,
#26192),(#26193,#26194),(#26195,#26196),(#26197,#26198),(#26199,#26200),
(#26201,#26202),(#26203,#26204),(#26205,#26206),(#26207,#26208),(#26209,
#26210),(#26211,#26212),(#26213,#26214),(#26215,#26216),(#26217,#26218),
(#26219,#26220)),.UNSPECIFIED.,.F.,.F.,.F.,(6,1,1,1,1,1,1,1,1,1,1,1,1,1,
1,1,1,1,1,1,1,1,1,1,1,1,1,1,1,1,1,1,1,1,1,1,1,1,1,1,1,1,1,1,1,1,1,1,1,1,
1,1,1,1,1,1,1,1,1,1,1,1,1,1,1,1,1,1,1,1,6),(2,2),(-1.,-0.985714285714284,
-0.97142857142857,-0.957142857142856,-0.942857142857141,-0.928571428571427,
-0.914285714285713,-0.899999999999999,-0.885714285714284,-0.87142857142857,
-0.857142857142856,-0.842857142857142,-0.828571428571428,-0.814285714285713,
-0.799999999999999,-0.785714285714285,-0.771428571428571,-0.757142857142856,
-0.742857142857142,-0.728571428571428,-0.714285714285714,-0.699999999999999,
-0.685714285714285,-0.671428571428571,-0.657142857142857,-0.642857142857142,
-0.628571428571428,-0.614285714285714,-0.6,-0.585714285714286,-0.571428571428571,
-0.557142857142857,-0.542857142857143,-0.528571428571429,-0.514285714285714,
-0.5,-0.485714285714286,-0.471428571428572,-0.457142857142857,-0.442857142857143,
-0.428571428571429,-0.414285714285714,-0.4,-0.385714285714286,-0.371428571428571,
-0.357142857142857,-0.342857142857143,-0.328571428571429,-0.314285714285714,
-0.3,-0.285714285714286,-0.271428571428571,-0.257142857142857,-0.242857142857143,
-0.228571428571429,-0.214285714285714,-0.2,-0.185714285714286,-0.171428571428571,
-0.157142857142857,-0.142857142857143,-0.128571428571429,-0.114285714285714,
-0.1,-0.0857142857142857,-0.0714285714285714,-0.0571428571428571,-0.0428571428571429,
-0.0285714285714286,-0.0142857142857143,0.),(0.,1.8),.UNSPECIFIED.);
#970=B_SPLINE_SURFACE_WITH_KNOTS('',5,1,((#26379,#26380),(#26381,#26382),
(#26383,#26384),(#26385,#26386),(#26387,#26388),(#26389,#26390),(#26391,
#26392),(#26393,#26394),(#26395,#26396),(#26397,#26398),(#26399,#26400),
(#26401,#26402),(#26403,#26404),(#26405,#26406),(#26407,#26408),(#26409,
#26410),(#26411,#26412),(#26413,#26414),(#26415,#26416),(#26417,#26418),
(#26419,#26420),(#26421,#26422),(#26423,#26424),(#26425,#26426),(#26427,
#26428),(#26429,#26430),(#26431,#26432),(#26433,#26434),(#26435,#26436),
(#26437,#26438),(#26439,#26440),(#26441,#26442),(#26443,#26444),(#26445,
#26446),(#26447,#26448),(#26449,#26450),(#26451,#26452),(#26453,#26454),
(#26455,#26456),(#26457,#26458),(#26459,#26460),(#26461,#26462),(#26463,
#26464),(#26465,#26466),(#26467,#26468),(#26469,#26470),(#26471,#26472),
(#26473,#26474),(#26475,#26476),(#26477,#26478),(#26479,#26480),(#26481,
#26482),(#26483,#26484),(#26485,#26486),(#26487,#26488),(#26489,#26490),
(#26491,#26492),(#26493,#26494),(#26495,#26496),(#26497,#26498),(#26499,
#26500),(#26501,#26502),(#26503,#26504),(#26505,#26506),(#26507,#26508),
(#26509,#26510),(#26511,#26512),(#26513,#26514),(#26515,#26516),(#26517,
#26518),(#26519,#26520),(#26521,#26522),(#26523,#26524),(#26525,#26526),
(#26527,#26528)),.UNSPECIFIED.,.F.,.F.,.F.,(6,1,1,1,1,1,1,1,1,1,1,1,1,1,
1,1,1,1,1,1,1,1,1,1,1,1,1,1,1,1,1,1,1,1,1,1,1,1,1,1,1,1,1,1,1,1,1,1,1,1,
1,1,1,1,1,1,1,1,1,1,1,1,1,1,1,1,1,1,1,1,6),(2,2),(0.,0.0142857142857143,
0.0285714285714286,0.0428571428571429,0.0571428571428571,0.0714285714285714,
0.0857142857142857,0.1,0.114285714285714,0.128571428571429,0.142857142857143,
0.157142857142857,0.171428571428571,0.185714285714286,0.2,0.214285714285714,
0.228571428571429,0.242857142857143,0.257142857142857,0.271428571428571,
0.285714285714286,0.3,0.314285714285714,0.328571428571429,0.342857142857143,
0.357142857142857,0.371428571428571,0.385714285714286,0.4,0.414285714285714,
0.428571428571429,0.442857142857143,0.457142857142857,0.471428571428572,
0.485714285714286,0.5,0.514285714285714,0.528571428571429,0.542857142857143,
0.557142857142857,0.571428571428571,0.585714285714286,0.6,0.614285714285714,
0.628571428571428,0.642857142857142,0.657142857142857,0.671428571428571,
0.685714285714285,0.699999999999999,0.714285714285714,0.728571428571428,
0.742857142857142,0.757142857142856,0.771428571428571,0.785714285714285,
0.799999999999999,0.814285714285713,0.828571428571428,0.842857142857142,
0.857142857142856,0.87142857142857,0.885714285714284,0.899999999999999,
0.914285714285713,0.928571428571427,0.942857142857141,0.957142857142856,
0.97142857142857,0.985714285714284,1.),(0.,1.8),.UNSPECIFIED.);
#971=B_SPLINE_SURFACE_WITH_KNOTS('',5,1,((#26677,#26678),(#26679,#26680),
(#26681,#26682),(#26683,#26684),(#26685,#26686),(#26687,#26688),(#26689,
#26690),(#26691,#26692),(#26693,#26694),(#26695,#26696),(#26697,#26698),
(#26699,#26700),(#26701,#26702),(#26703,#26704),(#26705,#26706),(#26707,
#26708),(#26709,#26710),(#26711,#26712),(#26713,#26714),(#26715,#26716),
(#26717,#26718),(#26719,#26720),(#26721,#26722),(#26723,#26724),(#26725,
#26726),(#26727,#26728),(#26729,#26730),(#26731,#26732),(#26733,#26734),
(#26735,#26736),(#26737,#26738),(#26739,#26740),(#26741,#26742),(#26743,
#26744),(#26745,#26746),(#26747,#26748),(#26749,#26750),(#26751,#26752),
(#26753,#26754),(#26755,#26756),(#26757,#26758),(#26759,#26760),(#26761,
#26762),(#26763,#26764),(#26765,#26766),(#26767,#26768),(#26769,#26770),
(#26771,#26772),(#26773,#26774),(#26775,#26776),(#26777,#26778),(#26779,
#26780),(#26781,#26782),(#26783,#26784),(#26785,#26786),(#26787,#26788),
(#26789,#26790),(#26791,#26792),(#26793,#26794),(#26795,#26796),(#26797,
#26798),(#26799,#26800),(#26801,#26802),(#26803,#26804),(#26805,#26806),
(#26807,#26808),(#26809,#26810),(#26811,#26812),(#26813,#26814),(#26815,
#26816),(#26817,#26818),(#26819,#26820),(#26821,#26822),(#26823,#26824),
(#26825,#26826)),.UNSPECIFIED.,.F.,.F.,.F.,(6,1,1,1,1,1,1,1,1,1,1,1,1,1,
1,1,1,1,1,1,1,1,1,1,1,1,1,1,1,1,1,1,1,1,1,1,1,1,1,1,1,1,1,1,1,1,1,1,1,1,
1,1,1,1,1,1,1,1,1,1,1,1,1,1,1,1,1,1,1,1,6),(2,2),(-1.,-0.985714285714284,
-0.97142857142857,-0.957142857142856,-0.942857142857141,-0.928571428571427,
-0.914285714285713,-0.899999999999999,-0.885714285714284,-0.87142857142857,
-0.857142857142856,-0.842857142857142,-0.828571428571428,-0.814285714285713,
-0.799999999999999,-0.785714285714285,-0.771428571428571,-0.757142857142856,
-0.742857142857142,-0.728571428571428,-0.714285714285714,-0.699999999999999,
-0.685714285714285,-0.671428571428571,-0.657142857142857,-0.642857142857142,
-0.628571428571428,-0.614285714285714,-0.6,-0.585714285714286,-0.571428571428571,
-0.557142857142857,-0.542857142857143,-0.528571428571429,-0.514285714285714,
-0.5,-0.485714285714286,-0.471428571428572,-0.457142857142857,-0.442857142857143,
-0.428571428571429,-0.414285714285714,-0.4,-0.385714285714286,-0.371428571428571,
-0.357142857142857,-0.342857142857143,-0.328571428571429,-0.314285714285714,
-0.3,-0.285714285714286,-0.271428571428571,-0.257142857142857,-0.242857142857143,
-0.228571428571429,-0.214285714285714,-0.2,-0.185714285714286,-0.171428571428571,
-0.157142857142857,-0.142857142857143,-0.128571428571429,-0.114285714285714,
-0.1,-0.0857142857142857,-0.0714285714285714,-0.0571428571428571,-0.0428571428571429,
-0.0285714285714286,-0.0142857142857143,0.),(0.,1.8),.UNSPECIFIED.);
#972=B_SPLINE_SURFACE_WITH_KNOTS('',5,1,((#26985,#26986),(#26987,#26988),
(#26989,#26990),(#26991,#26992),(#26993,#26994),(#26995,#26996),(#26997,
#26998),(#26999,#27000),(#27001,#27002),(#27003,#27004),(#27005,#27006),
(#27007,#27008),(#27009,#27010),(#27011,#27012),(#27013,#27014),(#27015,
#27016),(#27017,#27018),(#27019,#27020),(#27021,#27022),(#27023,#27024),
(#27025,#27026),(#27027,#27028),(#27029,#27030),(#27031,#27032),(#27033,
#27034),(#27035,#27036),(#27037,#27038),(#27039,#27040),(#27041,#27042),
(#27043,#27044),(#27045,#27046),(#27047,#27048),(#27049,#27050),(#27051,
#27052),(#27053,#27054),(#27055,#27056),(#27057,#27058),(#27059,#27060),
(#27061,#27062),(#27063,#27064),(#27065,#27066),(#27067,#27068),(#27069,
#27070),(#27071,#27072),(#27073,#27074),(#27075,#27076),(#27077,#27078),
(#27079,#27080),(#27081,#27082),(#27083,#27084),(#27085,#27086),(#27087,
#27088),(#27089,#27090),(#27091,#27092),(#27093,#27094),(#27095,#27096),
(#27097,#27098),(#27099,#27100),(#27101,#27102),(#27103,#27104),(#27105,
#27106),(#27107,#27108),(#27109,#27110),(#27111,#27112),(#27113,#27114),
(#27115,#27116),(#27117,#27118),(#27119,#27120),(#27121,#27122),(#27123,
#27124),(#27125,#27126),(#27127,#27128),(#27129,#27130),(#27131,#27132),
(#27133,#27134)),.UNSPECIFIED.,.F.,.F.,.F.,(6,1,1,1,1,1,1,1,1,1,1,1,1,1,
1,1,1,1,1,1,1,1,1,1,1,1,1,1,1,1,1,1,1,1,1,1,1,1,1,1,1,1,1,1,1,1,1,1,1,1,
1,1,1,1,1,1,1,1,1,1,1,1,1,1,1,1,1,1,1,1,6),(2,2),(0.,0.0142857142857143,
0.0285714285714286,0.0428571428571429,0.0571428571428571,0.0714285714285714,
0.0857142857142857,0.1,0.114285714285714,0.128571428571429,0.142857142857143,
0.157142857142857,0.171428571428571,0.185714285714286,0.2,0.214285714285714,
0.228571428571429,0.242857142857143,0.257142857142857,0.271428571428571,
0.285714285714286,0.3,0.314285714285714,0.328571428571429,0.342857142857143,
0.357142857142857,0.371428571428571,0.385714285714286,0.4,0.414285714285714,
0.428571428571429,0.442857142857143,0.457142857142857,0.471428571428572,
0.485714285714286,0.5,0.514285714285714,0.528571428571429,0.542857142857143,
0.557142857142857,0.571428571428571,0.585714285714286,0.6,0.614285714285714,
0.628571428571428,0.642857142857142,0.657142857142857,0.671428571428571,
0.685714285714285,0.699999999999999,0.714285714285714,0.728571428571428,
0.742857142857142,0.757142857142856,0.771428571428571,0.785714285714285,
0.799999999999999,0.814285714285713,0.828571428571428,0.842857142857142,
0.857142857142856,0.87142857142857,0.885714285714284,0.899999999999999,
0.914285714285713,0.928571428571427,0.942857142857141,0.957142857142856,
0.97142857142857,0.985714285714284,1.),(0.,1.8),.UNSPECIFIED.);
#973=B_SPLINE_SURFACE_WITH_KNOTS('',5,1,((#27283,#27284),(#27285,#27286),
(#27287,#27288),(#27289,#27290),(#27291,#27292),(#27293,#27294),(#27295,
#27296),(#27297,#27298),(#27299,#27300),(#27301,#27302),(#27303,#27304),
(#27305,#27306),(#27307,#27308),(#27309,#27310),(#27311,#27312),(#27313,
#27314),(#27315,#27316),(#27317,#27318),(#27319,#27320),(#27321,#27322),
(#27323,#27324),(#27325,#27326),(#27327,#27328),(#27329,#27330),(#27331,
#27332),(#27333,#27334),(#27335,#27336),(#27337,#27338),(#27339,#27340),
(#27341,#27342),(#27343,#27344),(#27345,#27346),(#27347,#27348),(#27349,
#27350),(#27351,#27352),(#27353,#27354),(#27355,#27356),(#27357,#27358),
(#27359,#27360),(#27361,#27362),(#27363,#27364),(#27365,#27366),(#27367,
#27368),(#27369,#27370),(#27371,#27372),(#27373,#27374),(#27375,#27376),
(#27377,#27378),(#27379,#27380),(#27381,#27382),(#27383,#27384),(#27385,
#27386),(#27387,#27388),(#27389,#27390),(#27391,#27392),(#27393,#27394),
(#27395,#27396),(#27397,#27398),(#27399,#27400),(#27401,#27402),(#27403,
#27404),(#27405,#27406),(#27407,#27408),(#27409,#27410),(#27411,#27412),
(#27413,#27414),(#27415,#27416),(#27417,#27418),(#27419,#27420),(#27421,
#27422),(#27423,#27424),(#27425,#27426),(#27427,#27428),(#27429,#27430),
(#27431,#27432)),.UNSPECIFIED.,.F.,.F.,.F.,(6,1,1,1,1,1,1,1,1,1,1,1,1,1,
1,1,1,1,1,1,1,1,1,1,1,1,1,1,1,1,1,1,1,1,1,1,1,1,1,1,1,1,1,1,1,1,1,1,1,1,
1,1,1,1,1,1,1,1,1,1,1,1,1,1,1,1,1,1,1,1,6),(2,2),(-1.,-0.985714285714284,
-0.97142857142857,-0.957142857142856,-0.942857142857141,-0.928571428571427,
-0.914285714285713,-0.899999999999999,-0.885714285714284,-0.87142857142857,
-0.857142857142856,-0.842857142857142,-0.828571428571428,-0.814285714285713,
-0.799999999999999,-0.785714285714285,-0.771428571428571,-0.757142857142856,
-0.742857142857142,-0.728571428571428,-0.714285714285714,-0.699999999999999,
-0.685714285714285,-0.671428571428571,-0.657142857142857,-0.642857142857142,
-0.628571428571428,-0.614285714285714,-0.6,-0.585714285714286,-0.571428571428571,
-0.557142857142857,-0.542857142857143,-0.528571428571429,-0.514285714285714,
-0.5,-0.485714285714286,-0.471428571428572,-0.457142857142857,-0.442857142857143,
-0.428571428571429,-0.414285714285714,-0.4,-0.385714285714286,-0.371428571428571,
-0.357142857142857,-0.342857142857143,-0.328571428571429,-0.314285714285714,
-0.3,-0.285714285714286,-0.271428571428571,-0.257142857142857,-0.242857142857143,
-0.228571428571429,-0.214285714285714,-0.2,-0.185714285714286,-0.171428571428571,
-0.157142857142857,-0.142857142857143,-0.128571428571429,-0.114285714285714,
-0.1,-0.0857142857142857,-0.0714285714285714,-0.0571428571428571,-0.0428571428571429,
-0.0285714285714286,-0.0142857142857143,0.),(0.,1.8),.UNSPECIFIED.);
#974=B_SPLINE_SURFACE_WITH_KNOTS('',5,1,((#27591,#27592),(#27593,#27594),
(#27595,#27596),(#27597,#27598),(#27599,#27600),(#27601,#27602),(#27603,
#27604),(#27605,#27606),(#27607,#27608),(#27609,#27610),(#27611,#27612),
(#27613,#27614),(#27615,#27616),(#27617,#27618),(#27619,#27620),(#27621,
#27622),(#27623,#27624),(#27625,#27626),(#27627,#27628),(#27629,#27630),
(#27631,#27632),(#27633,#27634),(#27635,#27636),(#27637,#27638),(#27639,
#27640),(#27641,#27642),(#27643,#27644),(#27645,#27646),(#27647,#27648),
(#27649,#27650),(#27651,#27652),(#27653,#27654),(#27655,#27656),(#27657,
#27658),(#27659,#27660),(#27661,#27662),(#27663,#27664),(#27665,#27666),
(#27667,#27668),(#27669,#27670),(#27671,#27672),(#27673,#27674),(#27675,
#27676),(#27677,#27678),(#27679,#27680),(#27681,#27682),(#27683,#27684),
(#27685,#27686),(#27687,#27688),(#27689,#27690),(#27691,#27692),(#27693,
#27694),(#27695,#27696),(#27697,#27698),(#27699,#27700),(#27701,#27702),
(#27703,#27704),(#27705,#27706),(#27707,#27708),(#27709,#27710),(#27711,
#27712),(#27713,#27714),(#27715,#27716),(#27717,#27718),(#27719,#27720),
(#27721,#27722),(#27723,#27724),(#27725,#27726),(#27727,#27728),(#27729,
#27730),(#27731,#27732),(#27733,#27734),(#27735,#27736),(#27737,#27738),
(#27739,#27740)),.UNSPECIFIED.,.F.,.F.,.F.,(6,1,1,1,1,1,1,1,1,1,1,1,1,1,
1,1,1,1,1,1,1,1,1,1,1,1,1,1,1,1,1,1,1,1,1,1,1,1,1,1,1,1,1,1,1,1,1,1,1,1,
1,1,1,1,1,1,1,1,1,1,1,1,1,1,1,1,1,1,1,1,6),(2,2),(0.,0.0142857142857143,
0.0285714285714286,0.0428571428571429,0.0571428571428571,0.0714285714285714,
0.0857142857142857,0.1,0.114285714285714,0.128571428571429,0.142857142857143,
0.157142857142857,0.171428571428571,0.185714285714286,0.2,0.214285714285714,
0.228571428571429,0.242857142857143,0.257142857142857,0.271428571428571,
0.285714285714286,0.3,0.314285714285714,0.328571428571429,0.342857142857143,
0.357142857142857,0.371428571428571,0.385714285714286,0.4,0.414285714285714,
0.428571428571429,0.442857142857143,0.457142857142857,0.471428571428572,
0.485714285714286,0.5,0.514285714285714,0.528571428571429,0.542857142857143,
0.557142857142857,0.571428571428571,0.585714285714286,0.6,0.614285714285714,
0.628571428571428,0.642857142857142,0.657142857142857,0.671428571428571,
0.685714285714285,0.699999999999999,0.714285714285714,0.728571428571428,
0.742857142857142,0.757142857142856,0.771428571428571,0.785714285714285,
0.799999999999999,0.814285714285713,0.828571428571428,0.842857142857142,
0.857142857142856,0.87142857142857,0.885714285714284,0.899999999999999,
0.914285714285713,0.928571428571427,0.942857142857141,0.957142857142856,
0.97142857142857,0.985714285714284,1.),(0.,1.8),.UNSPECIFIED.);
#975=B_SPLINE_SURFACE_WITH_KNOTS('',5,1,((#27889,#27890),(#27891,#27892),
(#27893,#27894),(#27895,#27896),(#27897,#27898),(#27899,#27900),(#27901,
#27902),(#27903,#27904),(#27905,#27906),(#27907,#27908),(#27909,#27910),
(#27911,#27912),(#27913,#27914),(#27915,#27916),(#27917,#27918),(#27919,
#27920),(#27921,#27922),(#27923,#27924),(#27925,#27926),(#27927,#27928),
(#27929,#27930),(#27931,#27932),(#27933,#27934),(#27935,#27936),(#27937,
#27938),(#27939,#27940),(#27941,#27942),(#27943,#27944),(#27945,#27946),
(#27947,#27948),(#27949,#27950),(#27951,#27952),(#27953,#27954),(#27955,
#27956),(#27957,#27958),(#27959,#27960),(#27961,#27962),(#27963,#27964),
(#27965,#27966),(#27967,#27968),(#27969,#27970),(#27971,#27972),(#27973,
#27974),(#27975,#27976),(#27977,#27978),(#27979,#27980),(#27981,#27982),
(#27983,#27984),(#27985,#27986),(#27987,#27988),(#27989,#27990),(#27991,
#27992),(#27993,#27994),(#27995,#27996),(#27997,#27998),(#27999,#28000),
(#28001,#28002),(#28003,#28004),(#28005,#28006),(#28007,#28008),(#28009,
#28010),(#28011,#28012),(#28013,#28014),(#28015,#28016),(#28017,#28018),
(#28019,#28020),(#28021,#28022),(#28023,#28024),(#28025,#28026),(#28027,
#28028),(#28029,#28030),(#28031,#28032),(#28033,#28034),(#28035,#28036),
(#28037,#28038)),.UNSPECIFIED.,.F.,.F.,.F.,(6,1,1,1,1,1,1,1,1,1,1,1,1,1,
1,1,1,1,1,1,1,1,1,1,1,1,1,1,1,1,1,1,1,1,1,1,1,1,1,1,1,1,1,1,1,1,1,1,1,1,
1,1,1,1,1,1,1,1,1,1,1,1,1,1,1,1,1,1,1,1,6),(2,2),(-1.,-0.985714285714284,
-0.97142857142857,-0.957142857142856,-0.942857142857141,-0.928571428571427,
-0.914285714285713,-0.899999999999999,-0.885714285714284,-0.87142857142857,
-0.857142857142856,-0.842857142857142,-0.828571428571428,-0.814285714285713,
-0.799999999999999,-0.785714285714285,-0.771428571428571,-0.757142857142856,
-0.742857142857142,-0.728571428571428,-0.714285714285714,-0.699999999999999,
-0.685714285714285,-0.671428571428571,-0.657142857142857,-0.642857142857142,
-0.628571428571428,-0.614285714285714,-0.6,-0.585714285714286,-0.571428571428571,
-0.557142857142857,-0.542857142857143,-0.528571428571429,-0.514285714285714,
-0.5,-0.485714285714286,-0.471428571428572,-0.457142857142857,-0.442857142857143,
-0.428571428571429,-0.414285714285714,-0.4,-0.385714285714286,-0.371428571428571,
-0.357142857142857,-0.342857142857143,-0.328571428571429,-0.314285714285714,
-0.3,-0.285714285714286,-0.271428571428571,-0.257142857142857,-0.242857142857143,
-0.228571428571429,-0.214285714285714,-0.2,-0.185714285714286,-0.171428571428571,
-0.157142857142857,-0.142857142857143,-0.128571428571429,-0.114285714285714,
-0.1,-0.0857142857142857,-0.0714285714285714,-0.0571428571428571,-0.0428571428571429,
-0.0285714285714286,-0.0142857142857143,0.),(0.,1.8),.UNSPECIFIED.);
#976=B_SPLINE_SURFACE_WITH_KNOTS('',5,1,((#28197,#28198),(#28199,#28200),
(#28201,#28202),(#28203,#28204),(#28205,#28206),(#28207,#28208),(#28209,
#28210),(#28211,#28212),(#28213,#28214),(#28215,#28216),(#28217,#28218),
(#28219,#28220),(#28221,#28222),(#28223,#28224),(#28225,#28226),(#28227,
#28228),(#28229,#28230),(#28231,#28232),(#28233,#28234),(#28235,#28236),
(#28237,#28238),(#28239,#28240),(#28241,#28242),(#28243,#28244),(#28245,
#28246),(#28247,#28248),(#28249,#28250),(#28251,#28252),(#28253,#28254),
(#28255,#28256),(#28257,#28258),(#28259,#28260),(#28261,#28262),(#28263,
#28264),(#28265,#28266),(#28267,#28268),(#28269,#28270),(#28271,#28272),
(#28273,#28274),(#28275,#28276),(#28277,#28278),(#28279,#28280),(#28281,
#28282),(#28283,#28284),(#28285,#28286),(#28287,#28288),(#28289,#28290),
(#28291,#28292),(#28293,#28294),(#28295,#28296),(#28297,#28298),(#28299,
#28300),(#28301,#28302),(#28303,#28304),(#28305,#28306),(#28307,#28308),
(#28309,#28310),(#28311,#28312),(#28313,#28314),(#28315,#28316),(#28317,
#28318),(#28319,#28320),(#28321,#28322),(#28323,#28324),(#28325,#28326),
(#28327,#28328),(#28329,#28330),(#28331,#28332),(#28333,#28334),(#28335,
#28336),(#28337,#28338),(#28339,#28340),(#28341,#28342),(#28343,#28344),
(#28345,#28346)),.UNSPECIFIED.,.F.,.F.,.F.,(6,1,1,1,1,1,1,1,1,1,1,1,1,1,
1,1,1,1,1,1,1,1,1,1,1,1,1,1,1,1,1,1,1,1,1,1,1,1,1,1,1,1,1,1,1,1,1,1,1,1,
1,1,1,1,1,1,1,1,1,1,1,1,1,1,1,1,1,1,1,1,6),(2,2),(0.,0.0142857142857143,
0.0285714285714286,0.0428571428571429,0.0571428571428571,0.0714285714285714,
0.0857142857142857,0.1,0.114285714285714,0.128571428571429,0.142857142857143,
0.157142857142857,0.171428571428571,0.185714285714286,0.2,0.214285714285714,
0.228571428571429,0.242857142857143,0.257142857142857,0.271428571428571,
0.285714285714286,0.3,0.314285714285714,0.328571428571429,0.342857142857143,
0.357142857142857,0.371428571428571,0.385714285714286,0.4,0.414285714285714,
0.428571428571429,0.442857142857143,0.457142857142857,0.471428571428572,
0.485714285714286,0.5,0.514285714285714,0.528571428571429,0.542857142857143,
0.557142857142857,0.571428571428571,0.585714285714286,0.6,0.614285714285714,
0.628571428571428,0.642857142857142,0.657142857142857,0.671428571428571,
0.685714285714285,0.699999999999999,0.714285714285714,0.728571428571428,
0.742857142857142,0.757142857142856,0.771428571428571,0.785714285714285,
0.799999999999999,0.814285714285713,0.828571428571428,0.842857142857142,
0.857142857142856,0.87142857142857,0.885714285714284,0.899999999999999,
0.914285714285713,0.928571428571427,0.942857142857141,0.957142857142856,
0.97142857142857,0.985714285714284,1.),(0.,1.8),.UNSPECIFIED.);
#977=B_SPLINE_SURFACE_WITH_KNOTS('',5,1,((#28495,#28496),(#28497,#28498),
(#28499,#28500),(#28501,#28502),(#28503,#28504),(#28505,#28506),(#28507,
#28508),(#28509,#28510),(#28511,#28512),(#28513,#28514),(#28515,#28516),
(#28517,#28518),(#28519,#28520),(#28521,#28522),(#28523,#28524),(#28525,
#28526),(#28527,#28528),(#28529,#28530),(#28531,#28532),(#28533,#28534),
(#28535,#28536),(#28537,#28538),(#28539,#28540),(#28541,#28542),(#28543,
#28544),(#28545,#28546),(#28547,#28548),(#28549,#28550),(#28551,#28552),
(#28553,#28554),(#28555,#28556),(#28557,#28558),(#28559,#28560),(#28561,
#28562),(#28563,#28564),(#28565,#28566),(#28567,#28568),(#28569,#28570),
(#28571,#28572),(#28573,#28574),(#28575,#28576),(#28577,#28578),(#28579,
#28580),(#28581,#28582),(#28583,#28584),(#28585,#28586),(#28587,#28588),
(#28589,#28590),(#28591,#28592),(#28593,#28594),(#28595,#28596),(#28597,
#28598),(#28599,#28600),(#28601,#28602),(#28603,#28604),(#28605,#28606),
(#28607,#28608),(#28609,#28610),(#28611,#28612),(#28613,#28614),(#28615,
#28616),(#28617,#28618),(#28619,#28620),(#28621,#28622),(#28623,#28624),
(#28625,#28626),(#28627,#28628),(#28629,#28630),(#28631,#28632),(#28633,
#28634),(#28635,#28636),(#28637,#28638),(#28639,#28640),(#28641,#28642),
(#28643,#28644)),.UNSPECIFIED.,.F.,.F.,.F.,(6,1,1,1,1,1,1,1,1,1,1,1,1,1,
1,1,1,1,1,1,1,1,1,1,1,1,1,1,1,1,1,1,1,1,1,1,1,1,1,1,1,1,1,1,1,1,1,1,1,1,
1,1,1,1,1,1,1,1,1,1,1,1,1,1,1,1,1,1,1,1,6),(2,2),(-1.,-0.985714285714284,
-0.97142857142857,-0.957142857142856,-0.942857142857141,-0.928571428571427,
-0.914285714285713,-0.899999999999999,-0.885714285714284,-0.87142857142857,
-0.857142857142856,-0.842857142857142,-0.828571428571428,-0.814285714285713,
-0.799999999999999,-0.785714285714285,-0.771428571428571,-0.757142857142856,
-0.742857142857142,-0.728571428571428,-0.714285714285714,-0.699999999999999,
-0.685714285714285,-0.671428571428571,-0.657142857142857,-0.642857142857142,
-0.628571428571428,-0.614285714285714,-0.6,-0.585714285714286,-0.571428571428571,
-0.557142857142857,-0.542857142857143,-0.528571428571429,-0.514285714285714,
-0.5,-0.485714285714286,-0.471428571428572,-0.457142857142857,-0.442857142857143,
-0.428571428571429,-0.414285714285714,-0.4,-0.385714285714286,-0.371428571428571,
-0.357142857142857,-0.342857142857143,-0.328571428571429,-0.314285714285714,
-0.3,-0.285714285714286,-0.271428571428571,-0.257142857142857,-0.242857142857143,
-0.228571428571429,-0.214285714285714,-0.2,-0.185714285714286,-0.171428571428571,
-0.157142857142857,-0.142857142857143,-0.128571428571429,-0.114285714285714,
-0.1,-0.0857142857142857,-0.0714285714285714,-0.0571428571428571,-0.0428571428571429,
-0.0285714285714286,-0.0142857142857143,0.),(0.,1.8),.UNSPECIFIED.);
#978=B_SPLINE_SURFACE_WITH_KNOTS('',5,1,((#28803,#28804),(#28805,#28806),
(#28807,#28808),(#28809,#28810),(#28811,#28812),(#28813,#28814),(#28815,
#28816),(#28817,#28818),(#28819,#28820),(#28821,#28822),(#28823,#28824),
(#28825,#28826),(#28827,#28828),(#28829,#28830),(#28831,#28832),(#28833,
#28834),(#28835,#28836),(#28837,#28838),(#28839,#28840),(#28841,#28842),
(#28843,#28844),(#28845,#28846),(#28847,#28848),(#28849,#28850),(#28851,
#28852),(#28853,#28854),(#28855,#28856),(#28857,#28858),(#28859,#28860),
(#28861,#28862),(#28863,#28864),(#28865,#28866),(#28867,#28868),(#28869,
#28870),(#28871,#28872),(#28873,#28874),(#28875,#28876),(#28877,#28878),
(#28879,#28880),(#28881,#28882),(#28883,#28884),(#28885,#28886),(#28887,
#28888),(#28889,#28890),(#28891,#28892),(#28893,#28894),(#28895,#28896),
(#28897,#28898),(#28899,#28900),(#28901,#28902),(#28903,#28904),(#28905,
#28906),(#28907,#28908),(#28909,#28910),(#28911,#28912),(#28913,#28914),
(#28915,#28916),(#28917,#28918),(#28919,#28920),(#28921,#28922),(#28923,
#28924),(#28925,#28926),(#28927,#28928),(#28929,#28930),(#28931,#28932),
(#28933,#28934),(#28935,#28936),(#28937,#28938),(#28939,#28940),(#28941,
#28942),(#28943,#28944),(#28945,#28946),(#28947,#28948),(#28949,#28950),
(#28951,#28952)),.UNSPECIFIED.,.F.,.F.,.F.,(6,1,1,1,1,1,1,1,1,1,1,1,1,1,
1,1,1,1,1,1,1,1,1,1,1,1,1,1,1,1,1,1,1,1,1,1,1,1,1,1,1,1,1,1,1,1,1,1,1,1,
1,1,1,1,1,1,1,1,1,1,1,1,1,1,1,1,1,1,1,1,6),(2,2),(0.,0.0142857142857143,
0.0285714285714286,0.0428571428571429,0.0571428571428571,0.0714285714285714,
0.0857142857142857,0.1,0.114285714285714,0.128571428571429,0.142857142857143,
0.157142857142857,0.171428571428571,0.185714285714286,0.2,0.214285714285714,
0.228571428571429,0.242857142857143,0.257142857142857,0.271428571428571,
0.285714285714286,0.3,0.314285714285714,0.328571428571429,0.342857142857143,
0.357142857142857,0.371428571428571,0.385714285714286,0.4,0.414285714285714,
0.428571428571429,0.442857142857143,0.457142857142857,0.471428571428572,
0.485714285714286,0.5,0.514285714285714,0.528571428571429,0.542857142857143,
0.557142857142857,0.571428571428571,0.585714285714286,0.6,0.614285714285714,
0.628571428571428,0.642857142857142,0.657142857142857,0.671428571428571,
0.685714285714285,0.699999999999999,0.714285714285714,0.728571428571428,
0.742857142857142,0.757142857142856,0.771428571428571,0.785714285714285,
0.799999999999999,0.814285714285713,0.828571428571428,0.842857142857142,
0.857142857142856,0.87142857142857,0.885714285714284,0.899999999999999,
0.914285714285713,0.928571428571427,0.942857142857141,0.957142857142856,
0.97142857142857,0.985714285714284,1.),(0.,1.8),.UNSPECIFIED.);
#979=B_SPLINE_SURFACE_WITH_KNOTS('',5,1,((#29101,#29102),(#29103,#29104),
(#29105,#29106),(#29107,#29108),(#29109,#29110),(#29111,#29112),(#29113,
#29114),(#29115,#29116),(#29117,#29118),(#29119,#29120),(#29121,#29122),
(#29123,#29124),(#29125,#29126),(#29127,#29128),(#29129,#29130),(#29131,
#29132),(#29133,#29134),(#29135,#29136),(#29137,#29138),(#29139,#29140),
(#29141,#29142),(#29143,#29144),(#29145,#29146),(#29147,#29148),(#29149,
#29150),(#29151,#29152),(#29153,#29154),(#29155,#29156),(#29157,#29158),
(#29159,#29160),(#29161,#29162),(#29163,#29164),(#29165,#29166),(#29167,
#29168),(#29169,#29170),(#29171,#29172),(#29173,#29174),(#29175,#29176),
(#29177,#29178),(#29179,#29180),(#29181,#29182),(#29183,#29184),(#29185,
#29186),(#29187,#29188),(#29189,#29190),(#29191,#29192),(#29193,#29194),
(#29195,#29196),(#29197,#29198),(#29199,#29200),(#29201,#29202),(#29203,
#29204),(#29205,#29206),(#29207,#29208),(#29209,#29210),(#29211,#29212),
(#29213,#29214),(#29215,#29216),(#29217,#29218),(#29219,#29220),(#29221,
#29222),(#29223,#29224),(#29225,#29226),(#29227,#29228),(#29229,#29230),
(#29231,#29232),(#29233,#29234),(#29235,#29236),(#29237,#29238),(#29239,
#29240),(#29241,#29242),(#29243,#29244),(#29245,#29246),(#29247,#29248),
(#29249,#29250)),.UNSPECIFIED.,.F.,.F.,.F.,(6,1,1,1,1,1,1,1,1,1,1,1,1,1,
1,1,1,1,1,1,1,1,1,1,1,1,1,1,1,1,1,1,1,1,1,1,1,1,1,1,1,1,1,1,1,1,1,1,1,1,
1,1,1,1,1,1,1,1,1,1,1,1,1,1,1,1,1,1,1,1,6),(2,2),(-1.,-0.985714285714284,
-0.97142857142857,-0.957142857142856,-0.942857142857141,-0.928571428571427,
-0.914285714285713,-0.899999999999999,-0.885714285714284,-0.87142857142857,
-0.857142857142856,-0.842857142857142,-0.828571428571428,-0.814285714285713,
-0.799999999999999,-0.785714285714285,-0.771428571428571,-0.757142857142856,
-0.742857142857142,-0.728571428571428,-0.714285714285714,-0.699999999999999,
-0.685714285714285,-0.671428571428571,-0.657142857142857,-0.642857142857142,
-0.628571428571428,-0.614285714285714,-0.6,-0.585714285714286,-0.571428571428571,
-0.557142857142857,-0.542857142857143,-0.528571428571429,-0.514285714285714,
-0.5,-0.485714285714286,-0.471428571428572,-0.457142857142857,-0.442857142857143,
-0.428571428571429,-0.414285714285714,-0.4,-0.385714285714286,-0.371428571428571,
-0.357142857142857,-0.342857142857143,-0.328571428571429,-0.314285714285714,
-0.3,-0.285714285714286,-0.271428571428571,-0.257142857142857,-0.242857142857143,
-0.228571428571429,-0.214285714285714,-0.2,-0.185714285714286,-0.171428571428571,
-0.157142857142857,-0.142857142857143,-0.128571428571429,-0.114285714285714,
-0.1,-0.0857142857142857,-0.0714285714285714,-0.0571428571428571,-0.0428571428571429,
-0.0285714285714286,-0.0142857142857143,0.),(0.,1.8),.UNSPECIFIED.);
#980=B_SPLINE_SURFACE_WITH_KNOTS('',5,1,((#29409,#29410),(#29411,#29412),
(#29413,#29414),(#29415,#29416),(#29417,#29418),(#29419,#29420),(#29421,
#29422),(#29423,#29424),(#29425,#29426),(#29427,#29428),(#29429,#29430),
(#29431,#29432),(#29433,#29434),(#29435,#29436),(#29437,#29438),(#29439,
#29440),(#29441,#29442),(#29443,#29444),(#29445,#29446),(#29447,#29448),
(#29449,#29450),(#29451,#29452),(#29453,#29454),(#29455,#29456),(#29457,
#29458),(#29459,#29460),(#29461,#29462),(#29463,#29464),(#29465,#29466),
(#29467,#29468),(#29469,#29470),(#29471,#29472),(#29473,#29474),(#29475,
#29476),(#29477,#29478),(#29479,#29480),(#29481,#29482),(#29483,#29484),
(#29485,#29486),(#29487,#29488),(#29489,#29490),(#29491,#29492),(#29493,
#29494),(#29495,#29496),(#29497,#29498),(#29499,#29500),(#29501,#29502),
(#29503,#29504),(#29505,#29506),(#29507,#29508),(#29509,#29510),(#29511,
#29512),(#29513,#29514),(#29515,#29516),(#29517,#29518),(#29519,#29520),
(#29521,#29522),(#29523,#29524),(#29525,#29526),(#29527,#29528),(#29529,
#29530),(#29531,#29532),(#29533,#29534),(#29535,#29536),(#29537,#29538),
(#29539,#29540),(#29541,#29542),(#29543,#29544),(#29545,#29546),(#29547,
#29548),(#29549,#29550),(#29551,#29552),(#29553,#29554),(#29555,#29556),
(#29557,#29558)),.UNSPECIFIED.,.F.,.F.,.F.,(6,1,1,1,1,1,1,1,1,1,1,1,1,1,
1,1,1,1,1,1,1,1,1,1,1,1,1,1,1,1,1,1,1,1,1,1,1,1,1,1,1,1,1,1,1,1,1,1,1,1,
1,1,1,1,1,1,1,1,1,1,1,1,1,1,1,1,1,1,1,1,6),(2,2),(0.,0.0142857142857143,
0.0285714285714286,0.0428571428571429,0.0571428571428571,0.0714285714285714,
0.0857142857142857,0.1,0.114285714285714,0.128571428571429,0.142857142857143,
0.157142857142857,0.171428571428571,0.185714285714286,0.2,0.214285714285714,
0.228571428571429,0.242857142857143,0.257142857142857,0.271428571428571,
0.285714285714286,0.3,0.314285714285714,0.328571428571429,0.342857142857143,
0.357142857142857,0.371428571428571,0.385714285714286,0.4,0.414285714285714,
0.428571428571429,0.442857142857143,0.457142857142857,0.471428571428572,
0.485714285714286,0.5,0.514285714285714,0.528571428571429,0.542857142857143,
0.557142857142857,0.571428571428571,0.585714285714286,0.6,0.614285714285714,
0.628571428571428,0.642857142857142,0.657142857142857,0.671428571428571,
0.685714285714285,0.699999999999999,0.714285714285714,0.728571428571428,
0.742857142857142,0.757142857142856,0.771428571428571,0.785714285714285,
0.799999999999999,0.814285714285713,0.828571428571428,0.842857142857142,
0.857142857142856,0.87142857142857,0.885714285714284,0.899999999999999,
0.914285714285713,0.928571428571427,0.942857142857141,0.957142857142856,
0.97142857142857,0.985714285714284,1.),(0.,1.8),.UNSPECIFIED.);
#981=B_SPLINE_SURFACE_WITH_KNOTS('',5,1,((#29707,#29708),(#29709,#29710),
(#29711,#29712),(#29713,#29714),(#29715,#29716),(#29717,#29718),(#29719,
#29720),(#29721,#29722),(#29723,#29724),(#29725,#29726),(#29727,#29728),
(#29729,#29730),(#29731,#29732),(#29733,#29734),(#29735,#29736),(#29737,
#29738),(#29739,#29740),(#29741,#29742),(#29743,#29744),(#29745,#29746),
(#29747,#29748),(#29749,#29750),(#29751,#29752),(#29753,#29754),(#29755,
#29756),(#29757,#29758),(#29759,#29760),(#29761,#29762),(#29763,#29764),
(#29765,#29766),(#29767,#29768),(#29769,#29770),(#29771,#29772),(#29773,
#29774),(#29775,#29776),(#29777,#29778),(#29779,#29780),(#29781,#29782),
(#29783,#29784),(#29785,#29786),(#29787,#29788),(#29789,#29790),(#29791,
#29792),(#29793,#29794),(#29795,#29796),(#29797,#29798),(#29799,#29800),
(#29801,#29802),(#29803,#29804),(#29805,#29806),(#29807,#29808),(#29809,
#29810),(#29811,#29812),(#29813,#29814),(#29815,#29816),(#29817,#29818),
(#29819,#29820),(#29821,#29822),(#29823,#29824),(#29825,#29826),(#29827,
#29828),(#29829,#29830),(#29831,#29832),(#29833,#29834),(#29835,#29836),
(#29837,#29838),(#29839,#29840),(#29841,#29842),(#29843,#29844),(#29845,
#29846),(#29847,#29848),(#29849,#29850),(#29851,#29852),(#29853,#29854),
(#29855,#29856)),.UNSPECIFIED.,.F.,.F.,.F.,(6,1,1,1,1,1,1,1,1,1,1,1,1,1,
1,1,1,1,1,1,1,1,1,1,1,1,1,1,1,1,1,1,1,1,1,1,1,1,1,1,1,1,1,1,1,1,1,1,1,1,
1,1,1,1,1,1,1,1,1,1,1,1,1,1,1,1,1,1,1,1,6),(2,2),(-1.,-0.985714285714284,
-0.97142857142857,-0.957142857142856,-0.942857142857141,-0.928571428571427,
-0.914285714285713,-0.899999999999999,-0.885714285714284,-0.87142857142857,
-0.857142857142856,-0.842857142857142,-0.828571428571428,-0.814285714285713,
-0.799999999999999,-0.785714285714285,-0.771428571428571,-0.757142857142856,
-0.742857142857142,-0.728571428571428,-0.714285714285714,-0.699999999999999,
-0.685714285714285,-0.671428571428571,-0.657142857142857,-0.642857142857142,
-0.628571428571428,-0.614285714285714,-0.6,-0.585714285714286,-0.571428571428571,
-0.557142857142857,-0.542857142857143,-0.528571428571429,-0.514285714285714,
-0.5,-0.485714285714286,-0.471428571428572,-0.457142857142857,-0.442857142857143,
-0.428571428571429,-0.414285714285714,-0.4,-0.385714285714286,-0.371428571428571,
-0.357142857142857,-0.342857142857143,-0.328571428571429,-0.314285714285714,
-0.3,-0.285714285714286,-0.271428571428571,-0.257142857142857,-0.242857142857143,
-0.228571428571429,-0.214285714285714,-0.2,-0.185714285714286,-0.171428571428571,
-0.157142857142857,-0.142857142857143,-0.128571428571429,-0.114285714285714,
-0.1,-0.0857142857142857,-0.0714285714285714,-0.0571428571428571,-0.0428571428571429,
-0.0285714285714286,-0.0142857142857143,0.),(0.,1.8),.UNSPECIFIED.);
#982=B_SPLINE_SURFACE_WITH_KNOTS('',5,1,((#30015,#30016),(#30017,#30018),
(#30019,#30020),(#30021,#30022),(#30023,#30024),(#30025,#30026),(#30027,
#30028),(#30029,#30030),(#30031,#30032),(#30033,#30034),(#30035,#30036),
(#30037,#30038),(#30039,#30040),(#30041,#30042),(#30043,#30044),(#30045,
#30046),(#30047,#30048),(#30049,#30050),(#30051,#30052),(#30053,#30054),
(#30055,#30056),(#30057,#30058),(#30059,#30060),(#30061,#30062),(#30063,
#30064),(#30065,#30066),(#30067,#30068),(#30069,#30070),(#30071,#30072),
(#30073,#30074),(#30075,#30076),(#30077,#30078),(#30079,#30080),(#30081,
#30082),(#30083,#30084),(#30085,#30086),(#30087,#30088),(#30089,#30090),
(#30091,#30092),(#30093,#30094),(#30095,#30096),(#30097,#30098),(#30099,
#30100),(#30101,#30102),(#30103,#30104),(#30105,#30106),(#30107,#30108),
(#30109,#30110),(#30111,#30112),(#30113,#30114),(#30115,#30116),(#30117,
#30118),(#30119,#30120),(#30121,#30122),(#30123,#30124),(#30125,#30126),
(#30127,#30128),(#30129,#30130),(#30131,#30132),(#30133,#30134),(#30135,
#30136),(#30137,#30138),(#30139,#30140),(#30141,#30142),(#30143,#30144),
(#30145,#30146),(#30147,#30148),(#30149,#30150),(#30151,#30152),(#30153,
#30154),(#30155,#30156),(#30157,#30158),(#30159,#30160),(#30161,#30162),
(#30163,#30164)),.UNSPECIFIED.,.F.,.F.,.F.,(6,1,1,1,1,1,1,1,1,1,1,1,1,1,
1,1,1,1,1,1,1,1,1,1,1,1,1,1,1,1,1,1,1,1,1,1,1,1,1,1,1,1,1,1,1,1,1,1,1,1,
1,1,1,1,1,1,1,1,1,1,1,1,1,1,1,1,1,1,1,1,6),(2,2),(0.,0.0142857142857143,
0.0285714285714286,0.0428571428571429,0.0571428571428571,0.0714285714285714,
0.0857142857142857,0.1,0.114285714285714,0.128571428571429,0.142857142857143,
0.157142857142857,0.171428571428571,0.185714285714286,0.2,0.214285714285714,
0.228571428571429,0.242857142857143,0.257142857142857,0.271428571428571,
0.285714285714286,0.3,0.314285714285714,0.328571428571429,0.342857142857143,
0.357142857142857,0.371428571428571,0.385714285714286,0.4,0.414285714285714,
0.428571428571429,0.442857142857143,0.457142857142857,0.471428571428572,
0.485714285714286,0.5,0.514285714285714,0.528571428571429,0.542857142857143,
0.557142857142857,0.571428571428571,0.585714285714286,0.6,0.614285714285714,
0.628571428571428,0.642857142857142,0.657142857142857,0.671428571428571,
0.685714285714285,0.699999999999999,0.714285714285714,0.728571428571428,
0.742857142857142,0.757142857142856,0.771428571428571,0.785714285714285,
0.799999999999999,0.814285714285713,0.828571428571428,0.842857142857142,
0.857142857142856,0.87142857142857,0.885714285714284,0.899999999999999,
0.914285714285713,0.928571428571427,0.942857142857141,0.957142857142856,
0.97142857142857,0.985714285714284,1.),(0.,1.8),.UNSPECIFIED.);
#983=B_SPLINE_SURFACE_WITH_KNOTS('',5,1,((#30313,#30314),(#30315,#30316),
(#30317,#30318),(#30319,#30320),(#30321,#30322),(#30323,#30324),(#30325,
#30326),(#30327,#30328),(#30329,#30330),(#30331,#30332),(#30333,#30334),
(#30335,#30336),(#30337,#30338),(#30339,#30340),(#30341,#30342),(#30343,
#30344),(#30345,#30346),(#30347,#30348),(#30349,#30350),(#30351,#30352),
(#30353,#30354),(#30355,#30356),(#30357,#30358),(#30359,#30360),(#30361,
#30362),(#30363,#30364),(#30365,#30366),(#30367,#30368),(#30369,#30370),
(#30371,#30372),(#30373,#30374),(#30375,#30376),(#30377,#30378),(#30379,
#30380),(#30381,#30382),(#30383,#30384),(#30385,#30386),(#30387,#30388),
(#30389,#30390),(#30391,#30392),(#30393,#30394),(#30395,#30396),(#30397,
#30398),(#30399,#30400),(#30401,#30402),(#30403,#30404),(#30405,#30406),
(#30407,#30408),(#30409,#30410),(#30411,#30412),(#30413,#30414),(#30415,
#30416),(#30417,#30418),(#30419,#30420),(#30421,#30422),(#30423,#30424),
(#30425,#30426),(#30427,#30428),(#30429,#30430),(#30431,#30432),(#30433,
#30434),(#30435,#30436),(#30437,#30438),(#30439,#30440),(#30441,#30442),
(#30443,#30444),(#30445,#30446),(#30447,#30448),(#30449,#30450),(#30451,
#30452),(#30453,#30454),(#30455,#30456),(#30457,#30458),(#30459,#30460),
(#30461,#30462)),.UNSPECIFIED.,.F.,.F.,.F.,(6,1,1,1,1,1,1,1,1,1,1,1,1,1,
1,1,1,1,1,1,1,1,1,1,1,1,1,1,1,1,1,1,1,1,1,1,1,1,1,1,1,1,1,1,1,1,1,1,1,1,
1,1,1,1,1,1,1,1,1,1,1,1,1,1,1,1,1,1,1,1,6),(2,2),(-1.,-0.985714285714284,
-0.97142857142857,-0.957142857142856,-0.942857142857141,-0.928571428571427,
-0.914285714285713,-0.899999999999999,-0.885714285714284,-0.87142857142857,
-0.857142857142856,-0.842857142857142,-0.828571428571428,-0.814285714285713,
-0.799999999999999,-0.785714285714285,-0.771428571428571,-0.757142857142856,
-0.742857142857142,-0.728571428571428,-0.714285714285714,-0.699999999999999,
-0.685714285714285,-0.671428571428571,-0.657142857142857,-0.642857142857142,
-0.628571428571428,-0.614285714285714,-0.6,-0.585714285714286,-0.571428571428571,
-0.557142857142857,-0.542857142857143,-0.528571428571429,-0.514285714285714,
-0.5,-0.485714285714286,-0.471428571428572,-0.457142857142857,-0.442857142857143,
-0.428571428571429,-0.414285714285714,-0.4,-0.385714285714286,-0.371428571428571,
-0.357142857142857,-0.342857142857143,-0.328571428571429,-0.314285714285714,
-0.3,-0.285714285714286,-0.271428571428571,-0.257142857142857,-0.242857142857143,
-0.228571428571429,-0.214285714285714,-0.2,-0.185714285714286,-0.171428571428571,
-0.157142857142857,-0.142857142857143,-0.128571428571429,-0.114285714285714,
-0.1,-0.0857142857142857,-0.0714285714285714,-0.0571428571428571,-0.0428571428571429,
-0.0285714285714286,-0.0142857142857143,0.),(0.,1.8),.UNSPECIFIED.);
#984=B_SPLINE_SURFACE_WITH_KNOTS('',5,1,((#30621,#30622),(#30623,#30624),
(#30625,#30626),(#30627,#30628),(#30629,#30630),(#30631,#30632),(#30633,
#30634),(#30635,#30636),(#30637,#30638),(#30639,#30640),(#30641,#30642),
(#30643,#30644),(#30645,#30646),(#30647,#30648),(#30649,#30650),(#30651,
#30652),(#30653,#30654),(#30655,#30656),(#30657,#30658),(#30659,#30660),
(#30661,#30662),(#30663,#30664),(#30665,#30666),(#30667,#30668),(#30669,
#30670),(#30671,#30672),(#30673,#30674),(#30675,#30676),(#30677,#30678),
(#30679,#30680),(#30681,#30682),(#30683,#30684),(#30685,#30686),(#30687,
#30688),(#30689,#30690),(#30691,#30692),(#30693,#30694),(#30695,#30696),
(#30697,#30698),(#30699,#30700),(#30701,#30702),(#30703,#30704),(#30705,
#30706),(#30707,#30708),(#30709,#30710),(#30711,#30712),(#30713,#30714),
(#30715,#30716),(#30717,#30718),(#30719,#30720),(#30721,#30722),(#30723,
#30724),(#30725,#30726),(#30727,#30728),(#30729,#30730),(#30731,#30732),
(#30733,#30734),(#30735,#30736),(#30737,#30738),(#30739,#30740),(#30741,
#30742),(#30743,#30744),(#30745,#30746),(#30747,#30748),(#30749,#30750),
(#30751,#30752),(#30753,#30754),(#30755,#30756),(#30757,#30758),(#30759,
#30760),(#30761,#30762),(#30763,#30764),(#30765,#30766),(#30767,#30768),
(#30769,#30770)),.UNSPECIFIED.,.F.,.F.,.F.,(6,1,1,1,1,1,1,1,1,1,1,1,1,1,
1,1,1,1,1,1,1,1,1,1,1,1,1,1,1,1,1,1,1,1,1,1,1,1,1,1,1,1,1,1,1,1,1,1,1,1,
1,1,1,1,1,1,1,1,1,1,1,1,1,1,1,1,1,1,1,1,6),(2,2),(0.,0.0142857142857143,
0.0285714285714286,0.0428571428571429,0.0571428571428571,0.0714285714285714,
0.0857142857142857,0.1,0.114285714285714,0.128571428571429,0.142857142857143,
0.157142857142857,0.171428571428571,0.185714285714286,0.2,0.214285714285714,
0.228571428571429,0.242857142857143,0.257142857142857,0.271428571428571,
0.285714285714286,0.3,0.314285714285714,0.328571428571429,0.342857142857143,
0.357142857142857,0.371428571428571,0.385714285714286,0.4,0.414285714285714,
0.428571428571429,0.442857142857143,0.457142857142857,0.471428571428572,
0.485714285714286,0.5,0.514285714285714,0.528571428571429,0.542857142857143,
0.557142857142857,0.571428571428571,0.585714285714286,0.6,0.614285714285714,
0.628571428571428,0.642857142857142,0.657142857142857,0.671428571428571,
0.685714285714285,0.699999999999999,0.714285714285714,0.728571428571428,
0.742857142857142,0.757142857142856,0.771428571428571,0.785714285714285,
0.799999999999999,0.814285714285713,0.828571428571428,0.842857142857142,
0.857142857142856,0.87142857142857,0.885714285714284,0.899999999999999,
0.914285714285713,0.928571428571427,0.942857142857141,0.957142857142856,
0.97142857142857,0.985714285714284,1.),(0.,1.8),.UNSPECIFIED.);
#985=B_SPLINE_SURFACE_WITH_KNOTS('',5,1,((#31313,#31314),(#31315,#31316),
(#31317,#31318),(#31319,#31320),(#31321,#31322),(#31323,#31324),(#31325,
#31326),(#31327,#31328),(#31329,#31330),(#31331,#31332),(#31333,#31334),
(#31335,#31336),(#31337,#31338),(#31339,#31340),(#31341,#31342),(#31343,
#31344),(#31345,#31346),(#31347,#31348),(#31349,#31350),(#31351,#31352),
(#31353,#31354),(#31355,#31356),(#31357,#31358),(#31359,#31360),(#31361,
#31362),(#31363,#31364),(#31365,#31366),(#31367,#31368),(#31369,#31370),
(#31371,#31372),(#31373,#31374),(#31375,#31376),(#31377,#31378),(#31379,
#31380),(#31381,#31382),(#31383,#31384),(#31385,#31386),(#31387,#31388),
(#31389,#31390),(#31391,#31392),(#31393,#31394),(#31395,#31396),(#31397,
#31398),(#31399,#31400),(#31401,#31402),(#31403,#31404),(#31405,#31406),
(#31407,#31408),(#31409,#31410),(#31411,#31412),(#31413,#31414),(#31415,
#31416),(#31417,#31418),(#31419,#31420),(#31421,#31422),(#31423,#31424),
(#31425,#31426),(#31427,#31428),(#31429,#31430),(#31431,#31432),(#31433,
#31434),(#31435,#31436),(#31437,#31438),(#31439,#31440),(#31441,#31442),
(#31443,#31444),(#31445,#31446),(#31447,#31448),(#31449,#31450),(#31451,
#31452),(#31453,#31454),(#31455,#31456),(#31457,#31458),(#31459,#31460),
(#31461,#31462)),.UNSPECIFIED.,.F.,.F.,.F.,(6,1,1,1,1,1,1,1,1,1,1,1,1,1,
1,1,1,1,1,1,1,1,1,1,1,1,1,1,1,1,1,1,1,1,1,1,1,1,1,1,1,1,1,1,1,1,1,1,1,1,
1,1,1,1,1,1,1,1,1,1,1,1,1,1,1,1,1,1,1,1,6),(2,2),(-1.,-0.985714285714284,
-0.97142857142857,-0.957142857142856,-0.942857142857141,-0.928571428571427,
-0.914285714285713,-0.899999999999999,-0.885714285714284,-0.87142857142857,
-0.857142857142856,-0.842857142857142,-0.828571428571428,-0.814285714285713,
-0.799999999999999,-0.785714285714285,-0.771428571428571,-0.757142857142856,
-0.742857142857142,-0.728571428571428,-0.714285714285714,-0.699999999999999,
-0.685714285714285,-0.671428571428571,-0.657142857142857,-0.642857142857142,
-0.628571428571428,-0.614285714285714,-0.6,-0.585714285714286,-0.571428571428571,
-0.557142857142857,-0.542857142857143,-0.528571428571429,-0.514285714285714,
-0.5,-0.485714285714286,-0.471428571428572,-0.457142857142857,-0.442857142857143,
-0.428571428571429,-0.414285714285714,-0.4,-0.385714285714286,-0.371428571428571,
-0.357142857142857,-0.342857142857143,-0.328571428571429,-0.314285714285714,
-0.3,-0.285714285714286,-0.271428571428571,-0.257142857142857,-0.242857142857143,
-0.228571428571429,-0.214285714285714,-0.2,-0.185714285714286,-0.171428571428571,
-0.157142857142857,-0.142857142857143,-0.128571428571429,-0.114285714285714,
-0.1,-0.0857142857142857,-0.0714285714285714,-0.0571428571428571,-0.0428571428571429,
-0.0285714285714286,-0.0142857142857143,0.),(0.,1.8),.UNSPECIFIED.);
#986=B_SPLINE_SURFACE_WITH_KNOTS('',5,1,((#31466,#31467),(#31468,#31469),
(#31470,#31471),(#31472,#31473),(#31474,#31475),(#31476,#31477),(#31478,
#31479),(#31480,#31481),(#31482,#31483),(#31484,#31485),(#31486,#31487),
(#31488,#31489),(#31490,#31491),(#31492,#31493),(#31494,#31495),(#31496,
#31497),(#31498,#31499),(#31500,#31501),(#31502,#31503),(#31504,#31505),
(#31506,#31507),(#31508,#31509),(#31510,#31511),(#31512,#31513),(#31514,
#31515),(#31516,#31517),(#31518,#31519),(#31520,#31521),(#31522,#31523),
(#31524,#31525),(#31526,#31527),(#31528,#31529),(#31530,#31531),(#31532,
#31533),(#31534,#31535),(#31536,#31537),(#31538,#31539),(#31540,#31541),
(#31542,#31543),(#31544,#31545),(#31546,#31547),(#31548,#31549),(#31550,
#31551),(#31552,#31553),(#31554,#31555),(#31556,#31557),(#31558,#31559),
(#31560,#31561),(#31562,#31563),(#31564,#31565),(#31566,#31567),(#31568,
#31569),(#31570,#31571),(#31572,#31573),(#31574,#31575),(#31576,#31577),
(#31578,#31579),(#31580,#31581),(#31582,#31583),(#31584,#31585),(#31586,
#31587),(#31588,#31589),(#31590,#31591),(#31592,#31593),(#31594,#31595),
(#31596,#31597),(#31598,#31599),(#31600,#31601),(#31602,#31603),(#31604,
#31605),(#31606,#31607),(#31608,#31609),(#31610,#31611),(#31612,#31613),
(#31614,#31615)),.UNSPECIFIED.,.F.,.F.,.F.,(6,1,1,1,1,1,1,1,1,1,1,1,1,1,
1,1,1,1,1,1,1,1,1,1,1,1,1,1,1,1,1,1,1,1,1,1,1,1,1,1,1,1,1,1,1,1,1,1,1,1,
1,1,1,1,1,1,1,1,1,1,1,1,1,1,1,1,1,1,1,1,6),(2,2),(0.,0.0142857142857143,
0.0285714285714286,0.0428571428571429,0.0571428571428571,0.0714285714285714,
0.0857142857142857,0.1,0.114285714285714,0.128571428571429,0.142857142857143,
0.157142857142857,0.171428571428571,0.185714285714286,0.2,0.214285714285714,
0.228571428571429,0.242857142857143,0.257142857142857,0.271428571428571,
0.285714285714286,0.3,0.314285714285714,0.328571428571429,0.342857142857143,
0.357142857142857,0.371428571428571,0.385714285714286,0.4,0.414285714285714,
0.428571428571429,0.442857142857143,0.457142857142857,0.471428571428572,
0.485714285714286,0.5,0.514285714285714,0.528571428571429,0.542857142857143,
0.557142857142857,0.571428571428571,0.585714285714286,0.6,0.614285714285714,
0.628571428571428,0.642857142857142,0.657142857142857,0.671428571428571,
0.685714285714285,0.699999999999999,0.714285714285714,0.728571428571428,
0.742857142857142,0.757142857142856,0.771428571428571,0.785714285714285,
0.799999999999999,0.814285714285713,0.828571428571428,0.842857142857142,
0.857142857142856,0.87142857142857,0.885714285714284,0.899999999999999,
0.914285714285713,0.928571428571427,0.942857142857141,0.957142857142856,
0.97142857142857,0.985714285714284,1.),(0.,1.8),.UNSPECIFIED.);
#987=B_SPLINE_SURFACE_WITH_KNOTS('',5,1,((#31902,#31903),(#31904,#31905),
(#31906,#31907),(#31908,#31909),(#31910,#31911),(#31912,#31913),(#31914,
#31915),(#31916,#31917),(#31918,#31919),(#31920,#31921),(#31922,#31923),
(#31924,#31925),(#31926,#31927),(#31928,#31929),(#31930,#31931),(#31932,
#31933),(#31934,#31935),(#31936,#31937),(#31938,#31939),(#31940,#31941),
(#31942,#31943),(#31944,#31945),(#31946,#31947),(#31948,#31949),(#31950,
#31951),(#31952,#31953),(#31954,#31955),(#31956,#31957),(#31958,#31959),
(#31960,#31961),(#31962,#31963),(#31964,#31965),(#31966,#31967),(#31968,
#31969),(#31970,#31971),(#31972,#31973),(#31974,#31975),(#31976,#31977),
(#31978,#31979),(#31980,#31981),(#31982,#31983),(#31984,#31985),(#31986,
#31987),(#31988,#31989),(#31990,#31991),(#31992,#31993),(#31994,#31995),
(#31996,#31997),(#31998,#31999),(#32000,#32001),(#32002,#32003),(#32004,
#32005),(#32006,#32007),(#32008,#32009),(#32010,#32011),(#32012,#32013),
(#32014,#32015),(#32016,#32017),(#32018,#32019),(#32020,#32021),(#32022,
#32023),(#32024,#32025),(#32026,#32027),(#32028,#32029),(#32030,#32031),
(#32032,#32033),(#32034,#32035),(#32036,#32037),(#32038,#32039),(#32040,
#32041),(#32042,#32043),(#32044,#32045),(#32046,#32047),(#32048,#32049),
(#32050,#32051)),.UNSPECIFIED.,.F.,.F.,.F.,(6,1,1,1,1,1,1,1,1,1,1,1,1,1,
1,1,1,1,1,1,1,1,1,1,1,1,1,1,1,1,1,1,1,1,1,1,1,1,1,1,1,1,1,1,1,1,1,1,1,1,
1,1,1,1,1,1,1,1,1,1,1,1,1,1,1,1,1,1,1,1,6),(2,2),(-1.,-0.985714285714284,
-0.97142857142857,-0.957142857142856,-0.942857142857141,-0.928571428571427,
-0.914285714285713,-0.899999999999999,-0.885714285714284,-0.87142857142857,
-0.857142857142856,-0.842857142857142,-0.828571428571428,-0.814285714285713,
-0.799999999999999,-0.785714285714285,-0.771428571428571,-0.757142857142856,
-0.742857142857142,-0.728571428571428,-0.714285714285714,-0.699999999999999,
-0.685714285714285,-0.671428571428571,-0.657142857142857,-0.642857142857142,
-0.628571428571428,-0.614285714285714,-0.6,-0.585714285714286,-0.571428571428571,
-0.557142857142857,-0.542857142857143,-0.528571428571429,-0.514285714285714,
-0.5,-0.485714285714286,-0.471428571428572,-0.457142857142857,-0.442857142857143,
-0.428571428571429,-0.414285714285714,-0.4,-0.385714285714286,-0.371428571428571,
-0.357142857142857,-0.342857142857143,-0.328571428571429,-0.314285714285714,
-0.3,-0.285714285714286,-0.271428571428571,-0.257142857142857,-0.242857142857143,
-0.228571428571429,-0.214285714285714,-0.2,-0.185714285714286,-0.171428571428571,
-0.157142857142857,-0.142857142857143,-0.128571428571429,-0.114285714285714,
-0.1,-0.0857142857142857,-0.0714285714285714,-0.0571428571428571,-0.0428571428571429,
-0.0285714285714286,-0.0142857142857143,0.),(0.,1.8),.UNSPECIFIED.);
#988=B_SPLINE_SURFACE_WITH_KNOTS('',5,1,((#32210,#32211),(#32212,#32213),
(#32214,#32215),(#32216,#32217),(#32218,#32219),(#32220,#32221),(#32222,
#32223),(#32224,#32225),(#32226,#32227),(#32228,#32229),(#32230,#32231),
(#32232,#32233),(#32234,#32235),(#32236,#32237),(#32238,#32239),(#32240,
#32241),(#32242,#32243),(#32244,#32245),(#32246,#32247),(#32248,#32249),
(#32250,#32251),(#32252,#32253),(#32254,#32255),(#32256,#32257),(#32258,
#32259),(#32260,#32261),(#32262,#32263),(#32264,#32265),(#32266,#32267),
(#32268,#32269),(#32270,#32271),(#32272,#32273),(#32274,#32275),(#32276,
#32277),(#32278,#32279),(#32280,#32281),(#32282,#32283),(#32284,#32285),
(#32286,#32287),(#32288,#32289),(#32290,#32291),(#32292,#32293),(#32294,
#32295),(#32296,#32297),(#32298,#32299),(#32300,#32301),(#32302,#32303),
(#32304,#32305),(#32306,#32307),(#32308,#32309),(#32310,#32311),(#32312,
#32313),(#32314,#32315),(#32316,#32317),(#32318,#32319),(#32320,#32321),
(#32322,#32323),(#32324,#32325),(#32326,#32327),(#32328,#32329),(#32330,
#32331),(#32332,#32333),(#32334,#32335),(#32336,#32337),(#32338,#32339),
(#32340,#32341),(#32342,#32343),(#32344,#32345),(#32346,#32347),(#32348,
#32349),(#32350,#32351),(#32352,#32353),(#32354,#32355),(#32356,#32357),
(#32358,#32359)),.UNSPECIFIED.,.F.,.F.,.F.,(6,1,1,1,1,1,1,1,1,1,1,1,1,1,
1,1,1,1,1,1,1,1,1,1,1,1,1,1,1,1,1,1,1,1,1,1,1,1,1,1,1,1,1,1,1,1,1,1,1,1,
1,1,1,1,1,1,1,1,1,1,1,1,1,1,1,1,1,1,1,1,6),(2,2),(0.,0.0142857142857143,
0.0285714285714286,0.0428571428571429,0.0571428571428571,0.0714285714285714,
0.0857142857142857,0.1,0.114285714285714,0.128571428571429,0.142857142857143,
0.157142857142857,0.171428571428571,0.185714285714286,0.2,0.214285714285714,
0.228571428571429,0.242857142857143,0.257142857142857,0.271428571428571,
0.285714285714286,0.3,0.314285714285714,0.328571428571429,0.342857142857143,
0.357142857142857,0.371428571428571,0.385714285714286,0.4,0.414285714285714,
0.428571428571429,0.442857142857143,0.457142857142857,0.471428571428572,
0.485714285714286,0.5,0.514285714285714,0.528571428571429,0.542857142857143,
0.557142857142857,0.571428571428571,0.585714285714286,0.6,0.614285714285714,
0.628571428571428,0.642857142857142,0.657142857142857,0.671428571428571,
0.685714285714285,0.699999999999999,0.714285714285714,0.728571428571428,
0.742857142857142,0.757142857142856,0.771428571428571,0.785714285714285,
0.799999999999999,0.814285714285713,0.828571428571428,0.842857142857142,
0.857142857142856,0.87142857142857,0.885714285714284,0.899999999999999,
0.914285714285713,0.928571428571427,0.942857142857141,0.957142857142856,
0.97142857142857,0.985714285714284,1.),(0.,1.8),.UNSPECIFIED.);
#989=B_SPLINE_SURFACE_WITH_KNOTS('',5,1,((#32508,#32509),(#32510,#32511),
(#32512,#32513),(#32514,#32515),(#32516,#32517),(#32518,#32519),(#32520,
#32521),(#32522,#32523),(#32524,#32525),(#32526,#32527),(#32528,#32529),
(#32530,#32531),(#32532,#32533),(#32534,#32535),(#32536,#32537),(#32538,
#32539),(#32540,#32541),(#32542,#32543),(#32544,#32545),(#32546,#32547),
(#32548,#32549),(#32550,#32551),(#32552,#32553),(#32554,#32555),(#32556,
#32557),(#32558,#32559),(#32560,#32561),(#32562,#32563),(#32564,#32565),
(#32566,#32567),(#32568,#32569),(#32570,#32571),(#32572,#32573),(#32574,
#32575),(#32576,#32577),(#32578,#32579),(#32580,#32581),(#32582,#32583),
(#32584,#32585),(#32586,#32587),(#32588,#32589),(#32590,#32591),(#32592,
#32593),(#32594,#32595),(#32596,#32597),(#32598,#32599),(#32600,#32601),
(#32602,#32603),(#32604,#32605),(#32606,#32607),(#32608,#32609),(#32610,
#32611),(#32612,#32613),(#32614,#32615),(#32616,#32617),(#32618,#32619),
(#32620,#32621),(#32622,#32623),(#32624,#32625),(#32626,#32627),(#32628,
#32629),(#32630,#32631),(#32632,#32633),(#32634,#32635),(#32636,#32637),
(#32638,#32639),(#32640,#32641),(#32642,#32643),(#32644,#32645),(#32646,
#32647),(#32648,#32649),(#32650,#32651),(#32652,#32653),(#32654,#32655),
(#32656,#32657)),.UNSPECIFIED.,.F.,.F.,.F.,(6,1,1,1,1,1,1,1,1,1,1,1,1,1,
1,1,1,1,1,1,1,1,1,1,1,1,1,1,1,1,1,1,1,1,1,1,1,1,1,1,1,1,1,1,1,1,1,1,1,1,
1,1,1,1,1,1,1,1,1,1,1,1,1,1,1,1,1,1,1,1,6),(2,2),(-1.,-0.985714285714284,
-0.97142857142857,-0.957142857142856,-0.942857142857141,-0.928571428571427,
-0.914285714285713,-0.899999999999999,-0.885714285714284,-0.87142857142857,
-0.857142857142856,-0.842857142857142,-0.828571428571428,-0.814285714285713,
-0.799999999999999,-0.785714285714285,-0.771428571428571,-0.757142857142856,
-0.742857142857142,-0.728571428571428,-0.714285714285714,-0.699999999999999,
-0.685714285714285,-0.671428571428571,-0.657142857142857,-0.642857142857142,
-0.628571428571428,-0.614285714285714,-0.6,-0.585714285714286,-0.571428571428571,
-0.557142857142857,-0.542857142857143,-0.528571428571429,-0.514285714285714,
-0.5,-0.485714285714286,-0.471428571428572,-0.457142857142857,-0.442857142857143,
-0.428571428571429,-0.414285714285714,-0.4,-0.385714285714286,-0.371428571428571,
-0.357142857142857,-0.342857142857143,-0.328571428571429,-0.314285714285714,
-0.3,-0.285714285714286,-0.271428571428571,-0.257142857142857,-0.242857142857143,
-0.228571428571429,-0.214285714285714,-0.2,-0.185714285714286,-0.171428571428571,
-0.157142857142857,-0.142857142857143,-0.128571428571429,-0.114285714285714,
-0.1,-0.0857142857142857,-0.0714285714285714,-0.0571428571428571,-0.0428571428571429,
-0.0285714285714286,-0.0142857142857143,0.),(0.,1.8),.UNSPECIFIED.);
#990=B_SPLINE_SURFACE_WITH_KNOTS('',5,1,((#32816,#32817),(#32818,#32819),
(#32820,#32821),(#32822,#32823),(#32824,#32825),(#32826,#32827),(#32828,
#32829),(#32830,#32831),(#32832,#32833),(#32834,#32835),(#32836,#32837),
(#32838,#32839),(#32840,#32841),(#32842,#32843),(#32844,#32845),(#32846,
#32847),(#32848,#32849),(#32850,#32851),(#32852,#32853),(#32854,#32855),
(#32856,#32857),(#32858,#32859),(#32860,#32861),(#32862,#32863),(#32864,
#32865),(#32866,#32867),(#32868,#32869),(#32870,#32871),(#32872,#32873),
(#32874,#32875),(#32876,#32877),(#32878,#32879),(#32880,#32881),(#32882,
#32883),(#32884,#32885),(#32886,#32887),(#32888,#32889),(#32890,#32891),
(#32892,#32893),(#32894,#32895),(#32896,#32897),(#32898,#32899),(#32900,
#32901),(#32902,#32903),(#32904,#32905),(#32906,#32907),(#32908,#32909),
(#32910,#32911),(#32912,#32913),(#32914,#32915),(#32916,#32917),(#32918,
#32919),(#32920,#32921),(#32922,#32923),(#32924,#32925),(#32926,#32927),
(#32928,#32929),(#32930,#32931),(#32932,#32933),(#32934,#32935),(#32936,
#32937),(#32938,#32939),(#32940,#32941),(#32942,#32943),(#32944,#32945),
(#32946,#32947),(#32948,#32949),(#32950,#32951),(#32952,#32953),(#32954,
#32955),(#32956,#32957),(#32958,#32959),(#32960,#32961),(#32962,#32963),
(#32964,#32965)),.UNSPECIFIED.,.F.,.F.,.F.,(6,1,1,1,1,1,1,1,1,1,1,1,1,1,
1,1,1,1,1,1,1,1,1,1,1,1,1,1,1,1,1,1,1,1,1,1,1,1,1,1,1,1,1,1,1,1,1,1,1,1,
1,1,1,1,1,1,1,1,1,1,1,1,1,1,1,1,1,1,1,1,6),(2,2),(0.,0.0142857142857143,
0.0285714285714286,0.0428571428571429,0.0571428571428571,0.0714285714285714,
0.0857142857142857,0.1,0.114285714285714,0.128571428571429,0.142857142857143,
0.157142857142857,0.171428571428571,0.185714285714286,0.2,0.214285714285714,
0.228571428571429,0.242857142857143,0.257142857142857,0.271428571428571,
0.285714285714286,0.3,0.314285714285714,0.328571428571429,0.342857142857143,
0.357142857142857,0.371428571428571,0.385714285714286,0.4,0.414285714285714,
0.428571428571429,0.442857142857143,0.457142857142857,0.471428571428572,
0.485714285714286,0.5,0.514285714285714,0.528571428571429,0.542857142857143,
0.557142857142857,0.571428571428571,0.585714285714286,0.6,0.614285714285714,
0.628571428571428,0.642857142857142,0.657142857142857,0.671428571428571,
0.685714285714285,0.699999999999999,0.714285714285714,0.728571428571428,
0.742857142857142,0.757142857142856,0.771428571428571,0.785714285714285,
0.799999999999999,0.814285714285713,0.828571428571428,0.842857142857142,
0.857142857142856,0.87142857142857,0.885714285714284,0.899999999999999,
0.914285714285713,0.928571428571427,0.942857142857141,0.957142857142856,
0.97142857142857,0.985714285714284,1.),(0.,1.8),.UNSPECIFIED.);
#991=B_SPLINE_SURFACE_WITH_KNOTS('',5,1,((#33114,#33115),(#33116,#33117),
(#33118,#33119),(#33120,#33121),(#33122,#33123),(#33124,#33125),(#33126,
#33127),(#33128,#33129),(#33130,#33131),(#33132,#33133),(#33134,#33135),
(#33136,#33137),(#33138,#33139),(#33140,#33141),(#33142,#33143),(#33144,
#33145),(#33146,#33147),(#33148,#33149),(#33150,#33151),(#33152,#33153),
(#33154,#33155),(#33156,#33157),(#33158,#33159),(#33160,#33161),(#33162,
#33163),(#33164,#33165),(#33166,#33167),(#33168,#33169),(#33170,#33171),
(#33172,#33173),(#33174,#33175),(#33176,#33177),(#33178,#33179),(#33180,
#33181),(#33182,#33183),(#33184,#33185),(#33186,#33187),(#33188,#33189),
(#33190,#33191),(#33192,#33193),(#33194,#33195),(#33196,#33197),(#33198,
#33199),(#33200,#33201),(#33202,#33203),(#33204,#33205),(#33206,#33207),
(#33208,#33209),(#33210,#33211),(#33212,#33213),(#33214,#33215),(#33216,
#33217),(#33218,#33219),(#33220,#33221),(#33222,#33223),(#33224,#33225),
(#33226,#33227),(#33228,#33229),(#33230,#33231),(#33232,#33233),(#33234,
#33235),(#33236,#33237),(#33238,#33239),(#33240,#33241),(#33242,#33243),
(#33244,#33245),(#33246,#33247),(#33248,#33249),(#33250,#33251),(#33252,
#33253),(#33254,#33255),(#33256,#33257),(#33258,#33259),(#33260,#33261),
(#33262,#33263)),.UNSPECIFIED.,.F.,.F.,.F.,(6,1,1,1,1,1,1,1,1,1,1,1,1,1,
1,1,1,1,1,1,1,1,1,1,1,1,1,1,1,1,1,1,1,1,1,1,1,1,1,1,1,1,1,1,1,1,1,1,1,1,
1,1,1,1,1,1,1,1,1,1,1,1,1,1,1,1,1,1,1,1,6),(2,2),(-1.,-0.985714285714284,
-0.97142857142857,-0.957142857142856,-0.942857142857141,-0.928571428571427,
-0.914285714285713,-0.899999999999999,-0.885714285714284,-0.87142857142857,
-0.857142857142856,-0.842857142857142,-0.828571428571428,-0.814285714285713,
-0.799999999999999,-0.785714285714285,-0.771428571428571,-0.757142857142856,
-0.742857142857142,-0.728571428571428,-0.714285714285714,-0.699999999999999,
-0.685714285714285,-0.671428571428571,-0.657142857142857,-0.642857142857142,
-0.628571428571428,-0.614285714285714,-0.6,-0.585714285714286,-0.571428571428571,
-0.557142857142857,-0.542857142857143,-0.528571428571429,-0.514285714285714,
-0.5,-0.485714285714286,-0.471428571428572,-0.457142857142857,-0.442857142857143,
-0.428571428571429,-0.414285714285714,-0.4,-0.385714285714286,-0.371428571428571,
-0.357142857142857,-0.342857142857143,-0.328571428571429,-0.314285714285714,
-0.3,-0.285714285714286,-0.271428571428571,-0.257142857142857,-0.242857142857143,
-0.228571428571429,-0.214285714285714,-0.2,-0.185714285714286,-0.171428571428571,
-0.157142857142857,-0.142857142857143,-0.128571428571429,-0.114285714285714,
-0.1,-0.0857142857142857,-0.0714285714285714,-0.0571428571428571,-0.0428571428571429,
-0.0285714285714286,-0.0142857142857143,0.),(0.,1.8),.UNSPECIFIED.);
#992=B_SPLINE_SURFACE_WITH_KNOTS('',5,1,((#33422,#33423),(#33424,#33425),
(#33426,#33427),(#33428,#33429),(#33430,#33431),(#33432,#33433),(#33434,
#33435),(#33436,#33437),(#33438,#33439),(#33440,#33441),(#33442,#33443),
(#33444,#33445),(#33446,#33447),(#33448,#33449),(#33450,#33451),(#33452,
#33453),(#33454,#33455),(#33456,#33457),(#33458,#33459),(#33460,#33461),
(#33462,#33463),(#33464,#33465),(#33466,#33467),(#33468,#33469),(#33470,
#33471),(#33472,#33473),(#33474,#33475),(#33476,#33477),(#33478,#33479),
(#33480,#33481),(#33482,#33483),(#33484,#33485),(#33486,#33487),(#33488,
#33489),(#33490,#33491),(#33492,#33493),(#33494,#33495),(#33496,#33497),
(#33498,#33499),(#33500,#33501),(#33502,#33503),(#33504,#33505),(#33506,
#33507),(#33508,#33509),(#33510,#33511),(#33512,#33513),(#33514,#33515),
(#33516,#33517),(#33518,#33519),(#33520,#33521),(#33522,#33523),(#33524,
#33525),(#33526,#33527),(#33528,#33529),(#33530,#33531),(#33532,#33533),
(#33534,#33535),(#33536,#33537),(#33538,#33539),(#33540,#33541),(#33542,
#33543),(#33544,#33545),(#33546,#33547),(#33548,#33549),(#33550,#33551),
(#33552,#33553),(#33554,#33555),(#33556,#33557),(#33558,#33559),(#33560,
#33561),(#33562,#33563),(#33564,#33565),(#33566,#33567),(#33568,#33569),
(#33570,#33571)),.UNSPECIFIED.,.F.,.F.,.F.,(6,1,1,1,1,1,1,1,1,1,1,1,1,1,
1,1,1,1,1,1,1,1,1,1,1,1,1,1,1,1,1,1,1,1,1,1,1,1,1,1,1,1,1,1,1,1,1,1,1,1,
1,1,1,1,1,1,1,1,1,1,1,1,1,1,1,1,1,1,1,1,6),(2,2),(0.,0.0142857142857143,
0.0285714285714286,0.0428571428571429,0.0571428571428571,0.0714285714285714,
0.0857142857142857,0.1,0.114285714285714,0.128571428571429,0.142857142857143,
0.157142857142857,0.171428571428571,0.185714285714286,0.2,0.214285714285714,
0.228571428571429,0.242857142857143,0.257142857142857,0.271428571428571,
0.285714285714286,0.3,0.314285714285714,0.328571428571429,0.342857142857143,
0.357142857142857,0.371428571428571,0.385714285714286,0.4,0.414285714285714,
0.428571428571429,0.442857142857143,0.457142857142857,0.471428571428572,
0.485714285714286,0.5,0.514285714285714,0.528571428571429,0.542857142857143,
0.557142857142857,0.571428571428571,0.585714285714286,0.6,0.614285714285714,
0.628571428571428,0.642857142857142,0.657142857142857,0.671428571428571,
0.685714285714285,0.699999999999999,0.714285714285714,0.728571428571428,
0.742857142857142,0.757142857142856,0.771428571428571,0.785714285714285,
0.799999999999999,0.814285714285713,0.828571428571428,0.842857142857142,
0.857142857142856,0.87142857142857,0.885714285714284,0.899999999999999,
0.914285714285713,0.928571428571427,0.942857142857141,0.957142857142856,
0.97142857142857,0.985714285714284,1.),(0.,1.8),.UNSPECIFIED.);
#993=B_SPLINE_SURFACE_WITH_KNOTS('',5,1,((#33720,#33721),(#33722,#33723),
(#33724,#33725),(#33726,#33727),(#33728,#33729),(#33730,#33731),(#33732,
#33733),(#33734,#33735),(#33736,#33737),(#33738,#33739),(#33740,#33741),
(#33742,#33743),(#33744,#33745),(#33746,#33747),(#33748,#33749),(#33750,
#33751),(#33752,#33753),(#33754,#33755),(#33756,#33757),(#33758,#33759),
(#33760,#33761),(#33762,#33763),(#33764,#33765),(#33766,#33767),(#33768,
#33769),(#33770,#33771),(#33772,#33773),(#33774,#33775),(#33776,#33777),
(#33778,#33779),(#33780,#33781),(#33782,#33783),(#33784,#33785),(#33786,
#33787),(#33788,#33789),(#33790,#33791),(#33792,#33793),(#33794,#33795),
(#33796,#33797),(#33798,#33799),(#33800,#33801),(#33802,#33803),(#33804,
#33805),(#33806,#33807),(#33808,#33809),(#33810,#33811),(#33812,#33813),
(#33814,#33815),(#33816,#33817),(#33818,#33819),(#33820,#33821),(#33822,
#33823),(#33824,#33825),(#33826,#33827),(#33828,#33829),(#33830,#33831),
(#33832,#33833),(#33834,#33835),(#33836,#33837),(#33838,#33839),(#33840,
#33841),(#33842,#33843),(#33844,#33845),(#33846,#33847),(#33848,#33849),
(#33850,#33851),(#33852,#33853),(#33854,#33855),(#33856,#33857),(#33858,
#33859),(#33860,#33861),(#33862,#33863),(#33864,#33865),(#33866,#33867),
(#33868,#33869)),.UNSPECIFIED.,.F.,.F.,.F.,(6,1,1,1,1,1,1,1,1,1,1,1,1,1,
1,1,1,1,1,1,1,1,1,1,1,1,1,1,1,1,1,1,1,1,1,1,1,1,1,1,1,1,1,1,1,1,1,1,1,1,
1,1,1,1,1,1,1,1,1,1,1,1,1,1,1,1,1,1,1,1,6),(2,2),(-1.,-0.985714285714284,
-0.97142857142857,-0.957142857142856,-0.942857142857141,-0.928571428571427,
-0.914285714285713,-0.899999999999999,-0.885714285714284,-0.87142857142857,
-0.857142857142856,-0.842857142857142,-0.828571428571428,-0.814285714285713,
-0.799999999999999,-0.785714285714285,-0.771428571428571,-0.757142857142856,
-0.742857142857142,-0.728571428571428,-0.714285714285714,-0.699999999999999,
-0.685714285714285,-0.671428571428571,-0.657142857142857,-0.642857142857142,
-0.628571428571428,-0.614285714285714,-0.6,-0.585714285714286,-0.571428571428571,
-0.557142857142857,-0.542857142857143,-0.528571428571429,-0.514285714285714,
-0.5,-0.485714285714286,-0.471428571428572,-0.457142857142857,-0.442857142857143,
-0.428571428571429,-0.414285714285714,-0.4,-0.385714285714286,-0.371428571428571,
-0.357142857142857,-0.342857142857143,-0.328571428571429,-0.314285714285714,
-0.3,-0.285714285714286,-0.271428571428571,-0.257142857142857,-0.242857142857143,
-0.228571428571429,-0.214285714285714,-0.2,-0.185714285714286,-0.171428571428571,
-0.157142857142857,-0.142857142857143,-0.128571428571429,-0.114285714285714,
-0.1,-0.0857142857142857,-0.0714285714285714,-0.0571428571428571,-0.0428571428571429,
-0.0285714285714286,-0.0142857142857143,0.),(0.,1.8),.UNSPECIFIED.);
#994=B_SPLINE_SURFACE_WITH_KNOTS('',5,1,((#34028,#34029),(#34030,#34031),
(#34032,#34033),(#34034,#34035),(#34036,#34037),(#34038,#34039),(#34040,
#34041),(#34042,#34043),(#34044,#34045),(#34046,#34047),(#34048,#34049),
(#34050,#34051),(#34052,#34053),(#34054,#34055),(#34056,#34057),(#34058,
#34059),(#34060,#34061),(#34062,#34063),(#34064,#34065),(#34066,#34067),
(#34068,#34069),(#34070,#34071),(#34072,#34073),(#34074,#34075),(#34076,
#34077),(#34078,#34079),(#34080,#34081),(#34082,#34083),(#34084,#34085),
(#34086,#34087),(#34088,#34089),(#34090,#34091),(#34092,#34093),(#34094,
#34095),(#34096,#34097),(#34098,#34099),(#34100,#34101),(#34102,#34103),
(#34104,#34105),(#34106,#34107),(#34108,#34109),(#34110,#34111),(#34112,
#34113),(#34114,#34115),(#34116,#34117),(#34118,#34119),(#34120,#34121),
(#34122,#34123),(#34124,#34125),(#34126,#34127),(#34128,#34129),(#34130,
#34131),(#34132,#34133),(#34134,#34135),(#34136,#34137),(#34138,#34139),
(#34140,#34141),(#34142,#34143),(#34144,#34145),(#34146,#34147),(#34148,
#34149),(#34150,#34151),(#34152,#34153),(#34154,#34155),(#34156,#34157),
(#34158,#34159),(#34160,#34161),(#34162,#34163),(#34164,#34165),(#34166,
#34167),(#34168,#34169),(#34170,#34171),(#34172,#34173),(#34174,#34175),
(#34176,#34177)),.UNSPECIFIED.,.F.,.F.,.F.,(6,1,1,1,1,1,1,1,1,1,1,1,1,1,
1,1,1,1,1,1,1,1,1,1,1,1,1,1,1,1,1,1,1,1,1,1,1,1,1,1,1,1,1,1,1,1,1,1,1,1,
1,1,1,1,1,1,1,1,1,1,1,1,1,1,1,1,1,1,1,1,6),(2,2),(0.,0.0142857142857143,
0.0285714285714286,0.0428571428571429,0.0571428571428571,0.0714285714285714,
0.0857142857142857,0.1,0.114285714285714,0.128571428571429,0.142857142857143,
0.157142857142857,0.171428571428571,0.185714285714286,0.2,0.214285714285714,
0.228571428571429,0.242857142857143,0.257142857142857,0.271428571428571,
0.285714285714286,0.3,0.314285714285714,0.328571428571429,0.342857142857143,
0.357142857142857,0.371428571428571,0.385714285714286,0.4,0.414285714285714,
0.428571428571429,0.442857142857143,0.457142857142857,0.471428571428572,
0.485714285714286,0.5,0.514285714285714,0.528571428571429,0.542857142857143,
0.557142857142857,0.571428571428571,0.585714285714286,0.6,0.614285714285714,
0.628571428571428,0.642857142857142,0.657142857142857,0.671428571428571,
0.685714285714285,0.699999999999999,0.714285714285714,0.728571428571428,
0.742857142857142,0.757142857142856,0.771428571428571,0.785714285714285,
0.799999999999999,0.814285714285713,0.828571428571428,0.842857142857142,
0.857142857142856,0.87142857142857,0.885714285714284,0.899999999999999,
0.914285714285713,0.928571428571427,0.942857142857141,0.957142857142856,
0.97142857142857,0.985714285714284,1.),(0.,1.8),.UNSPECIFIED.);
#995=B_SPLINE_SURFACE_WITH_KNOTS('',5,1,((#34326,#34327),(#34328,#34329),
(#34330,#34331),(#34332,#34333),(#34334,#34335),(#34336,#34337),(#34338,
#34339),(#34340,#34341),(#34342,#34343),(#34344,#34345),(#34346,#34347),
(#34348,#34349),(#34350,#34351),(#34352,#34353),(#34354,#34355),(#34356,
#34357),(#34358,#34359),(#34360,#34361),(#34362,#34363),(#34364,#34365),
(#34366,#34367),(#34368,#34369),(#34370,#34371),(#34372,#34373),(#34374,
#34375),(#34376,#34377),(#34378,#34379),(#34380,#34381),(#34382,#34383),
(#34384,#34385),(#34386,#34387),(#34388,#34389),(#34390,#34391),(#34392,
#34393),(#34394,#34395),(#34396,#34397),(#34398,#34399),(#34400,#34401),
(#34402,#34403),(#34404,#34405),(#34406,#34407),(#34408,#34409),(#34410,
#34411),(#34412,#34413),(#34414,#34415),(#34416,#34417),(#34418,#34419),
(#34420,#34421),(#34422,#34423),(#34424,#34425),(#34426,#34427),(#34428,
#34429),(#34430,#34431),(#34432,#34433),(#34434,#34435),(#34436,#34437),
(#34438,#34439),(#34440,#34441),(#34442,#34443),(#34444,#34445),(#34446,
#34447),(#34448,#34449),(#34450,#34451),(#34452,#34453),(#34454,#34455),
(#34456,#34457),(#34458,#34459),(#34460,#34461),(#34462,#34463),(#34464,
#34465),(#34466,#34467),(#34468,#34469),(#34470,#34471),(#34472,#34473),
(#34474,#34475)),.UNSPECIFIED.,.F.,.F.,.F.,(6,1,1,1,1,1,1,1,1,1,1,1,1,1,
1,1,1,1,1,1,1,1,1,1,1,1,1,1,1,1,1,1,1,1,1,1,1,1,1,1,1,1,1,1,1,1,1,1,1,1,
1,1,1,1,1,1,1,1,1,1,1,1,1,1,1,1,1,1,1,1,6),(2,2),(-1.,-0.985714285714284,
-0.97142857142857,-0.957142857142856,-0.942857142857141,-0.928571428571427,
-0.914285714285713,-0.899999999999999,-0.885714285714284,-0.87142857142857,
-0.857142857142856,-0.842857142857142,-0.828571428571428,-0.814285714285713,
-0.799999999999999,-0.785714285714285,-0.771428571428571,-0.757142857142856,
-0.742857142857142,-0.728571428571428,-0.714285714285714,-0.699999999999999,
-0.685714285714285,-0.671428571428571,-0.657142857142857,-0.642857142857142,
-0.628571428571428,-0.614285714285714,-0.6,-0.585714285714286,-0.571428571428571,
-0.557142857142857,-0.542857142857143,-0.528571428571429,-0.514285714285714,
-0.5,-0.485714285714286,-0.471428571428572,-0.457142857142857,-0.442857142857143,
-0.428571428571429,-0.414285714285714,-0.4,-0.385714285714286,-0.371428571428571,
-0.357142857142857,-0.342857142857143,-0.328571428571429,-0.314285714285714,
-0.3,-0.285714285714286,-0.271428571428571,-0.257142857142857,-0.242857142857143,
-0.228571428571429,-0.214285714285714,-0.2,-0.185714285714286,-0.171428571428571,
-0.157142857142857,-0.142857142857143,-0.128571428571429,-0.114285714285714,
-0.1,-0.0857142857142857,-0.0714285714285714,-0.0571428571428571,-0.0428571428571429,
-0.0285714285714286,-0.0142857142857143,0.),(0.,1.8),.UNSPECIFIED.);
#996=B_SPLINE_SURFACE_WITH_KNOTS('',5,1,((#34634,#34635),(#34636,#34637),
(#34638,#34639),(#34640,#34641),(#34642,#34643),(#34644,#34645),(#34646,
#34647),(#34648,#34649),(#34650,#34651),(#34652,#34653),(#34654,#34655),
(#34656,#34657),(#34658,#34659),(#34660,#34661),(#34662,#34663),(#34664,
#34665),(#34666,#34667),(#34668,#34669),(#34670,#34671),(#34672,#34673),
(#34674,#34675),(#34676,#34677),(#34678,#34679),(#34680,#34681),(#34682,
#34683),(#34684,#34685),(#34686,#34687),(#34688,#34689),(#34690,#34691),
(#34692,#34693),(#34694,#34695),(#34696,#34697),(#34698,#34699),(#34700,
#34701),(#34702,#34703),(#34704,#34705),(#34706,#34707),(#34708,#34709),
(#34710,#34711),(#34712,#34713),(#34714,#34715),(#34716,#34717),(#34718,
#34719),(#34720,#34721),(#34722,#34723),(#34724,#34725),(#34726,#34727),
(#34728,#34729),(#34730,#34731),(#34732,#34733),(#34734,#34735),(#34736,
#34737),(#34738,#34739),(#34740,#34741),(#34742,#34743),(#34744,#34745),
(#34746,#34747),(#34748,#34749),(#34750,#34751),(#34752,#34753),(#34754,
#34755),(#34756,#34757),(#34758,#34759),(#34760,#34761),(#34762,#34763),
(#34764,#34765),(#34766,#34767),(#34768,#34769),(#34770,#34771),(#34772,
#34773),(#34774,#34775),(#34776,#34777),(#34778,#34779),(#34780,#34781),
(#34782,#34783)),.UNSPECIFIED.,.F.,.F.,.F.,(6,1,1,1,1,1,1,1,1,1,1,1,1,1,
1,1,1,1,1,1,1,1,1,1,1,1,1,1,1,1,1,1,1,1,1,1,1,1,1,1,1,1,1,1,1,1,1,1,1,1,
1,1,1,1,1,1,1,1,1,1,1,1,1,1,1,1,1,1,1,1,6),(2,2),(0.,0.0142857142857143,
0.0285714285714286,0.0428571428571429,0.0571428571428571,0.0714285714285714,
0.0857142857142857,0.1,0.114285714285714,0.128571428571429,0.142857142857143,
0.157142857142857,0.171428571428571,0.185714285714286,0.2,0.214285714285714,
0.228571428571429,0.242857142857143,0.257142857142857,0.271428571428571,
0.285714285714286,0.3,0.314285714285714,0.328571428571429,0.342857142857143,
0.357142857142857,0.371428571428571,0.385714285714286,0.4,0.414285714285714,
0.428571428571429,0.442857142857143,0.457142857142857,0.471428571428572,
0.485714285714286,0.5,0.514285714285714,0.528571428571429,0.542857142857143,
0.557142857142857,0.571428571428571,0.585714285714286,0.6,0.614285714285714,
0.628571428571428,0.642857142857142,0.657142857142857,0.671428571428571,
0.685714285714285,0.699999999999999,0.714285714285714,0.728571428571428,
0.742857142857142,0.757142857142856,0.771428571428571,0.785714285714285,
0.799999999999999,0.814285714285713,0.828571428571428,0.842857142857142,
0.857142857142856,0.87142857142857,0.885714285714284,0.899999999999999,
0.914285714285713,0.928571428571427,0.942857142857141,0.957142857142856,
0.97142857142857,0.985714285714284,1.),(0.,1.8),.UNSPECIFIED.);
#997=B_SPLINE_SURFACE_WITH_KNOTS('',5,1,((#34932,#34933),(#34934,#34935),
(#34936,#34937),(#34938,#34939),(#34940,#34941),(#34942,#34943),(#34944,
#34945),(#34946,#34947),(#34948,#34949),(#34950,#34951),(#34952,#34953),
(#34954,#34955),(#34956,#34957),(#34958,#34959),(#34960,#34961),(#34962,
#34963),(#34964,#34965),(#34966,#34967),(#34968,#34969),(#34970,#34971),
(#34972,#34973),(#34974,#34975),(#34976,#34977),(#34978,#34979),(#34980,
#34981),(#34982,#34983),(#34984,#34985),(#34986,#34987),(#34988,#34989),
(#34990,#34991),(#34992,#34993),(#34994,#34995),(#34996,#34997),(#34998,
#34999),(#35000,#35001),(#35002,#35003),(#35004,#35005),(#35006,#35007),
(#35008,#35009),(#35010,#35011),(#35012,#35013),(#35014,#35015),(#35016,
#35017),(#35018,#35019),(#35020,#35021),(#35022,#35023),(#35024,#35025),
(#35026,#35027),(#35028,#35029),(#35030,#35031),(#35032,#35033),(#35034,
#35035),(#35036,#35037),(#35038,#35039),(#35040,#35041),(#35042,#35043),
(#35044,#35045),(#35046,#35047),(#35048,#35049),(#35050,#35051),(#35052,
#35053),(#35054,#35055),(#35056,#35057),(#35058,#35059),(#35060,#35061),
(#35062,#35063),(#35064,#35065),(#35066,#35067),(#35068,#35069),(#35070,
#35071),(#35072,#35073),(#35074,#35075),(#35076,#35077),(#35078,#35079),
(#35080,#35081)),.UNSPECIFIED.,.F.,.F.,.F.,(6,1,1,1,1,1,1,1,1,1,1,1,1,1,
1,1,1,1,1,1,1,1,1,1,1,1,1,1,1,1,1,1,1,1,1,1,1,1,1,1,1,1,1,1,1,1,1,1,1,1,
1,1,1,1,1,1,1,1,1,1,1,1,1,1,1,1,1,1,1,1,6),(2,2),(-1.,-0.985714285714284,
-0.97142857142857,-0.957142857142856,-0.942857142857141,-0.928571428571427,
-0.914285714285713,-0.899999999999999,-0.885714285714284,-0.87142857142857,
-0.857142857142856,-0.842857142857142,-0.828571428571428,-0.814285714285713,
-0.799999999999999,-0.785714285714285,-0.771428571428571,-0.757142857142856,
-0.742857142857142,-0.728571428571428,-0.714285714285714,-0.699999999999999,
-0.685714285714285,-0.671428571428571,-0.657142857142857,-0.642857142857142,
-0.628571428571428,-0.614285714285714,-0.6,-0.585714285714286,-0.571428571428571,
-0.557142857142857,-0.542857142857143,-0.528571428571429,-0.514285714285714,
-0.5,-0.485714285714286,-0.471428571428572,-0.457142857142857,-0.442857142857143,
-0.428571428571429,-0.414285714285714,-0.4,-0.385714285714286,-0.371428571428571,
-0.357142857142857,-0.342857142857143,-0.328571428571429,-0.314285714285714,
-0.3,-0.285714285714286,-0.271428571428571,-0.257142857142857,-0.242857142857143,
-0.228571428571429,-0.214285714285714,-0.2,-0.185714285714286,-0.171428571428571,
-0.157142857142857,-0.142857142857143,-0.128571428571429,-0.114285714285714,
-0.1,-0.0857142857142857,-0.0714285714285714,-0.0571428571428571,-0.0428571428571429,
-0.0285714285714286,-0.0142857142857143,0.),(0.,1.8),.UNSPECIFIED.);
#998=B_SPLINE_SURFACE_WITH_KNOTS('',5,1,((#35240,#35241),(#35242,#35243),
(#35244,#35245),(#35246,#35247),(#35248,#35249),(#35250,#35251),(#35252,
#35253),(#35254,#35255),(#35256,#35257),(#35258,#35259),(#35260,#35261),
(#35262,#35263),(#35264,#35265),(#35266,#35267),(#35268,#35269),(#35270,
#35271),(#35272,#35273),(#35274,#35275),(#35276,#35277),(#35278,#35279),
(#35280,#35281),(#35282,#35283),(#35284,#35285),(#35286,#35287),(#35288,
#35289),(#35290,#35291),(#35292,#35293),(#35294,#35295),(#35296,#35297),
(#35298,#35299),(#35300,#35301),(#35302,#35303),(#35304,#35305),(#35306,
#35307),(#35308,#35309),(#35310,#35311),(#35312,#35313),(#35314,#35315),
(#35316,#35317),(#35318,#35319),(#35320,#35321),(#35322,#35323),(#35324,
#35325),(#35326,#35327),(#35328,#35329),(#35330,#35331),(#35332,#35333),
(#35334,#35335),(#35336,#35337),(#35338,#35339),(#35340,#35341),(#35342,
#35343),(#35344,#35345),(#35346,#35347),(#35348,#35349),(#35350,#35351),
(#35352,#35353),(#35354,#35355),(#35356,#35357),(#35358,#35359),(#35360,
#35361),(#35362,#35363),(#35364,#35365),(#35366,#35367),(#35368,#35369),
(#35370,#35371),(#35372,#35373),(#35374,#35375),(#35376,#35377),(#35378,
#35379),(#35380,#35381),(#35382,#35383),(#35384,#35385),(#35386,#35387),
(#35388,#35389)),.UNSPECIFIED.,.F.,.F.,.F.,(6,1,1,1,1,1,1,1,1,1,1,1,1,1,
1,1,1,1,1,1,1,1,1,1,1,1,1,1,1,1,1,1,1,1,1,1,1,1,1,1,1,1,1,1,1,1,1,1,1,1,
1,1,1,1,1,1,1,1,1,1,1,1,1,1,1,1,1,1,1,1,6),(2,2),(0.,0.0142857142857143,
0.0285714285714286,0.0428571428571429,0.0571428571428571,0.0714285714285714,
0.0857142857142857,0.1,0.114285714285714,0.128571428571429,0.142857142857143,
0.157142857142857,0.171428571428571,0.185714285714286,0.2,0.214285714285714,
0.228571428571429,0.242857142857143,0.257142857142857,0.271428571428571,
0.285714285714286,0.3,0.314285714285714,0.328571428571429,0.342857142857143,
0.357142857142857,0.371428571428571,0.385714285714286,0.4,0.414285714285714,
0.428571428571429,0.442857142857143,0.457142857142857,0.471428571428572,
0.485714285714286,0.5,0.514285714285714,0.528571428571429,0.542857142857143,
0.557142857142857,0.571428571428571,0.585714285714286,0.6,0.614285714285714,
0.628571428571428,0.642857142857142,0.657142857142857,0.671428571428571,
0.685714285714285,0.699999999999999,0.714285714285714,0.728571428571428,
0.742857142857142,0.757142857142856,0.771428571428571,0.785714285714285,
0.799999999999999,0.814285714285713,0.828571428571428,0.842857142857142,
0.857142857142856,0.87142857142857,0.885714285714284,0.899999999999999,
0.914285714285713,0.928571428571427,0.942857142857141,0.957142857142856,
0.97142857142857,0.985714285714284,1.),(0.,1.8),.UNSPECIFIED.);
#999=B_SPLINE_SURFACE_WITH_KNOTS('',5,1,((#35538,#35539),(#35540,#35541),
(#35542,#35543),(#35544,#35545),(#35546,#35547),(#35548,#35549),(#35550,
#35551),(#35552,#35553),(#35554,#35555),(#35556,#35557),(#35558,#35559),
(#35560,#35561),(#35562,#35563),(#35564,#35565),(#35566,#35567),(#35568,
#35569),(#35570,#35571),(#35572,#35573),(#35574,#35575),(#35576,#35577),
(#35578,#35579),(#35580,#35581),(#35582,#35583),(#35584,#35585),(#35586,
#35587),(#35588,#35589),(#35590,#35591),(#35592,#35593),(#35594,#35595),
(#35596,#35597),(#35598,#35599),(#35600,#35601),(#35602,#35603),(#35604,
#35605),(#35606,#35607),(#35608,#35609),(#35610,#35611),(#35612,#35613),
(#35614,#35615),(#35616,#35617),(#35618,#35619),(#35620,#35621),(#35622,
#35623),(#35624,#35625),(#35626,#35627),(#35628,#35629),(#35630,#35631),
(#35632,#35633),(#35634,#35635),(#35636,#35637),(#35638,#35639),(#35640,
#35641),(#35642,#35643),(#35644,#35645),(#35646,#35647),(#35648,#35649),
(#35650,#35651),(#35652,#35653),(#35654,#35655),(#35656,#35657),(#35658,
#35659),(#35660,#35661),(#35662,#35663),(#35664,#35665),(#35666,#35667),
(#35668,#35669),(#35670,#35671),(#35672,#35673),(#35674,#35675),(#35676,
#35677),(#35678,#35679),(#35680,#35681),(#35682,#35683),(#35684,#35685),
(#35686,#35687)),.UNSPECIFIED.,.F.,.F.,.F.,(6,1,1,1,1,1,1,1,1,1,1,1,1,1,
1,1,1,1,1,1,1,1,1,1,1,1,1,1,1,1,1,1,1,1,1,1,1,1,1,1,1,1,1,1,1,1,1,1,1,1,
1,1,1,1,1,1,1,1,1,1,1,1,1,1,1,1,1,1,1,1,6),(2,2),(-1.,-0.985714285714284,
-0.97142857142857,-0.957142857142856,-0.942857142857141,-0.928571428571427,
-0.914285714285713,-0.899999999999999,-0.885714285714284,-0.87142857142857,
-0.857142857142856,-0.842857142857142,-0.828571428571428,-0.814285714285713,
-0.799999999999999,-0.785714285714285,-0.771428571428571,-0.757142857142856,
-0.742857142857142,-0.728571428571428,-0.714285714285714,-0.699999999999999,
-0.685714285714285,-0.671428571428571,-0.657142857142857,-0.642857142857142,
-0.628571428571428,-0.614285714285714,-0.6,-0.585714285714286,-0.571428571428571,
-0.557142857142857,-0.542857142857143,-0.528571428571429,-0.514285714285714,
-0.5,-0.485714285714286,-0.471428571428572,-0.457142857142857,-0.442857142857143,
-0.428571428571429,-0.414285714285714,-0.4,-0.385714285714286,-0.371428571428571,
-0.357142857142857,-0.342857142857143,-0.328571428571429,-0.314285714285714,
-0.3,-0.285714285714286,-0.271428571428571,-0.257142857142857,-0.242857142857143,
-0.228571428571429,-0.214285714285714,-0.2,-0.185714285714286,-0.171428571428571,
-0.157142857142857,-0.142857142857143,-0.128571428571429,-0.114285714285714,
-0.1,-0.0857142857142857,-0.0714285714285714,-0.0571428571428571,-0.0428571428571429,
-0.0285714285714286,-0.0142857142857143,0.),(0.,1.8),.UNSPECIFIED.);
#1000=B_SPLINE_SURFACE_WITH_KNOTS('',5,1,((#35846,#35847),(#35848,#35849),
(#35850,#35851),(#35852,#35853),(#35854,#35855),(#35856,#35857),(#35858,
#35859),(#35860,#35861),(#35862,#35863),(#35864,#35865),(#35866,#35867),
(#35868,#35869),(#35870,#35871),(#35872,#35873),(#35874,#35875),(#35876,
#35877),(#35878,#35879),(#35880,#35881),(#35882,#35883),(#35884,#35885),
(#35886,#35887),(#35888,#35889),(#35890,#35891),(#35892,#35893),(#35894,
#35895),(#35896,#35897),(#35898,#35899),(#35900,#35901),(#35902,#35903),
(#35904,#35905),(#35906,#35907),(#35908,#35909),(#35910,#35911),(#35912,
#35913),(#35914,#35915),(#35916,#35917),(#35918,#35919),(#35920,#35921),
(#35922,#35923),(#35924,#35925),(#35926,#35927),(#35928,#35929),(#35930,
#35931),(#35932,#35933),(#35934,#35935),(#35936,#35937),(#35938,#35939),
(#35940,#35941),(#35942,#35943),(#35944,#35945),(#35946,#35947),(#35948,
#35949),(#35950,#35951),(#35952,#35953),(#35954,#35955),(#35956,#35957),
(#35958,#35959),(#35960,#35961),(#35962,#35963),(#35964,#35965),(#35966,
#35967),(#35968,#35969),(#35970,#35971),(#35972,#35973),(#35974,#35975),
(#35976,#35977),(#35978,#35979),(#35980,#35981),(#35982,#35983),(#35984,
#35985),(#35986,#35987),(#35988,#35989),(#35990,#35991),(#35992,#35993),
(#35994,#35995)),.UNSPECIFIED.,.F.,.F.,.F.,(6,1,1,1,1,1,1,1,1,1,1,1,1,1,
1,1,1,1,1,1,1,1,1,1,1,1,1,1,1,1,1,1,1,1,1,1,1,1,1,1,1,1,1,1,1,1,1,1,1,1,
1,1,1,1,1,1,1,1,1,1,1,1,1,1,1,1,1,1,1,1,6),(2,2),(0.,0.0142857142857143,
0.0285714285714286,0.0428571428571429,0.0571428571428571,0.0714285714285714,
0.0857142857142857,0.1,0.114285714285714,0.128571428571429,0.142857142857143,
0.157142857142857,0.171428571428571,0.185714285714286,0.2,0.214285714285714,
0.228571428571429,0.242857142857143,0.257142857142857,0.271428571428571,
0.285714285714286,0.3,0.314285714285714,0.328571428571429,0.342857142857143,
0.357142857142857,0.371428571428571,0.385714285714286,0.4,0.414285714285714,
0.428571428571429,0.442857142857143,0.457142857142857,0.471428571428572,
0.485714285714286,0.5,0.514285714285714,0.528571428571429,0.542857142857143,
0.557142857142857,0.571428571428571,0.585714285714286,0.6,0.614285714285714,
0.628571428571428,0.642857142857142,0.657142857142857,0.671428571428571,
0.685714285714285,0.699999999999999,0.714285714285714,0.728571428571428,
0.742857142857142,0.757142857142856,0.771428571428571,0.785714285714285,
0.799999999999999,0.814285714285713,0.828571428571428,0.842857142857142,
0.857142857142856,0.87142857142857,0.885714285714284,0.899999999999999,
0.914285714285713,0.928571428571427,0.942857142857141,0.957142857142856,
0.97142857142857,0.985714285714284,1.),(0.,1.8),.UNSPECIFIED.);
#1001=B_SPLINE_SURFACE_WITH_KNOTS('',5,1,((#36144,#36145),(#36146,#36147),
(#36148,#36149),(#36150,#36151),(#36152,#36153),(#36154,#36155),(#36156,
#36157),(#36158,#36159),(#36160,#36161),(#36162,#36163),(#36164,#36165),
(#36166,#36167),(#36168,#36169),(#36170,#36171),(#36172,#36173),(#36174,
#36175),(#36176,#36177),(#36178,#36179),(#36180,#36181),(#36182,#36183),
(#36184,#36185),(#36186,#36187),(#36188,#36189),(#36190,#36191),(#36192,
#36193),(#36194,#36195),(#36196,#36197),(#36198,#36199),(#36200,#36201),
(#36202,#36203),(#36204,#36205),(#36206,#36207),(#36208,#36209),(#36210,
#36211),(#36212,#36213),(#36214,#36215),(#36216,#36217),(#36218,#36219),
(#36220,#36221),(#36222,#36223),(#36224,#36225),(#36226,#36227),(#36228,
#36229),(#36230,#36231),(#36232,#36233),(#36234,#36235),(#36236,#36237),
(#36238,#36239),(#36240,#36241),(#36242,#36243),(#36244,#36245),(#36246,
#36247),(#36248,#36249),(#36250,#36251),(#36252,#36253),(#36254,#36255),
(#36256,#36257),(#36258,#36259),(#36260,#36261),(#36262,#36263),(#36264,
#36265),(#36266,#36267),(#36268,#36269),(#36270,#36271),(#36272,#36273),
(#36274,#36275),(#36276,#36277),(#36278,#36279),(#36280,#36281),(#36282,
#36283),(#36284,#36285),(#36286,#36287),(#36288,#36289),(#36290,#36291),
(#36292,#36293)),.UNSPECIFIED.,.F.,.F.,.F.,(6,1,1,1,1,1,1,1,1,1,1,1,1,1,
1,1,1,1,1,1,1,1,1,1,1,1,1,1,1,1,1,1,1,1,1,1,1,1,1,1,1,1,1,1,1,1,1,1,1,1,
1,1,1,1,1,1,1,1,1,1,1,1,1,1,1,1,1,1,1,1,6),(2,2),(-1.,-0.985714285714284,
-0.97142857142857,-0.957142857142856,-0.942857142857141,-0.928571428571427,
-0.914285714285713,-0.899999999999999,-0.885714285714284,-0.87142857142857,
-0.857142857142856,-0.842857142857142,-0.828571428571428,-0.814285714285713,
-0.799999999999999,-0.785714285714285,-0.771428571428571,-0.757142857142856,
-0.742857142857142,-0.728571428571428,-0.714285714285714,-0.699999999999999,
-0.685714285714285,-0.671428571428571,-0.657142857142857,-0.642857142857142,
-0.628571428571428,-0.614285714285714,-0.6,-0.585714285714286,-0.571428571428571,
-0.557142857142857,-0.542857142857143,-0.528571428571429,-0.514285714285714,
-0.5,-0.485714285714286,-0.471428571428572,-0.457142857142857,-0.442857142857143,
-0.428571428571429,-0.414285714285714,-0.4,-0.385714285714286,-0.371428571428571,
-0.357142857142857,-0.342857142857143,-0.328571428571429,-0.314285714285714,
-0.3,-0.285714285714286,-0.271428571428571,-0.257142857142857,-0.242857142857143,
-0.228571428571429,-0.214285714285714,-0.2,-0.185714285714286,-0.171428571428571,
-0.157142857142857,-0.142857142857143,-0.128571428571429,-0.114285714285714,
-0.1,-0.0857142857142857,-0.0714285714285714,-0.0571428571428571,-0.0428571428571429,
-0.0285714285714286,-0.0142857142857143,0.),(0.,1.8),.UNSPECIFIED.);
#1002=B_SPLINE_SURFACE_WITH_KNOTS('',5,1,((#36452,#36453),(#36454,#36455),
(#36456,#36457),(#36458,#36459),(#36460,#36461),(#36462,#36463),(#36464,
#36465),(#36466,#36467),(#36468,#36469),(#36470,#36471),(#36472,#36473),
(#36474,#36475),(#36476,#36477),(#36478,#36479),(#36480,#36481),(#36482,
#36483),(#36484,#36485),(#36486,#36487),(#36488,#36489),(#36490,#36491),
(#36492,#36493),(#36494,#36495),(#36496,#36497),(#36498,#36499),(#36500,
#36501),(#36502,#36503),(#36504,#36505),(#36506,#36507),(#36508,#36509),
(#36510,#36511),(#36512,#36513),(#36514,#36515),(#36516,#36517),(#36518,
#36519),(#36520,#36521),(#36522,#36523),(#36524,#36525),(#36526,#36527),
(#36528,#36529),(#36530,#36531),(#36532,#36533),(#36534,#36535),(#36536,
#36537),(#36538,#36539),(#36540,#36541),(#36542,#36543),(#36544,#36545),
(#36546,#36547),(#36548,#36549),(#36550,#36551),(#36552,#36553),(#36554,
#36555),(#36556,#36557),(#36558,#36559),(#36560,#36561),(#36562,#36563),
(#36564,#36565),(#36566,#36567),(#36568,#36569),(#36570,#36571),(#36572,
#36573),(#36574,#36575),(#36576,#36577),(#36578,#36579),(#36580,#36581),
(#36582,#36583),(#36584,#36585),(#36586,#36587),(#36588,#36589),(#36590,
#36591),(#36592,#36593),(#36594,#36595),(#36596,#36597),(#36598,#36599),
(#36600,#36601)),.UNSPECIFIED.,.F.,.F.,.F.,(6,1,1,1,1,1,1,1,1,1,1,1,1,1,
1,1,1,1,1,1,1,1,1,1,1,1,1,1,1,1,1,1,1,1,1,1,1,1,1,1,1,1,1,1,1,1,1,1,1,1,
1,1,1,1,1,1,1,1,1,1,1,1,1,1,1,1,1,1,1,1,6),(2,2),(0.,0.0142857142857143,
0.0285714285714286,0.0428571428571429,0.0571428571428571,0.0714285714285714,
0.0857142857142857,0.1,0.114285714285714,0.128571428571429,0.142857142857143,
0.157142857142857,0.171428571428571,0.185714285714286,0.2,0.214285714285714,
0.228571428571429,0.242857142857143,0.257142857142857,0.271428571428571,
0.285714285714286,0.3,0.314285714285714,0.328571428571429,0.342857142857143,
0.357142857142857,0.371428571428571,0.385714285714286,0.4,0.414285714285714,
0.428571428571429,0.442857142857143,0.457142857142857,0.471428571428572,
0.485714285714286,0.5,0.514285714285714,0.528571428571429,0.542857142857143,
0.557142857142857,0.571428571428571,0.585714285714286,0.6,0.614285714285714,
0.628571428571428,0.642857142857142,0.657142857142857,0.671428571428571,
0.685714285714285,0.699999999999999,0.714285714285714,0.728571428571428,
0.742857142857142,0.757142857142856,0.771428571428571,0.785714285714285,
0.799999999999999,0.814285714285713,0.828571428571428,0.842857142857142,
0.857142857142856,0.87142857142857,0.885714285714284,0.899999999999999,
0.914285714285713,0.928571428571427,0.942857142857141,0.957142857142856,
0.97142857142857,0.985714285714284,1.),(0.,1.8),.UNSPECIFIED.);
#1003=B_SPLINE_SURFACE_WITH_KNOTS('',5,1,((#36750,#36751),(#36752,#36753),
(#36754,#36755),(#36756,#36757),(#36758,#36759),(#36760,#36761),(#36762,
#36763),(#36764,#36765),(#36766,#36767),(#36768,#36769),(#36770,#36771),
(#36772,#36773),(#36774,#36775),(#36776,#36777),(#36778,#36779),(#36780,
#36781),(#36782,#36783),(#36784,#36785),(#36786,#36787),(#36788,#36789),
(#36790,#36791),(#36792,#36793),(#36794,#36795),(#36796,#36797),(#36798,
#36799),(#36800,#36801),(#36802,#36803),(#36804,#36805),(#36806,#36807),
(#36808,#36809),(#36810,#36811),(#36812,#36813),(#36814,#36815),(#36816,
#36817),(#36818,#36819),(#36820,#36821),(#36822,#36823),(#36824,#36825),
(#36826,#36827),(#36828,#36829),(#36830,#36831),(#36832,#36833),(#36834,
#36835),(#36836,#36837),(#36838,#36839),(#36840,#36841),(#36842,#36843),
(#36844,#36845),(#36846,#36847),(#36848,#36849),(#36850,#36851),(#36852,
#36853),(#36854,#36855),(#36856,#36857),(#36858,#36859),(#36860,#36861),
(#36862,#36863),(#36864,#36865),(#36866,#36867),(#36868,#36869),(#36870,
#36871),(#36872,#36873),(#36874,#36875),(#36876,#36877),(#36878,#36879),
(#36880,#36881),(#36882,#36883),(#36884,#36885),(#36886,#36887),(#36888,
#36889),(#36890,#36891),(#36892,#36893),(#36894,#36895),(#36896,#36897),
(#36898,#36899)),.UNSPECIFIED.,.F.,.F.,.F.,(6,1,1,1,1,1,1,1,1,1,1,1,1,1,
1,1,1,1,1,1,1,1,1,1,1,1,1,1,1,1,1,1,1,1,1,1,1,1,1,1,1,1,1,1,1,1,1,1,1,1,
1,1,1,1,1,1,1,1,1,1,1,1,1,1,1,1,1,1,1,1,6),(2,2),(-1.,-0.985714285714284,
-0.97142857142857,-0.957142857142856,-0.942857142857141,-0.928571428571427,
-0.914285714285713,-0.899999999999999,-0.885714285714284,-0.87142857142857,
-0.857142857142856,-0.842857142857142,-0.828571428571428,-0.814285714285713,
-0.799999999999999,-0.785714285714285,-0.771428571428571,-0.757142857142856,
-0.742857142857142,-0.728571428571428,-0.714285714285714,-0.699999999999999,
-0.685714285714285,-0.671428571428571,-0.657142857142857,-0.642857142857142,
-0.628571428571428,-0.614285714285714,-0.6,-0.585714285714286,-0.571428571428571,
-0.557142857142857,-0.542857142857143,-0.528571428571429,-0.514285714285714,
-0.5,-0.485714285714286,-0.471428571428572,-0.457142857142857,-0.442857142857143,
-0.428571428571429,-0.414285714285714,-0.4,-0.385714285714286,-0.371428571428571,
-0.357142857142857,-0.342857142857143,-0.328571428571429,-0.314285714285714,
-0.3,-0.285714285714286,-0.271428571428571,-0.257142857142857,-0.242857142857143,
-0.228571428571429,-0.214285714285714,-0.2,-0.185714285714286,-0.171428571428571,
-0.157142857142857,-0.142857142857143,-0.128571428571429,-0.114285714285714,
-0.1,-0.0857142857142857,-0.0714285714285714,-0.0571428571428571,-0.0428571428571429,
-0.0285714285714286,-0.0142857142857143,0.),(0.,1.8),.UNSPECIFIED.);
#1004=B_SPLINE_SURFACE_WITH_KNOTS('',5,1,((#37058,#37059),(#37060,#37061),
(#37062,#37063),(#37064,#37065),(#37066,#37067),(#37068,#37069),(#37070,
#37071),(#37072,#37073),(#37074,#37075),(#37076,#37077),(#37078,#37079),
(#37080,#37081),(#37082,#37083),(#37084,#37085),(#37086,#37087),(#37088,
#37089),(#37090,#37091),(#37092,#37093),(#37094,#37095),(#37096,#37097),
(#37098,#37099),(#37100,#37101),(#37102,#37103),(#37104,#37105),(#37106,
#37107),(#37108,#37109),(#37110,#37111),(#37112,#37113),(#37114,#37115),
(#37116,#37117),(#37118,#37119),(#37120,#37121),(#37122,#37123),(#37124,
#37125),(#37126,#37127),(#37128,#37129),(#37130,#37131),(#37132,#37133),
(#37134,#37135),(#37136,#37137),(#37138,#37139),(#37140,#37141),(#37142,
#37143),(#37144,#37145),(#37146,#37147),(#37148,#37149),(#37150,#37151),
(#37152,#37153),(#37154,#37155),(#37156,#37157),(#37158,#37159),(#37160,
#37161),(#37162,#37163),(#37164,#37165),(#37166,#37167),(#37168,#37169),
(#37170,#37171),(#37172,#37173),(#37174,#37175),(#37176,#37177),(#37178,
#37179),(#37180,#37181),(#37182,#37183),(#37184,#37185),(#37186,#37187),
(#37188,#37189),(#37190,#37191),(#37192,#37193),(#37194,#37195),(#37196,
#37197),(#37198,#37199),(#37200,#37201),(#37202,#37203),(#37204,#37205),
(#37206,#37207)),.UNSPECIFIED.,.F.,.F.,.F.,(6,1,1,1,1,1,1,1,1,1,1,1,1,1,
1,1,1,1,1,1,1,1,1,1,1,1,1,1,1,1,1,1,1,1,1,1,1,1,1,1,1,1,1,1,1,1,1,1,1,1,
1,1,1,1,1,1,1,1,1,1,1,1,1,1,1,1,1,1,1,1,6),(2,2),(0.,0.0142857142857143,
0.0285714285714286,0.0428571428571429,0.0571428571428571,0.0714285714285714,
0.0857142857142857,0.1,0.114285714285714,0.128571428571429,0.142857142857143,
0.157142857142857,0.171428571428571,0.185714285714286,0.2,0.214285714285714,
0.228571428571429,0.242857142857143,0.257142857142857,0.271428571428571,
0.285714285714286,0.3,0.314285714285714,0.328571428571429,0.342857142857143,
0.357142857142857,0.371428571428571,0.385714285714286,0.4,0.414285714285714,
0.428571428571429,0.442857142857143,0.457142857142857,0.471428571428572,
0.485714285714286,0.5,0.514285714285714,0.528571428571429,0.542857142857143,
0.557142857142857,0.571428571428571,0.585714285714286,0.6,0.614285714285714,
0.628571428571428,0.642857142857142,0.657142857142857,0.671428571428571,
0.685714285714285,0.699999999999999,0.714285714285714,0.728571428571428,
0.742857142857142,0.757142857142856,0.771428571428571,0.785714285714285,
0.799999999999999,0.814285714285713,0.828571428571428,0.842857142857142,
0.857142857142856,0.87142857142857,0.885714285714284,0.899999999999999,
0.914285714285713,0.928571428571427,0.942857142857141,0.957142857142856,
0.97142857142857,0.985714285714284,1.),(0.,1.8),.UNSPECIFIED.);
#1005=B_SPLINE_SURFACE_WITH_KNOTS('',5,1,((#37720,#37721),(#37722,#37723),
(#37724,#37725),(#37726,#37727),(#37728,#37729),(#37730,#37731),(#37732,
#37733),(#37734,#37735),(#37736,#37737),(#37738,#37739),(#37740,#37741),
(#37742,#37743),(#37744,#37745),(#37746,#37747),(#37748,#37749),(#37750,
#37751),(#37752,#37753),(#37754,#37755),(#37756,#37757),(#37758,#37759),
(#37760,#37761),(#37762,#37763),(#37764,#37765),(#37766,#37767),(#37768,
#37769),(#37770,#37771),(#37772,#37773),(#37774,#37775),(#37776,#37777),
(#37778,#37779),(#37780,#37781),(#37782,#37783),(#37784,#37785),(#37786,
#37787),(#37788,#37789),(#37790,#37791),(#37792,#37793),(#37794,#37795),
(#37796,#37797),(#37798,#37799),(#37800,#37801),(#37802,#37803),(#37804,
#37805),(#37806,#37807),(#37808,#37809),(#37810,#37811),(#37812,#37813),
(#37814,#37815),(#37816,#37817),(#37818,#37819),(#37820,#37821),(#37822,
#37823),(#37824,#37825),(#37826,#37827),(#37828,#37829),(#37830,#37831),
(#37832,#37833),(#37834,#37835),(#37836,#37837),(#37838,#37839),(#37840,
#37841),(#37842,#37843),(#37844,#37845),(#37846,#37847),(#37848,#37849),
(#37850,#37851),(#37852,#37853),(#37854,#37855),(#37856,#37857),(#37858,
#37859),(#37860,#37861),(#37862,#37863),(#37864,#37865),(#37866,#37867),
(#37868,#37869)),.UNSPECIFIED.,.F.,.F.,.F.,(6,1,1,1,1,1,1,1,1,1,1,1,1,1,
1,1,1,1,1,1,1,1,1,1,1,1,1,1,1,1,1,1,1,1,1,1,1,1,1,1,1,1,1,1,1,1,1,1,1,1,
1,1,1,1,1,1,1,1,1,1,1,1,1,1,1,1,1,1,1,1,6),(2,2),(-1.,-0.985714285714284,
-0.97142857142857,-0.957142857142856,-0.942857142857141,-0.928571428571427,
-0.914285714285713,-0.899999999999999,-0.885714285714284,-0.87142857142857,
-0.857142857142856,-0.842857142857142,-0.828571428571428,-0.814285714285713,
-0.799999999999999,-0.785714285714285,-0.771428571428571,-0.757142857142856,
-0.742857142857142,-0.728571428571428,-0.714285714285714,-0.699999999999999,
-0.685714285714285,-0.671428571428571,-0.657142857142857,-0.642857142857142,
-0.628571428571428,-0.614285714285714,-0.6,-0.585714285714286,-0.571428571428571,
-0.557142857142857,-0.542857142857143,-0.528571428571429,-0.514285714285714,
-0.5,-0.485714285714286,-0.471428571428572,-0.457142857142857,-0.442857142857143,
-0.428571428571429,-0.414285714285714,-0.4,-0.385714285714286,-0.371428571428571,
-0.357142857142857,-0.342857142857143,-0.328571428571429,-0.314285714285714,
-0.3,-0.285714285714286,-0.271428571428571,-0.257142857142857,-0.242857142857143,
-0.228571428571429,-0.214285714285714,-0.2,-0.185714285714286,-0.171428571428571,
-0.157142857142857,-0.142857142857143,-0.128571428571429,-0.114285714285714,
-0.1,-0.0857142857142857,-0.0714285714285714,-0.0571428571428571,-0.0428571428571429,
-0.0285714285714286,-0.0142857142857143,0.),(0.,1.8),.UNSPECIFIED.);
#1006=B_SPLINE_SURFACE_WITH_KNOTS('',5,1,((#37873,#37874),(#37875,#37876),
(#37877,#37878),(#37879,#37880),(#37881,#37882),(#37883,#37884),(#37885,
#37886),(#37887,#37888),(#37889,#37890),(#37891,#37892),(#37893,#37894),
(#37895,#37896),(#37897,#37898),(#37899,#37900),(#37901,#37902),(#37903,
#37904),(#37905,#37906),(#37907,#37908),(#37909,#37910),(#37911,#37912),
(#37913,#37914),(#37915,#37916),(#37917,#37918),(#37919,#37920),(#37921,
#37922),(#37923,#37924),(#37925,#37926),(#37927,#37928),(#37929,#37930),
(#37931,#37932),(#37933,#37934),(#37935,#37936),(#37937,#37938),(#37939,
#37940),(#37941,#37942),(#37943,#37944),(#37945,#37946),(#37947,#37948),
(#37949,#37950),(#37951,#37952),(#37953,#37954),(#37955,#37956),(#37957,
#37958),(#37959,#37960),(#37961,#37962),(#37963,#37964),(#37965,#37966),
(#37967,#37968),(#37969,#37970),(#37971,#37972),(#37973,#37974),(#37975,
#37976),(#37977,#37978),(#37979,#37980),(#37981,#37982),(#37983,#37984),
(#37985,#37986),(#37987,#37988),(#37989,#37990),(#37991,#37992),(#37993,
#37994),(#37995,#37996),(#37997,#37998),(#37999,#38000),(#38001,#38002),
(#38003,#38004),(#38005,#38006),(#38007,#38008),(#38009,#38010),(#38011,
#38012),(#38013,#38014),(#38015,#38016),(#38017,#38018),(#38019,#38020),
(#38021,#38022)),.UNSPECIFIED.,.F.,.F.,.F.,(6,1,1,1,1,1,1,1,1,1,1,1,1,1,
1,1,1,1,1,1,1,1,1,1,1,1,1,1,1,1,1,1,1,1,1,1,1,1,1,1,1,1,1,1,1,1,1,1,1,1,
1,1,1,1,1,1,1,1,1,1,1,1,1,1,1,1,1,1,1,1,6),(2,2),(0.,0.0142857142857143,
0.0285714285714286,0.0428571428571429,0.0571428571428571,0.0714285714285714,
0.0857142857142857,0.1,0.114285714285714,0.128571428571429,0.142857142857143,
0.157142857142857,0.171428571428571,0.185714285714286,0.2,0.214285714285714,
0.228571428571429,0.242857142857143,0.257142857142857,0.271428571428571,
0.285714285714286,0.3,0.314285714285714,0.328571428571429,0.342857142857143,
0.357142857142857,0.371428571428571,0.385714285714286,0.4,0.414285714285714,
0.428571428571429,0.442857142857143,0.457142857142857,0.471428571428572,
0.485714285714286,0.5,0.514285714285714,0.528571428571429,0.542857142857143,
0.557142857142857,0.571428571428571,0.585714285714286,0.6,0.614285714285714,
0.628571428571428,0.642857142857142,0.657142857142857,0.671428571428571,
0.685714285714285,0.699999999999999,0.714285714285714,0.728571428571428,
0.742857142857142,0.757142857142856,0.771428571428571,0.785714285714285,
0.799999999999999,0.814285714285713,0.828571428571428,0.842857142857142,
0.857142857142856,0.87142857142857,0.885714285714284,0.899999999999999,
0.914285714285713,0.928571428571427,0.942857142857141,0.957142857142856,
0.97142857142857,0.985714285714284,1.),(0.,1.8),.UNSPECIFIED.);
#1007=PLANE('',#13192);
#1008=PLANE('',#13193);
#1009=PLANE('',#13197);
#1010=PLANE('',#13201);
#1011=PLANE('',#13205);
#1012=PLANE('',#13209);
#1013=PLANE('',#13213);
#1014=PLANE('',#13217);
#1015=PLANE('',#13221);
#1016=PLANE('',#13225);
#1017=PLANE('',#13229);
#1018=PLANE('',#13233);
#1019=PLANE('',#13237);
#1020=PLANE('',#13241);
#1021=PLANE('',#13245);
#1022=PLANE('',#13249);
#1023=PLANE('',#13253);
#1024=PLANE('',#13257);
#1025=PLANE('',#13261);
#1026=PLANE('',#13265);
#1027=PLANE('',#13269);
#1028=PLANE('',#13273);
#1029=PLANE('',#13277);
#1030=PLANE('',#13281);
#1031=PLANE('',#13285);
#1032=PLANE('',#13289);
#1033=PLANE('',#13293);
#1034=PLANE('',#13297);
#1035=PLANE('',#13301);
#1036=PLANE('',#13305);
#1037=PLANE('',#13309);
#1038=PLANE('',#13313);
#1039=PLANE('',#13317);
#1040=PLANE('',#13321);
#1041=PLANE('',#13325);
#1042=PLANE('',#13329);
#1043=PLANE('',#13333);
#1044=PLANE('',#13337);
#1045=PLANE('',#13341);
#1046=PLANE('',#13345);
#1047=PLANE('',#13403);
#1048=PLANE('',#13427);
#1049=PLANE('',#13471);
#1050=PLANE('',#13473);
#1051=PLANE('',#13483);
#1052=PLANE('',#13484);
#1053=PLANE('',#13488);
#1054=PLANE('',#13492);
#1055=PLANE('',#13496);
#1056=PLANE('',#13500);
#1057=PLANE('',#13504);
#1058=PLANE('',#13508);
#1059=PLANE('',#13512);
#1060=PLANE('',#13516);
#1061=PLANE('',#13520);
#1062=PLANE('',#13524);
#1063=PLANE('',#13528);
#1064=PLANE('',#13532);
#1065=PLANE('',#13536);
#1066=PLANE('',#13540);
#1067=PLANE('',#13544);
#1068=PLANE('',#13548);
#1069=PLANE('',#13552);
#1070=PLANE('',#13556);
#1071=PLANE('',#13584);
#1072=PLANE('',#13598);
#1073=PLANE('',#13622);
#1074=PLANE('',#13624);
#1075=PLANE('',#13652);
#1076=PLANE('',#13653);
#1077=PLANE('',#13710);
#1078=PLANE('',#13711);
#1079=PLANE('',#13712);
#1080=PLANE('',#13713);
#1081=PLANE('',#13714);
#1082=PLANE('',#13715);
#1083=PLANE('',#13820);
#1084=PLANE('',#13821);
#1085=PLANE('',#13822);
#1086=PLANE('',#13823);
#1087=PLANE('',#13824);
#1088=PLANE('',#13827);
#1089=PLANE('',#13832);
#1090=PLANE('',#13833);
#1091=PLANE('',#13834);
#1092=PLANE('',#13837);
#1093=PLANE('',#13848);
#1094=PLANE('',#13849);
#1095=PLANE('',#13850);
#1096=PLANE('',#13851);
#1097=PLANE('',#13852);
#1098=PLANE('',#13855);
#1099=PLANE('',#13866);
#1100=PLANE('',#13867);
#1101=PLANE('',#13868);
#1102=PLANE('',#13869);
#1103=PLANE('',#13870);
#1104=PLANE('',#13873);
#1105=PLANE('',#13884);
#1106=PLANE('',#13885);
#1107=PLANE('',#13886);
#1108=PLANE('',#13887);
#1109=PLANE('',#13888);
#1110=PLANE('',#13891);
#1111=PLANE('',#13902);
#1112=PLANE('',#13903);
#1113=PLANE('',#13904);
#1114=PLANE('',#13905);
#1115=PLANE('',#13906);
#1116=PLANE('',#13909);
#1117=PLANE('',#13920);
#1118=PLANE('',#13921);
#1119=PLANE('',#13922);
#1120=PLANE('',#13923);
#1121=PLANE('',#13924);
#1122=PLANE('',#13927);
#1123=PLANE('',#13932);
#1124=PLANE('',#13935);
#1125=PLANE('',#13965);
#1126=PLANE('',#13966);
#1127=PLANE('',#14023);
#1128=PLANE('',#14024);
#1129=PLANE('',#14025);
#1130=PLANE('',#14026);
#1131=PLANE('',#14027);
#1132=PLANE('',#14028);
#1133=PLANE('',#14133);
#1134=PLANE('',#14134);
#1135=PLANE('',#14135);
#1136=PLANE('',#14136);
#1137=PLANE('',#14137);
#1138=PLANE('',#14140);
#1139=PLANE('',#14145);
#1140=PLANE('',#14146);
#1141=PLANE('',#14147);
#1142=PLANE('',#14150);
#1143=PLANE('',#14161);
#1144=PLANE('',#14162);
#1145=PLANE('',#14163);
#1146=PLANE('',#14164);
#1147=PLANE('',#14165);
#1148=PLANE('',#14168);
#1149=PLANE('',#14179);
#1150=PLANE('',#14180);
#1151=PLANE('',#14181);
#1152=PLANE('',#14182);
#1153=PLANE('',#14183);
#1154=PLANE('',#14186);
#1155=PLANE('',#14197);
#1156=PLANE('',#14198);
#1157=PLANE('',#14199);
#1158=PLANE('',#14200);
#1159=PLANE('',#14201);
#1160=PLANE('',#14204);
#1161=PLANE('',#14215);
#1162=PLANE('',#14216);
#1163=PLANE('',#14217);
#1164=PLANE('',#14218);
#1165=PLANE('',#14219);
#1166=PLANE('',#14222);
#1167=PLANE('',#14233);
#1168=PLANE('',#14234);
#1169=PLANE('',#14235);
#1170=PLANE('',#14236);
#1171=PLANE('',#14237);
#1172=PLANE('',#14240);
#1173=PLANE('',#14245);
#1174=PLANE('',#14248);
#1175=PLANE('',#14278);
#1176=PLANE('',#14279);
#1177=PLANE('',#14336);
#1178=PLANE('',#14337);
#1179=PLANE('',#14338);
#1180=PLANE('',#14339);
#1181=PLANE('',#14340);
#1182=PLANE('',#14341);
#1183=PLANE('',#14446);
#1184=PLANE('',#14447);
#1185=PLANE('',#14448);
#1186=PLANE('',#14449);
#1187=PLANE('',#14450);
#1188=PLANE('',#14453);
#1189=PLANE('',#14458);
#1190=PLANE('',#14459);
#1191=PLANE('',#14460);
#1192=PLANE('',#14463);
#1193=PLANE('',#14474);
#1194=PLANE('',#14475);
#1195=PLANE('',#14476);
#1196=PLANE('',#14477);
#1197=PLANE('',#14478);
#1198=PLANE('',#14481);
#1199=PLANE('',#14492);
#1200=PLANE('',#14493);
#1201=PLANE('',#14494);
#1202=PLANE('',#14495);
#1203=PLANE('',#14496);
#1204=PLANE('',#14499);
#1205=PLANE('',#14510);
#1206=PLANE('',#14511);
#1207=PLANE('',#14512);
#1208=PLANE('',#14513);
#1209=PLANE('',#14514);
#1210=PLANE('',#14517);
#1211=PLANE('',#14528);
#1212=PLANE('',#14529);
#1213=PLANE('',#14530);
#1214=PLANE('',#14531);
#1215=PLANE('',#14532);
#1216=PLANE('',#14535);
#1217=PLANE('',#14546);
#1218=PLANE('',#14547);
#1219=PLANE('',#14548);
#1220=PLANE('',#14549);
#1221=PLANE('',#14550);
#1222=PLANE('',#14553);
#1223=PLANE('',#14558);
#1224=PLANE('',#14561);
#1225=PLANE('',#14591);
#1226=PLANE('',#14592);
#1227=PLANE('',#14649);
#1228=PLANE('',#14650);
#1229=PLANE('',#14651);
#1230=PLANE('',#14652);
#1231=PLANE('',#14653);
#1232=PLANE('',#14654);
#1233=PLANE('',#14759);
#1234=PLANE('',#14760);
#1235=PLANE('',#14761);
#1236=PLANE('',#14762);
#1237=PLANE('',#14763);
#1238=PLANE('',#14766);
#1239=PLANE('',#14771);
#1240=PLANE('',#14772);
#1241=PLANE('',#14773);
#1242=PLANE('',#14776);
#1243=PLANE('',#14787);
#1244=PLANE('',#14788);
#1245=PLANE('',#14789);
#1246=PLANE('',#14790);
#1247=PLANE('',#14791);
#1248=PLANE('',#14794);
#1249=PLANE('',#14805);
#1250=PLANE('',#14806);
#1251=PLANE('',#14807);
#1252=PLANE('',#14808);
#1253=PLANE('',#14809);
#1254=PLANE('',#14812);
#1255=PLANE('',#14823);
#1256=PLANE('',#14824);
#1257=PLANE('',#14825);
#1258=PLANE('',#14826);
#1259=PLANE('',#14827);
#1260=PLANE('',#14830);
#1261=PLANE('',#14841);
#1262=PLANE('',#14842);
#1263=PLANE('',#14843);
#1264=PLANE('',#14844);
#1265=PLANE('',#14845);
#1266=PLANE('',#14848);
#1267=PLANE('',#14859);
#1268=PLANE('',#14860);
#1269=PLANE('',#14861);
#1270=PLANE('',#14862);
#1271=PLANE('',#14863);
#1272=PLANE('',#14866);
#1273=PLANE('',#14871);
#1274=PLANE('',#14874);
#1275=PLANE('',#14883);
#1276=PLANE('',#14887);
#1277=PLANE('',#14888);
#1278=PLANE('',#14889);
#1279=PLANE('',#14890);
#1280=PLANE('',#14891);
#1281=PLANE('',#14899);
#1282=PLANE('',#14900);
#1283=PLANE('',#14901);
#1284=PLANE('',#14902);
#1285=PLANE('',#14903);
#1286=PLANE('',#14904);
#1287=FACE_OUTER_BOUND('',#2039,.T.);
#1288=FACE_OUTER_BOUND('',#2040,.T.);
#1289=FACE_OUTER_BOUND('',#2041,.T.);
#1290=FACE_OUTER_BOUND('',#2042,.T.);
#1291=FACE_OUTER_BOUND('',#2043,.T.);
#1292=FACE_OUTER_BOUND('',#2044,.T.);
#1293=FACE_OUTER_BOUND('',#2045,.T.);
#1294=FACE_OUTER_BOUND('',#2046,.T.);
#1295=FACE_OUTER_BOUND('',#2047,.T.);
#1296=FACE_OUTER_BOUND('',#2048,.T.);
#1297=FACE_OUTER_BOUND('',#2049,.T.);
#1298=FACE_OUTER_BOUND('',#2050,.T.);
#1299=FACE_OUTER_BOUND('',#2051,.T.);
#1300=FACE_OUTER_BOUND('',#2052,.T.);
#1301=FACE_OUTER_BOUND('',#2053,.T.);
#1302=FACE_OUTER_BOUND('',#2054,.T.);
#1303=FACE_OUTER_BOUND('',#2055,.T.);
#1304=FACE_OUTER_BOUND('',#2056,.T.);
#1305=FACE_OUTER_BOUND('',#2057,.T.);
#1306=FACE_OUTER_BOUND('',#2058,.T.);
#1307=FACE_OUTER_BOUND('',#2059,.T.);
#1308=FACE_OUTER_BOUND('',#2060,.T.);
#1309=FACE_OUTER_BOUND('',#2061,.T.);
#1310=FACE_OUTER_BOUND('',#2062,.T.);
#1311=FACE_OUTER_BOUND('',#2063,.T.);
#1312=FACE_OUTER_BOUND('',#2064,.T.);
#1313=FACE_OUTER_BOUND('',#2065,.T.);
#1314=FACE_OUTER_BOUND('',#2066,.T.);
#1315=FACE_OUTER_BOUND('',#2067,.T.);
#1316=FACE_OUTER_BOUND('',#2068,.T.);
#1317=FACE_OUTER_BOUND('',#2069,.T.);
#1318=FACE_OUTER_BOUND('',#2070,.T.);
#1319=FACE_OUTER_BOUND('',#2071,.T.);
#1320=FACE_OUTER_BOUND('',#2072,.T.);
#1321=FACE_OUTER_BOUND('',#2073,.T.);
#1322=FACE_OUTER_BOUND('',#2074,.T.);
#1323=FACE_OUTER_BOUND('',#2075,.T.);
#1324=FACE_OUTER_BOUND('',#2076,.T.);
#1325=FACE_OUTER_BOUND('',#2077,.T.);
#1326=FACE_OUTER_BOUND('',#2078,.T.);
#1327=FACE_OUTER_BOUND('',#2079,.T.);
#1328=FACE_OUTER_BOUND('',#2080,.T.);
#1329=FACE_OUTER_BOUND('',#2081,.T.);
#1330=FACE_OUTER_BOUND('',#2082,.T.);
#1331=FACE_OUTER_BOUND('',#2083,.T.);
#1332=FACE_OUTER_BOUND('',#2084,.T.);
#1333=FACE_OUTER_BOUND('',#2085,.T.);
#1334=FACE_OUTER_BOUND('',#2086,.T.);
#1335=FACE_OUTER_BOUND('',#2087,.T.);
#1336=FACE_OUTER_BOUND('',#2088,.T.);
#1337=FACE_OUTER_BOUND('',#2089,.T.);
#1338=FACE_OUTER_BOUND('',#2090,.T.);
#1339=FACE_OUTER_BOUND('',#2091,.T.);
#1340=FACE_OUTER_BOUND('',#2092,.T.);
#1341=FACE_OUTER_BOUND('',#2093,.T.);
#1342=FACE_OUTER_BOUND('',#2094,.T.);
#1343=FACE_OUTER_BOUND('',#2095,.T.);
#1344=FACE_OUTER_BOUND('',#2096,.T.);
#1345=FACE_OUTER_BOUND('',#2097,.T.);
#1346=FACE_OUTER_BOUND('',#2098,.T.);
#1347=FACE_OUTER_BOUND('',#2099,.T.);
#1348=FACE_OUTER_BOUND('',#2100,.T.);
#1349=FACE_OUTER_BOUND('',#2101,.T.);
#1350=FACE_OUTER_BOUND('',#2102,.T.);
#1351=FACE_OUTER_BOUND('',#2103,.T.);
#1352=FACE_OUTER_BOUND('',#2104,.T.);
#1353=FACE_OUTER_BOUND('',#2105,.T.);
#1354=FACE_OUTER_BOUND('',#2106,.T.);
#1355=FACE_OUTER_BOUND('',#2107,.T.);
#1356=FACE_OUTER_BOUND('',#2108,.T.);
#1357=FACE_OUTER_BOUND('',#2109,.T.);
#1358=FACE_OUTER_BOUND('',#2110,.T.);
#1359=FACE_OUTER_BOUND('',#2111,.T.);
#1360=FACE_OUTER_BOUND('',#2112,.T.);
#1361=FACE_OUTER_BOUND('',#2113,.T.);
#1362=FACE_OUTER_BOUND('',#2114,.T.);
#1363=FACE_OUTER_BOUND('',#2115,.T.);
#1364=FACE_OUTER_BOUND('',#2116,.T.);
#1365=FACE_OUTER_BOUND('',#2117,.T.);
#1366=FACE_OUTER_BOUND('',#2118,.T.);
#1367=FACE_OUTER_BOUND('',#2119,.T.);
#1368=FACE_OUTER_BOUND('',#2120,.T.);
#1369=FACE_OUTER_BOUND('',#2121,.T.);
#1370=FACE_OUTER_BOUND('',#2122,.T.);
#1371=FACE_OUTER_BOUND('',#2123,.T.);
#1372=FACE_OUTER_BOUND('',#2124,.T.);
#1373=FACE_OUTER_BOUND('',#2125,.T.);
#1374=FACE_OUTER_BOUND('',#2126,.T.);
#1375=FACE_OUTER_BOUND('',#2127,.T.);
#1376=FACE_OUTER_BOUND('',#2128,.T.);
#1377=FACE_OUTER_BOUND('',#2129,.T.);
#1378=FACE_OUTER_BOUND('',#2130,.T.);
#1379=FACE_OUTER_BOUND('',#2131,.T.);
#1380=FACE_OUTER_BOUND('',#2132,.T.);
#1381=FACE_OUTER_BOUND('',#2133,.T.);
#1382=FACE_OUTER_BOUND('',#2134,.T.);
#1383=FACE_OUTER_BOUND('',#2135,.T.);
#1384=FACE_OUTER_BOUND('',#2136,.T.);
#1385=FACE_OUTER_BOUND('',#2137,.T.);
#1386=FACE_OUTER_BOUND('',#2138,.T.);
#1387=FACE_OUTER_BOUND('',#2139,.T.);
#1388=FACE_OUTER_BOUND('',#2140,.T.);
#1389=FACE_OUTER_BOUND('',#2141,.T.);
#1390=FACE_OUTER_BOUND('',#2142,.T.);
#1391=FACE_OUTER_BOUND('',#2143,.T.);
#1392=FACE_OUTER_BOUND('',#2144,.T.);
#1393=FACE_OUTER_BOUND('',#2145,.T.);
#1394=FACE_OUTER_BOUND('',#2146,.T.);
#1395=FACE_OUTER_BOUND('',#2147,.T.);
#1396=FACE_OUTER_BOUND('',#2148,.T.);
#1397=FACE_OUTER_BOUND('',#2149,.T.);
#1398=FACE_OUTER_BOUND('',#2150,.T.);
#1399=FACE_OUTER_BOUND('',#2151,.T.);
#1400=FACE_OUTER_BOUND('',#2152,.T.);
#1401=FACE_OUTER_BOUND('',#2153,.T.);
#1402=FACE_OUTER_BOUND('',#2154,.T.);
#1403=FACE_OUTER_BOUND('',#2155,.T.);
#1404=FACE_OUTER_BOUND('',#2156,.T.);
#1405=FACE_OUTER_BOUND('',#2157,.T.);
#1406=FACE_OUTER_BOUND('',#2158,.T.);
#1407=FACE_OUTER_BOUND('',#2159,.T.);
#1408=FACE_OUTER_BOUND('',#2160,.T.);
#1409=FACE_OUTER_BOUND('',#2161,.T.);
#1410=FACE_OUTER_BOUND('',#2162,.T.);
#1411=FACE_OUTER_BOUND('',#2163,.T.);
#1412=FACE_OUTER_BOUND('',#2164,.T.);
#1413=FACE_OUTER_BOUND('',#2165,.T.);
#1414=FACE_OUTER_BOUND('',#2166,.T.);
#1415=FACE_OUTER_BOUND('',#2167,.T.);
#1416=FACE_OUTER_BOUND('',#2168,.T.);
#1417=FACE_OUTER_BOUND('',#2169,.T.);
#1418=FACE_OUTER_BOUND('',#2170,.T.);
#1419=FACE_OUTER_BOUND('',#2171,.T.);
#1420=FACE_OUTER_BOUND('',#2172,.T.);
#1421=FACE_OUTER_BOUND('',#2173,.T.);
#1422=FACE_OUTER_BOUND('',#2174,.T.);
#1423=FACE_OUTER_BOUND('',#2175,.T.);
#1424=FACE_OUTER_BOUND('',#2176,.T.);
#1425=FACE_OUTER_BOUND('',#2178,.T.);
#1426=FACE_OUTER_BOUND('',#2180,.T.);
#1427=FACE_OUTER_BOUND('',#2181,.T.);
#1428=FACE_OUTER_BOUND('',#2182,.T.);
#1429=FACE_OUTER_BOUND('',#2183,.T.);
#1430=FACE_OUTER_BOUND('',#2184,.T.);
#1431=FACE_OUTER_BOUND('',#2185,.T.);
#1432=FACE_OUTER_BOUND('',#2186,.T.);
#1433=FACE_OUTER_BOUND('',#2187,.T.);
#1434=FACE_OUTER_BOUND('',#2188,.T.);
#1435=FACE_OUTER_BOUND('',#2189,.T.);
#1436=FACE_OUTER_BOUND('',#2190,.T.);
#1437=FACE_OUTER_BOUND('',#2191,.T.);
#1438=FACE_OUTER_BOUND('',#2192,.T.);
#1439=FACE_OUTER_BOUND('',#2193,.T.);
#1440=FACE_OUTER_BOUND('',#2194,.T.);
#1441=FACE_OUTER_BOUND('',#2195,.T.);
#1442=FACE_OUTER_BOUND('',#2196,.T.);
#1443=FACE_OUTER_BOUND('',#2197,.T.);
#1444=FACE_OUTER_BOUND('',#2198,.T.);
#1445=FACE_OUTER_BOUND('',#2199,.T.);
#1446=FACE_OUTER_BOUND('',#2200,.T.);
#1447=FACE_OUTER_BOUND('',#2201,.T.);
#1448=FACE_OUTER_BOUND('',#2202,.T.);
#1449=FACE_OUTER_BOUND('',#2203,.T.);
#1450=FACE_OUTER_BOUND('',#2204,.T.);
#1451=FACE_OUTER_BOUND('',#2205,.T.);
#1452=FACE_OUTER_BOUND('',#2206,.T.);
#1453=FACE_OUTER_BOUND('',#2207,.T.);
#1454=FACE_OUTER_BOUND('',#2208,.T.);
#1455=FACE_OUTER_BOUND('',#2209,.T.);
#1456=FACE_OUTER_BOUND('',#2210,.T.);
#1457=FACE_OUTER_BOUND('',#2211,.T.);
#1458=FACE_OUTER_BOUND('',#2212,.T.);
#1459=FACE_OUTER_BOUND('',#2213,.T.);
#1460=FACE_OUTER_BOUND('',#2214,.T.);
#1461=FACE_OUTER_BOUND('',#2215,.T.);
#1462=FACE_OUTER_BOUND('',#2216,.T.);
#1463=FACE_OUTER_BOUND('',#2217,.T.);
#1464=FACE_OUTER_BOUND('',#2218,.T.);
#1465=FACE_OUTER_BOUND('',#2219,.T.);
#1466=FACE_OUTER_BOUND('',#2220,.T.);
#1467=FACE_OUTER_BOUND('',#2221,.T.);
#1468=FACE_OUTER_BOUND('',#2222,.T.);
#1469=FACE_OUTER_BOUND('',#2223,.T.);
#1470=FACE_OUTER_BOUND('',#2224,.T.);
#1471=FACE_OUTER_BOUND('',#2225,.T.);
#1472=FACE_OUTER_BOUND('',#2226,.T.);
#1473=FACE_OUTER_BOUND('',#2227,.T.);
#1474=FACE_OUTER_BOUND('',#2228,.T.);
#1475=FACE_OUTER_BOUND('',#2229,.T.);
#1476=FACE_OUTER_BOUND('',#2230,.T.);
#1477=FACE_OUTER_BOUND('',#2231,.T.);
#1478=FACE_OUTER_BOUND('',#2232,.T.);
#1479=FACE_OUTER_BOUND('',#2233,.T.);
#1480=FACE_OUTER_BOUND('',#2234,.T.);
#1481=FACE_OUTER_BOUND('',#2235,.T.);
#1482=FACE_OUTER_BOUND('',#2236,.T.);
#1483=FACE_OUTER_BOUND('',#2237,.T.);
#1484=FACE_OUTER_BOUND('',#2238,.T.);
#1485=FACE_OUTER_BOUND('',#2239,.T.);
#1486=FACE_OUTER_BOUND('',#2240,.T.);
#1487=FACE_OUTER_BOUND('',#2241,.T.);
#1488=FACE_OUTER_BOUND('',#2242,.T.);
#1489=FACE_OUTER_BOUND('',#2243,.T.);
#1490=FACE_OUTER_BOUND('',#2244,.T.);
#1491=FACE_OUTER_BOUND('',#2245,.T.);
#1492=FACE_OUTER_BOUND('',#2246,.T.);
#1493=FACE_OUTER_BOUND('',#2247,.T.);
#1494=FACE_OUTER_BOUND('',#2248,.T.);
#1495=FACE_OUTER_BOUND('',#2249,.T.);
#1496=FACE_OUTER_BOUND('',#2250,.T.);
#1497=FACE_OUTER_BOUND('',#2251,.T.);
#1498=FACE_OUTER_BOUND('',#2252,.T.);
#1499=FACE_OUTER_BOUND('',#2253,.T.);
#1500=FACE_OUTER_BOUND('',#2254,.T.);
#1501=FACE_OUTER_BOUND('',#2255,.T.);
#1502=FACE_OUTER_BOUND('',#2256,.T.);
#1503=FACE_OUTER_BOUND('',#2257,.T.);
#1504=FACE_OUTER_BOUND('',#2258,.T.);
#1505=FACE_OUTER_BOUND('',#2259,.T.);
#1506=FACE_OUTER_BOUND('',#2260,.T.);
#1507=FACE_OUTER_BOUND('',#2261,.T.);
#1508=FACE_OUTER_BOUND('',#2262,.T.);
#1509=FACE_OUTER_BOUND('',#2263,.T.);
#1510=FACE_OUTER_BOUND('',#2264,.T.);
#1511=FACE_OUTER_BOUND('',#2265,.T.);
#1512=FACE_OUTER_BOUND('',#2266,.T.);
#1513=FACE_OUTER_BOUND('',#2267,.T.);
#1514=FACE_OUTER_BOUND('',#2268,.T.);
#1515=FACE_OUTER_BOUND('',#2269,.T.);
#1516=FACE_OUTER_BOUND('',#2270,.T.);
#1517=FACE_OUTER_BOUND('',#2271,.T.);
#1518=FACE_OUTER_BOUND('',#2272,.T.);
#1519=FACE_OUTER_BOUND('',#2273,.T.);
#1520=FACE_OUTER_BOUND('',#2274,.T.);
#1521=FACE_OUTER_BOUND('',#2276,.T.);
#1522=FACE_OUTER_BOUND('',#2278,.T.);
#1523=FACE_OUTER_BOUND('',#2279,.T.);
#1524=FACE_OUTER_BOUND('',#2280,.T.);
#1525=FACE_OUTER_BOUND('',#2281,.T.);
#1526=FACE_OUTER_BOUND('',#2282,.T.);
#1527=FACE_OUTER_BOUND('',#2283,.T.);
#1528=FACE_OUTER_BOUND('',#2284,.T.);
#1529=FACE_OUTER_BOUND('',#2285,.T.);
#1530=FACE_OUTER_BOUND('',#2286,.T.);
#1531=FACE_OUTER_BOUND('',#2287,.T.);
#1532=FACE_OUTER_BOUND('',#2288,.T.);
#1533=FACE_OUTER_BOUND('',#2289,.T.);
#1534=FACE_OUTER_BOUND('',#2290,.T.);
#1535=FACE_OUTER_BOUND('',#2291,.T.);
#1536=FACE_OUTER_BOUND('',#2292,.T.);
#1537=FACE_OUTER_BOUND('',#2293,.T.);
#1538=FACE_OUTER_BOUND('',#2294,.T.);
#1539=FACE_OUTER_BOUND('',#2295,.T.);
#1540=FACE_OUTER_BOUND('',#2296,.T.);
#1541=FACE_OUTER_BOUND('',#2297,.T.);
#1542=FACE_OUTER_BOUND('',#2298,.T.);
#1543=FACE_OUTER_BOUND('',#2299,.T.);
#1544=FACE_OUTER_BOUND('',#2300,.T.);
#1545=FACE_OUTER_BOUND('',#2301,.T.);
#1546=FACE_OUTER_BOUND('',#2302,.T.);
#1547=FACE_OUTER_BOUND('',#2303,.T.);
#1548=FACE_OUTER_BOUND('',#2305,.T.);
#1549=FACE_OUTER_BOUND('',#2307,.T.);
#1550=FACE_OUTER_BOUND('',#2308,.T.);
#1551=FACE_OUTER_BOUND('',#2309,.T.);
#1552=FACE_OUTER_BOUND('',#2310,.T.);
#1553=FACE_OUTER_BOUND('',#2311,.T.);
#1554=FACE_OUTER_BOUND('',#2312,.T.);
#1555=FACE_OUTER_BOUND('',#2313,.T.);
#1556=FACE_OUTER_BOUND('',#2314,.T.);
#1557=FACE_OUTER_BOUND('',#2315,.T.);
#1558=FACE_OUTER_BOUND('',#2316,.T.);
#1559=FACE_OUTER_BOUND('',#2317,.T.);
#1560=FACE_OUTER_BOUND('',#2318,.T.);
#1561=FACE_OUTER_BOUND('',#2319,.T.);
#1562=FACE_OUTER_BOUND('',#2320,.T.);
#1563=FACE_OUTER_BOUND('',#2321,.T.);
#1564=FACE_OUTER_BOUND('',#2322,.T.);
#1565=FACE_OUTER_BOUND('',#2323,.T.);
#1566=FACE_OUTER_BOUND('',#2324,.T.);
#1567=FACE_OUTER_BOUND('',#2325,.T.);
#1568=FACE_OUTER_BOUND('',#2326,.T.);
#1569=FACE_OUTER_BOUND('',#2327,.T.);
#1570=FACE_OUTER_BOUND('',#2328,.T.);
#1571=FACE_OUTER_BOUND('',#2330,.T.);
#1572=FACE_OUTER_BOUND('',#2332,.T.);
#1573=FACE_OUTER_BOUND('',#2334,.T.);
#1574=FACE_OUTER_BOUND('',#2336,.T.);
#1575=FACE_OUTER_BOUND('',#2338,.T.);
#1576=FACE_OUTER_BOUND('',#2340,.T.);
#1577=FACE_OUTER_BOUND('',#2343,.T.);
#1578=FACE_OUTER_BOUND('',#2346,.T.);
#1579=FACE_OUTER_BOUND('',#2349,.T.);
#1580=FACE_OUTER_BOUND('',#2352,.T.);
#1581=FACE_OUTER_BOUND('',#2355,.T.);
#1582=FACE_OUTER_BOUND('',#2358,.T.);
#1583=FACE_OUTER_BOUND('',#2361,.T.);
#1584=FACE_OUTER_BOUND('',#2364,.T.);
#1585=FACE_OUTER_BOUND('',#2367,.T.);
#1586=FACE_OUTER_BOUND('',#2370,.T.);
#1587=FACE_OUTER_BOUND('',#2373,.T.);
#1588=FACE_OUTER_BOUND('',#2376,.T.);
#1589=FACE_OUTER_BOUND('',#2379,.T.);
#1590=FACE_OUTER_BOUND('',#2382,.T.);
#1591=FACE_OUTER_BOUND('',#2383,.T.);
#1592=FACE_OUTER_BOUND('',#2384,.T.);
#1593=FACE_OUTER_BOUND('',#2385,.T.);
#1594=FACE_OUTER_BOUND('',#2386,.T.);
#1595=FACE_OUTER_BOUND('',#2388,.T.);
#1596=FACE_OUTER_BOUND('',#2390,.T.);
#1597=FACE_OUTER_BOUND('',#2391,.T.);
#1598=FACE_OUTER_BOUND('',#2392,.T.);
#1599=FACE_OUTER_BOUND('',#2393,.T.);
#1600=FACE_OUTER_BOUND('',#2394,.T.);
#1601=FACE_OUTER_BOUND('',#2396,.T.);
#1602=FACE_OUTER_BOUND('',#2398,.T.);
#1603=FACE_OUTER_BOUND('',#2399,.T.);
#1604=FACE_OUTER_BOUND('',#2400,.T.);
#1605=FACE_OUTER_BOUND('',#2401,.T.);
#1606=FACE_OUTER_BOUND('',#2402,.T.);
#1607=FACE_OUTER_BOUND('',#2403,.T.);
#1608=FACE_OUTER_BOUND('',#2404,.T.);
#1609=FACE_OUTER_BOUND('',#2405,.T.);
#1610=FACE_OUTER_BOUND('',#2406,.T.);
#1611=FACE_OUTER_BOUND('',#2408,.T.);
#1612=FACE_OUTER_BOUND('',#2410,.T.);
#1613=FACE_OUTER_BOUND('',#2411,.T.);
#1614=FACE_OUTER_BOUND('',#2412,.T.);
#1615=FACE_OUTER_BOUND('',#2413,.T.);
#1616=FACE_OUTER_BOUND('',#2414,.T.);
#1617=FACE_OUTER_BOUND('',#2415,.T.);
#1618=FACE_OUTER_BOUND('',#2416,.T.);
#1619=FACE_OUTER_BOUND('',#2417,.T.);
#1620=FACE_OUTER_BOUND('',#2418,.T.);
#1621=FACE_OUTER_BOUND('',#2420,.T.);
#1622=FACE_OUTER_BOUND('',#2422,.T.);
#1623=FACE_OUTER_BOUND('',#2423,.T.);
#1624=FACE_OUTER_BOUND('',#2424,.T.);
#1625=FACE_OUTER_BOUND('',#2425,.T.);
#1626=FACE_OUTER_BOUND('',#2426,.T.);
#1627=FACE_OUTER_BOUND('',#2427,.T.);
#1628=FACE_OUTER_BOUND('',#2428,.T.);
#1629=FACE_OUTER_BOUND('',#2429,.T.);
#1630=FACE_OUTER_BOUND('',#2430,.T.);
#1631=FACE_OUTER_BOUND('',#2432,.T.);
#1632=FACE_OUTER_BOUND('',#2434,.T.);
#1633=FACE_OUTER_BOUND('',#2435,.T.);
#1634=FACE_OUTER_BOUND('',#2436,.T.);
#1635=FACE_OUTER_BOUND('',#2437,.T.);
#1636=FACE_OUTER_BOUND('',#2438,.T.);
#1637=FACE_OUTER_BOUND('',#2439,.T.);
#1638=FACE_OUTER_BOUND('',#2440,.T.);
#1639=FACE_OUTER_BOUND('',#2441,.T.);
#1640=FACE_OUTER_BOUND('',#2442,.T.);
#1641=FACE_OUTER_BOUND('',#2444,.T.);
#1642=FACE_OUTER_BOUND('',#2446,.T.);
#1643=FACE_OUTER_BOUND('',#2447,.T.);
#1644=FACE_OUTER_BOUND('',#2448,.T.);
#1645=FACE_OUTER_BOUND('',#2449,.T.);
#1646=FACE_OUTER_BOUND('',#2450,.T.);
#1647=FACE_OUTER_BOUND('',#2451,.T.);
#1648=FACE_OUTER_BOUND('',#2452,.T.);
#1649=FACE_OUTER_BOUND('',#2453,.T.);
#1650=FACE_OUTER_BOUND('',#2454,.T.);
#1651=FACE_OUTER_BOUND('',#2456,.T.);
#1652=FACE_OUTER_BOUND('',#2458,.T.);
#1653=FACE_OUTER_BOUND('',#2459,.T.);
#1654=FACE_OUTER_BOUND('',#2460,.T.);
#1655=FACE_OUTER_BOUND('',#2461,.T.);
#1656=FACE_OUTER_BOUND('',#2462,.T.);
#1657=FACE_OUTER_BOUND('',#2463,.T.);
#1658=FACE_OUTER_BOUND('',#2464,.T.);
#1659=FACE_OUTER_BOUND('',#2465,.T.);
#1660=FACE_OUTER_BOUND('',#2466,.T.);
#1661=FACE_OUTER_BOUND('',#2467,.T.);
#1662=FACE_OUTER_BOUND('',#2468,.T.);
#1663=FACE_OUTER_BOUND('',#2469,.T.);
#1664=FACE_OUTER_BOUND('',#2470,.T.);
#1665=FACE_OUTER_BOUND('',#2471,.T.);
#1666=FACE_OUTER_BOUND('',#2472,.T.);
#1667=FACE_OUTER_BOUND('',#2473,.T.);
#1668=FACE_OUTER_BOUND('',#2474,.T.);
#1669=FACE_OUTER_BOUND('',#2476,.T.);
#1670=FACE_OUTER_BOUND('',#2478,.T.);
#1671=FACE_OUTER_BOUND('',#2479,.T.);
#1672=FACE_OUTER_BOUND('',#2480,.T.);
#1673=FACE_OUTER_BOUND('',#2481,.T.);
#1674=FACE_OUTER_BOUND('',#2482,.T.);
#1675=FACE_OUTER_BOUND('',#2483,.T.);
#1676=FACE_OUTER_BOUND('',#2484,.T.);
#1677=FACE_OUTER_BOUND('',#2485,.T.);
#1678=FACE_OUTER_BOUND('',#2486,.T.);
#1679=FACE_OUTER_BOUND('',#2487,.T.);
#1680=FACE_OUTER_BOUND('',#2488,.T.);
#1681=FACE_OUTER_BOUND('',#2489,.T.);
#1682=FACE_OUTER_BOUND('',#2490,.T.);
#1683=FACE_OUTER_BOUND('',#2491,.T.);
#1684=FACE_OUTER_BOUND('',#2492,.T.);
#1685=FACE_OUTER_BOUND('',#2493,.T.);
#1686=FACE_OUTER_BOUND('',#2494,.T.);
#1687=FACE_OUTER_BOUND('',#2495,.T.);
#1688=FACE_OUTER_BOUND('',#2496,.T.);
#1689=FACE_OUTER_BOUND('',#2497,.T.);
#1690=FACE_OUTER_BOUND('',#2498,.T.);
#1691=FACE_OUTER_BOUND('',#2499,.T.);
#1692=FACE_OUTER_BOUND('',#2501,.T.);
#1693=FACE_OUTER_BOUND('',#2503,.T.);
#1694=FACE_OUTER_BOUND('',#2505,.T.);
#1695=FACE_OUTER_BOUND('',#2507,.T.);
#1696=FACE_OUTER_BOUND('',#2509,.T.);
#1697=FACE_OUTER_BOUND('',#2511,.T.);
#1698=FACE_OUTER_BOUND('',#2514,.T.);
#1699=FACE_OUTER_BOUND('',#2517,.T.);
#1700=FACE_OUTER_BOUND('',#2520,.T.);
#1701=FACE_OUTER_BOUND('',#2523,.T.);
#1702=FACE_OUTER_BOUND('',#2526,.T.);
#1703=FACE_OUTER_BOUND('',#2529,.T.);
#1704=FACE_OUTER_BOUND('',#2532,.T.);
#1705=FACE_OUTER_BOUND('',#2535,.T.);
#1706=FACE_OUTER_BOUND('',#2538,.T.);
#1707=FACE_OUTER_BOUND('',#2541,.T.);
#1708=FACE_OUTER_BOUND('',#2544,.T.);
#1709=FACE_OUTER_BOUND('',#2547,.T.);
#1710=FACE_OUTER_BOUND('',#2550,.T.);
#1711=FACE_OUTER_BOUND('',#2553,.T.);
#1712=FACE_OUTER_BOUND('',#2554,.T.);
#1713=FACE_OUTER_BOUND('',#2555,.T.);
#1714=FACE_OUTER_BOUND('',#2556,.T.);
#1715=FACE_OUTER_BOUND('',#2557,.T.);
#1716=FACE_OUTER_BOUND('',#2559,.T.);
#1717=FACE_OUTER_BOUND('',#2561,.T.);
#1718=FACE_OUTER_BOUND('',#2562,.T.);
#1719=FACE_OUTER_BOUND('',#2563,.T.);
#1720=FACE_OUTER_BOUND('',#2564,.T.);
#1721=FACE_OUTER_BOUND('',#2565,.T.);
#1722=FACE_OUTER_BOUND('',#2567,.T.);
#1723=FACE_OUTER_BOUND('',#2569,.T.);
#1724=FACE_OUTER_BOUND('',#2570,.T.);
#1725=FACE_OUTER_BOUND('',#2571,.T.);
#1726=FACE_OUTER_BOUND('',#2572,.T.);
#1727=FACE_OUTER_BOUND('',#2573,.T.);
#1728=FACE_OUTER_BOUND('',#2574,.T.);
#1729=FACE_OUTER_BOUND('',#2575,.T.);
#1730=FACE_OUTER_BOUND('',#2576,.T.);
#1731=FACE_OUTER_BOUND('',#2577,.T.);
#1732=FACE_OUTER_BOUND('',#2579,.T.);
#1733=FACE_OUTER_BOUND('',#2581,.T.);
#1734=FACE_OUTER_BOUND('',#2582,.T.);
#1735=FACE_OUTER_BOUND('',#2583,.T.);
#1736=FACE_OUTER_BOUND('',#2584,.T.);
#1737=FACE_OUTER_BOUND('',#2585,.T.);
#1738=FACE_OUTER_BOUND('',#2586,.T.);
#1739=FACE_OUTER_BOUND('',#2587,.T.);
#1740=FACE_OUTER_BOUND('',#2588,.T.);
#1741=FACE_OUTER_BOUND('',#2589,.T.);
#1742=FACE_OUTER_BOUND('',#2591,.T.);
#1743=FACE_OUTER_BOUND('',#2593,.T.);
#1744=FACE_OUTER_BOUND('',#2594,.T.);
#1745=FACE_OUTER_BOUND('',#2595,.T.);
#1746=FACE_OUTER_BOUND('',#2596,.T.);
#1747=FACE_OUTER_BOUND('',#2597,.T.);
#1748=FACE_OUTER_BOUND('',#2598,.T.);
#1749=FACE_OUTER_BOUND('',#2599,.T.);
#1750=FACE_OUTER_BOUND('',#2600,.T.);
#1751=FACE_OUTER_BOUND('',#2601,.T.);
#1752=FACE_OUTER_BOUND('',#2603,.T.);
#1753=FACE_OUTER_BOUND('',#2605,.T.);
#1754=FACE_OUTER_BOUND('',#2606,.T.);
#1755=FACE_OUTER_BOUND('',#2607,.T.);
#1756=FACE_OUTER_BOUND('',#2608,.T.);
#1757=FACE_OUTER_BOUND('',#2609,.T.);
#1758=FACE_OUTER_BOUND('',#2610,.T.);
#1759=FACE_OUTER_BOUND('',#2611,.T.);
#1760=FACE_OUTER_BOUND('',#2612,.T.);
#1761=FACE_OUTER_BOUND('',#2613,.T.);
#1762=FACE_OUTER_BOUND('',#2615,.T.);
#1763=FACE_OUTER_BOUND('',#2617,.T.);
#1764=FACE_OUTER_BOUND('',#2618,.T.);
#1765=FACE_OUTER_BOUND('',#2619,.T.);
#1766=FACE_OUTER_BOUND('',#2620,.T.);
#1767=FACE_OUTER_BOUND('',#2621,.T.);
#1768=FACE_OUTER_BOUND('',#2622,.T.);
#1769=FACE_OUTER_BOUND('',#2623,.T.);
#1770=FACE_OUTER_BOUND('',#2624,.T.);
#1771=FACE_OUTER_BOUND('',#2625,.T.);
#1772=FACE_OUTER_BOUND('',#2627,.T.);
#1773=FACE_OUTER_BOUND('',#2629,.T.);
#1774=FACE_OUTER_BOUND('',#2630,.T.);
#1775=FACE_OUTER_BOUND('',#2631,.T.);
#1776=FACE_OUTER_BOUND('',#2632,.T.);
#1777=FACE_OUTER_BOUND('',#2633,.T.);
#1778=FACE_OUTER_BOUND('',#2634,.T.);
#1779=FACE_OUTER_BOUND('',#2635,.T.);
#1780=FACE_OUTER_BOUND('',#2636,.T.);
#1781=FACE_OUTER_BOUND('',#2637,.T.);
#1782=FACE_OUTER_BOUND('',#2638,.T.);
#1783=FACE_OUTER_BOUND('',#2639,.T.);
#1784=FACE_OUTER_BOUND('',#2640,.T.);
#1785=FACE_OUTER_BOUND('',#2641,.T.);
#1786=FACE_OUTER_BOUND('',#2642,.T.);
#1787=FACE_OUTER_BOUND('',#2643,.T.);
#1788=FACE_OUTER_BOUND('',#2644,.T.);
#1789=FACE_OUTER_BOUND('',#2645,.T.);
#1790=FACE_OUTER_BOUND('',#2647,.T.);
#1791=FACE_OUTER_BOUND('',#2649,.T.);
#1792=FACE_OUTER_BOUND('',#2650,.T.);
#1793=FACE_OUTER_BOUND('',#2651,.T.);
#1794=FACE_OUTER_BOUND('',#2652,.T.);
#1795=FACE_OUTER_BOUND('',#2653,.T.);
#1796=FACE_OUTER_BOUND('',#2654,.T.);
#1797=FACE_OUTER_BOUND('',#2655,.T.);
#1798=FACE_OUTER_BOUND('',#2656,.T.);
#1799=FACE_OUTER_BOUND('',#2657,.T.);
#1800=FACE_OUTER_BOUND('',#2658,.T.);
#1801=FACE_OUTER_BOUND('',#2659,.T.);
#1802=FACE_OUTER_BOUND('',#2660,.T.);
#1803=FACE_OUTER_BOUND('',#2661,.T.);
#1804=FACE_OUTER_BOUND('',#2662,.T.);
#1805=FACE_OUTER_BOUND('',#2663,.T.);
#1806=FACE_OUTER_BOUND('',#2664,.T.);
#1807=FACE_OUTER_BOUND('',#2665,.T.);
#1808=FACE_OUTER_BOUND('',#2666,.T.);
#1809=FACE_OUTER_BOUND('',#2667,.T.);
#1810=FACE_OUTER_BOUND('',#2668,.T.);
#1811=FACE_OUTER_BOUND('',#2669,.T.);
#1812=FACE_OUTER_BOUND('',#2670,.T.);
#1813=FACE_OUTER_BOUND('',#2672,.T.);
#1814=FACE_OUTER_BOUND('',#2674,.T.);
#1815=FACE_OUTER_BOUND('',#2676,.T.);
#1816=FACE_OUTER_BOUND('',#2678,.T.);
#1817=FACE_OUTER_BOUND('',#2680,.T.);
#1818=FACE_OUTER_BOUND('',#2682,.T.);
#1819=FACE_OUTER_BOUND('',#2685,.T.);
#1820=FACE_OUTER_BOUND('',#2688,.T.);
#1821=FACE_OUTER_BOUND('',#2691,.T.);
#1822=FACE_OUTER_BOUND('',#2694,.T.);
#1823=FACE_OUTER_BOUND('',#2697,.T.);
#1824=FACE_OUTER_BOUND('',#2700,.T.);
#1825=FACE_OUTER_BOUND('',#2703,.T.);
#1826=FACE_OUTER_BOUND('',#2706,.T.);
#1827=FACE_OUTER_BOUND('',#2709,.T.);
#1828=FACE_OUTER_BOUND('',#2712,.T.);
#1829=FACE_OUTER_BOUND('',#2715,.T.);
#1830=FACE_OUTER_BOUND('',#2718,.T.);
#1831=FACE_OUTER_BOUND('',#2721,.T.);
#1832=FACE_OUTER_BOUND('',#2724,.T.);
#1833=FACE_OUTER_BOUND('',#2725,.T.);
#1834=FACE_OUTER_BOUND('',#2726,.T.);
#1835=FACE_OUTER_BOUND('',#2727,.T.);
#1836=FACE_OUTER_BOUND('',#2728,.T.);
#1837=FACE_OUTER_BOUND('',#2730,.T.);
#1838=FACE_OUTER_BOUND('',#2732,.T.);
#1839=FACE_OUTER_BOUND('',#2733,.T.);
#1840=FACE_OUTER_BOUND('',#2734,.T.);
#1841=FACE_OUTER_BOUND('',#2735,.T.);
#1842=FACE_OUTER_BOUND('',#2736,.T.);
#1843=FACE_OUTER_BOUND('',#2738,.T.);
#1844=FACE_OUTER_BOUND('',#2740,.T.);
#1845=FACE_OUTER_BOUND('',#2741,.T.);
#1846=FACE_OUTER_BOUND('',#2742,.T.);
#1847=FACE_OUTER_BOUND('',#2743,.T.);
#1848=FACE_OUTER_BOUND('',#2744,.T.);
#1849=FACE_OUTER_BOUND('',#2745,.T.);
#1850=FACE_OUTER_BOUND('',#2746,.T.);
#1851=FACE_OUTER_BOUND('',#2747,.T.);
#1852=FACE_OUTER_BOUND('',#2748,.T.);
#1853=FACE_OUTER_BOUND('',#2750,.T.);
#1854=FACE_OUTER_BOUND('',#2752,.T.);
#1855=FACE_OUTER_BOUND('',#2753,.T.);
#1856=FACE_OUTER_BOUND('',#2754,.T.);
#1857=FACE_OUTER_BOUND('',#2755,.T.);
#1858=FACE_OUTER_BOUND('',#2756,.T.);
#1859=FACE_OUTER_BOUND('',#2757,.T.);
#1860=FACE_OUTER_BOUND('',#2758,.T.);
#1861=FACE_OUTER_BOUND('',#2759,.T.);
#1862=FACE_OUTER_BOUND('',#2760,.T.);
#1863=FACE_OUTER_BOUND('',#2762,.T.);
#1864=FACE_OUTER_BOUND('',#2764,.T.);
#1865=FACE_OUTER_BOUND('',#2765,.T.);
#1866=FACE_OUTER_BOUND('',#2766,.T.);
#1867=FACE_OUTER_BOUND('',#2767,.T.);
#1868=FACE_OUTER_BOUND('',#2768,.T.);
#1869=FACE_OUTER_BOUND('',#2769,.T.);
#1870=FACE_OUTER_BOUND('',#2770,.T.);
#1871=FACE_OUTER_BOUND('',#2771,.T.);
#1872=FACE_OUTER_BOUND('',#2772,.T.);
#1873=FACE_OUTER_BOUND('',#2774,.T.);
#1874=FACE_OUTER_BOUND('',#2776,.T.);
#1875=FACE_OUTER_BOUND('',#2777,.T.);
#1876=FACE_OUTER_BOUND('',#2778,.T.);
#1877=FACE_OUTER_BOUND('',#2779,.T.);
#1878=FACE_OUTER_BOUND('',#2780,.T.);
#1879=FACE_OUTER_BOUND('',#2781,.T.);
#1880=FACE_OUTER_BOUND('',#2782,.T.);
#1881=FACE_OUTER_BOUND('',#2783,.T.);
#1882=FACE_OUTER_BOUND('',#2784,.T.);
#1883=FACE_OUTER_BOUND('',#2786,.T.);
#1884=FACE_OUTER_BOUND('',#2788,.T.);
#1885=FACE_OUTER_BOUND('',#2789,.T.);
#1886=FACE_OUTER_BOUND('',#2790,.T.);
#1887=FACE_OUTER_BOUND('',#2791,.T.);
#1888=FACE_OUTER_BOUND('',#2792,.T.);
#1889=FACE_OUTER_BOUND('',#2793,.T.);
#1890=FACE_OUTER_BOUND('',#2794,.T.);
#1891=FACE_OUTER_BOUND('',#2795,.T.);
#1892=FACE_OUTER_BOUND('',#2796,.T.);
#1893=FACE_OUTER_BOUND('',#2798,.T.);
#1894=FACE_OUTER_BOUND('',#2800,.T.);
#1895=FACE_OUTER_BOUND('',#2801,.T.);
#1896=FACE_OUTER_BOUND('',#2802,.T.);
#1897=FACE_OUTER_BOUND('',#2803,.T.);
#1898=FACE_OUTER_BOUND('',#2804,.T.);
#1899=FACE_OUTER_BOUND('',#2805,.T.);
#1900=FACE_OUTER_BOUND('',#2806,.T.);
#1901=FACE_OUTER_BOUND('',#2807,.T.);
#1902=FACE_OUTER_BOUND('',#2808,.T.);
#1903=FACE_OUTER_BOUND('',#2809,.T.);
#1904=FACE_OUTER_BOUND('',#2810,.T.);
#1905=FACE_OUTER_BOUND('',#2811,.T.);
#1906=FACE_OUTER_BOUND('',#2812,.T.);
#1907=FACE_OUTER_BOUND('',#2813,.T.);
#1908=FACE_OUTER_BOUND('',#2814,.T.);
#1909=FACE_OUTER_BOUND('',#2815,.T.);
#1910=FACE_OUTER_BOUND('',#2816,.T.);
#1911=FACE_OUTER_BOUND('',#2818,.T.);
#1912=FACE_OUTER_BOUND('',#2820,.T.);
#1913=FACE_OUTER_BOUND('',#2821,.T.);
#1914=FACE_OUTER_BOUND('',#2822,.T.);
#1915=FACE_OUTER_BOUND('',#2823,.T.);
#1916=FACE_OUTER_BOUND('',#2824,.T.);
#1917=FACE_OUTER_BOUND('',#2825,.T.);
#1918=FACE_OUTER_BOUND('',#2826,.T.);
#1919=FACE_OUTER_BOUND('',#2827,.T.);
#1920=FACE_OUTER_BOUND('',#2828,.T.);
#1921=FACE_OUTER_BOUND('',#2829,.T.);
#1922=FACE_OUTER_BOUND('',#2830,.T.);
#1923=FACE_OUTER_BOUND('',#2831,.T.);
#1924=FACE_OUTER_BOUND('',#2832,.T.);
#1925=FACE_OUTER_BOUND('',#2833,.T.);
#1926=FACE_OUTER_BOUND('',#2834,.T.);
#1927=FACE_OUTER_BOUND('',#2835,.T.);
#1928=FACE_OUTER_BOUND('',#2836,.T.);
#1929=FACE_OUTER_BOUND('',#2837,.T.);
#1930=FACE_OUTER_BOUND('',#2838,.T.);
#1931=FACE_OUTER_BOUND('',#2839,.T.);
#1932=FACE_OUTER_BOUND('',#2840,.T.);
#1933=FACE_OUTER_BOUND('',#2841,.T.);
#1934=FACE_OUTER_BOUND('',#2843,.T.);
#1935=FACE_OUTER_BOUND('',#2845,.T.);
#1936=FACE_OUTER_BOUND('',#2847,.T.);
#1937=FACE_OUTER_BOUND('',#2849,.T.);
#1938=FACE_OUTER_BOUND('',#2851,.T.);
#1939=FACE_OUTER_BOUND('',#2853,.T.);
#1940=FACE_OUTER_BOUND('',#2856,.T.);
#1941=FACE_OUTER_BOUND('',#2859,.T.);
#1942=FACE_OUTER_BOUND('',#2862,.T.);
#1943=FACE_OUTER_BOUND('',#2865,.T.);
#1944=FACE_OUTER_BOUND('',#2868,.T.);
#1945=FACE_OUTER_BOUND('',#2871,.T.);
#1946=FACE_OUTER_BOUND('',#2874,.T.);
#1947=FACE_OUTER_BOUND('',#2877,.T.);
#1948=FACE_OUTER_BOUND('',#2880,.T.);
#1949=FACE_OUTER_BOUND('',#2883,.T.);
#1950=FACE_OUTER_BOUND('',#2886,.T.);
#1951=FACE_OUTER_BOUND('',#2889,.T.);
#1952=FACE_OUTER_BOUND('',#2892,.T.);
#1953=FACE_OUTER_BOUND('',#2895,.T.);
#1954=FACE_OUTER_BOUND('',#2896,.T.);
#1955=FACE_OUTER_BOUND('',#2897,.T.);
#1956=FACE_OUTER_BOUND('',#2898,.T.);
#1957=FACE_OUTER_BOUND('',#2899,.T.);
#1958=FACE_OUTER_BOUND('',#2901,.T.);
#1959=FACE_OUTER_BOUND('',#2903,.T.);
#1960=FACE_OUTER_BOUND('',#2904,.T.);
#1961=FACE_OUTER_BOUND('',#2905,.T.);
#1962=FACE_OUTER_BOUND('',#2906,.T.);
#1963=FACE_OUTER_BOUND('',#2907,.T.);
#1964=FACE_OUTER_BOUND('',#2909,.T.);
#1965=FACE_OUTER_BOUND('',#2911,.T.);
#1966=FACE_OUTER_BOUND('',#2912,.T.);
#1967=FACE_OUTER_BOUND('',#2913,.T.);
#1968=FACE_OUTER_BOUND('',#2914,.T.);
#1969=FACE_OUTER_BOUND('',#2915,.T.);
#1970=FACE_OUTER_BOUND('',#2916,.T.);
#1971=FACE_OUTER_BOUND('',#2917,.T.);
#1972=FACE_OUTER_BOUND('',#2918,.T.);
#1973=FACE_OUTER_BOUND('',#2919,.T.);
#1974=FACE_OUTER_BOUND('',#2921,.T.);
#1975=FACE_OUTER_BOUND('',#2923,.T.);
#1976=FACE_OUTER_BOUND('',#2924,.T.);
#1977=FACE_OUTER_BOUND('',#2925,.T.);
#1978=FACE_OUTER_BOUND('',#2926,.T.);
#1979=FACE_OUTER_BOUND('',#2927,.T.);
#1980=FACE_OUTER_BOUND('',#2928,.T.);
#1981=FACE_OUTER_BOUND('',#2929,.T.);
#1982=FACE_OUTER_BOUND('',#2930,.T.);
#1983=FACE_OUTER_BOUND('',#2931,.T.);
#1984=FACE_OUTER_BOUND('',#2933,.T.);
#1985=FACE_OUTER_BOUND('',#2935,.T.);
#1986=FACE_OUTER_BOUND('',#2936,.T.);
#1987=FACE_OUTER_BOUND('',#2937,.T.);
#1988=FACE_OUTER_BOUND('',#2938,.T.);
#1989=FACE_OUTER_BOUND('',#2939,.T.);
#1990=FACE_OUTER_BOUND('',#2940,.T.);
#1991=FACE_OUTER_BOUND('',#2941,.T.);
#1992=FACE_OUTER_BOUND('',#2942,.T.);
#1993=FACE_OUTER_BOUND('',#2943,.T.);
#1994=FACE_OUTER_BOUND('',#2945,.T.);
#1995=FACE_OUTER_BOUND('',#2947,.T.);
#1996=FACE_OUTER_BOUND('',#2948,.T.);
#1997=FACE_OUTER_BOUND('',#2949,.T.);
#1998=FACE_OUTER_BOUND('',#2950,.T.);
#1999=FACE_OUTER_BOUND('',#2951,.T.);
#2000=FACE_OUTER_BOUND('',#2952,.T.);
#2001=FACE_OUTER_BOUND('',#2953,.T.);
#2002=FACE_OUTER_BOUND('',#2954,.T.);
#2003=FACE_OUTER_BOUND('',#2955,.T.);
#2004=FACE_OUTER_BOUND('',#2957,.T.);
#2005=FACE_OUTER_BOUND('',#2959,.T.);
#2006=FACE_OUTER_BOUND('',#2960,.T.);
#2007=FACE_OUTER_BOUND('',#2961,.T.);
#2008=FACE_OUTER_BOUND('',#2962,.T.);
#2009=FACE_OUTER_BOUND('',#2963,.T.);
#2010=FACE_OUTER_BOUND('',#2964,.T.);
#2011=FACE_OUTER_BOUND('',#2965,.T.);
#2012=FACE_OUTER_BOUND('',#2966,.T.);
#2013=FACE_OUTER_BOUND('',#2967,.T.);
#2014=FACE_OUTER_BOUND('',#2969,.T.);
#2015=FACE_OUTER_BOUND('',#2971,.T.);
#2016=FACE_OUTER_BOUND('',#2972,.T.);
#2017=FACE_OUTER_BOUND('',#2973,.T.);
#2018=FACE_OUTER_BOUND('',#2974,.T.);
#2019=FACE_OUTER_BOUND('',#2975,.T.);
#2020=FACE_OUTER_BOUND('',#2976,.T.);
#2021=FACE_OUTER_BOUND('',#2977,.T.);
#2022=FACE_OUTER_BOUND('',#2978,.T.);
#2023=FACE_OUTER_BOUND('',#2979,.T.);
#2024=FACE_OUTER_BOUND('',#2980,.T.);
#2025=FACE_OUTER_BOUND('',#2983,.T.);
#2026=FACE_OUTER_BOUND('',#2984,.T.);
#2027=FACE_OUTER_BOUND('',#2987,.T.);
#2028=FACE_OUTER_BOUND('',#2988,.T.);
#2029=FACE_OUTER_BOUND('',#2989,.T.);
#2030=FACE_OUTER_BOUND('',#2990,.T.);
#2031=FACE_OUTER_BOUND('',#2991,.T.);
#2032=FACE_OUTER_BOUND('',#2992,.T.);
#2033=FACE_OUTER_BOUND('',#2993,.T.);
#2034=FACE_OUTER_BOUND('',#2996,.T.);
#2035=FACE_OUTER_BOUND('',#2997,.T.);
#2036=FACE_OUTER_BOUND('',#2998,.T.);
#2037=FACE_OUTER_BOUND('',#2999,.T.);
#2038=FACE_OUTER_BOUND('',#3000,.T.);
#2039=EDGE_LOOP('',(#8171,#8172,#8173,#8174));
#2040=EDGE_LOOP('',(#8175,#8176,#8177,#8178));
#2041=EDGE_LOOP('',(#8179));
#2042=EDGE_LOOP('',(#8180));
#2043=EDGE_LOOP('',(#8181,#8182,#8183,#8184));
#2044=EDGE_LOOP('',(#8185,#8186,#8187,#8188));
#2045=EDGE_LOOP('',(#8189,#8190,#8191,#8192));
#2046=EDGE_LOOP('',(#8193,#8194,#8195,#8196));
#2047=EDGE_LOOP('',(#8197,#8198,#8199,#8200));
#2048=EDGE_LOOP('',(#8201,#8202,#8203,#8204));
#2049=EDGE_LOOP('',(#8205,#8206,#8207,#8208));
#2050=EDGE_LOOP('',(#8209,#8210,#8211,#8212));
#2051=EDGE_LOOP('',(#8213,#8214,#8215,#8216));
#2052=EDGE_LOOP('',(#8217,#8218,#8219,#8220));
#2053=EDGE_LOOP('',(#8221,#8222,#8223,#8224));
#2054=EDGE_LOOP('',(#8225,#8226,#8227,#8228));
#2055=EDGE_LOOP('',(#8229,#8230,#8231,#8232));
#2056=EDGE_LOOP('',(#8233,#8234,#8235,#8236));
#2057=EDGE_LOOP('',(#8237,#8238,#8239,#8240));
#2058=EDGE_LOOP('',(#8241,#8242,#8243,#8244));
#2059=EDGE_LOOP('',(#8245,#8246,#8247,#8248));
#2060=EDGE_LOOP('',(#8249,#8250,#8251,#8252));
#2061=EDGE_LOOP('',(#8253,#8254,#8255,#8256));
#2062=EDGE_LOOP('',(#8257,#8258,#8259,#8260));
#2063=EDGE_LOOP('',(#8261,#8262,#8263,#8264));
#2064=EDGE_LOOP('',(#8265,#8266,#8267,#8268));
#2065=EDGE_LOOP('',(#8269,#8270,#8271,#8272));
#2066=EDGE_LOOP('',(#8273,#8274,#8275,#8276));
#2067=EDGE_LOOP('',(#8277,#8278,#8279,#8280));
#2068=EDGE_LOOP('',(#8281,#8282,#8283,#8284));
#2069=EDGE_LOOP('',(#8285,#8286,#8287,#8288));
#2070=EDGE_LOOP('',(#8289,#8290,#8291,#8292));
#2071=EDGE_LOOP('',(#8293,#8294,#8295,#8296));
#2072=EDGE_LOOP('',(#8297,#8298,#8299,#8300));
#2073=EDGE_LOOP('',(#8301,#8302,#8303,#8304));
#2074=EDGE_LOOP('',(#8305,#8306,#8307,#8308));
#2075=EDGE_LOOP('',(#8309,#8310,#8311,#8312));
#2076=EDGE_LOOP('',(#8313,#8314,#8315,#8316));
#2077=EDGE_LOOP('',(#8317,#8318,#8319,#8320));
#2078=EDGE_LOOP('',(#8321,#8322,#8323,#8324));
#2079=EDGE_LOOP('',(#8325,#8326,#8327,#8328));
#2080=EDGE_LOOP('',(#8329,#8330,#8331,#8332));
#2081=EDGE_LOOP('',(#8333,#8334,#8335,#8336));
#2082=EDGE_LOOP('',(#8337,#8338,#8339,#8340));
#2083=EDGE_LOOP('',(#8341,#8342,#8343,#8344));
#2084=EDGE_LOOP('',(#8345,#8346,#8347,#8348));
#2085=EDGE_LOOP('',(#8349,#8350,#8351,#8352));
#2086=EDGE_LOOP('',(#8353,#8354,#8355,#8356));
#2087=EDGE_LOOP('',(#8357,#8358,#8359,#8360));
#2088=EDGE_LOOP('',(#8361,#8362,#8363,#8364));
#2089=EDGE_LOOP('',(#8365,#8366,#8367,#8368));
#2090=EDGE_LOOP('',(#8369,#8370,#8371,#8372));
#2091=EDGE_LOOP('',(#8373,#8374,#8375,#8376));
#2092=EDGE_LOOP('',(#8377,#8378,#8379,#8380));
#2093=EDGE_LOOP('',(#8381,#8382,#8383,#8384));
#2094=EDGE_LOOP('',(#8385,#8386,#8387,#8388));
#2095=EDGE_LOOP('',(#8389,#8390,#8391,#8392));
#2096=EDGE_LOOP('',(#8393,#8394,#8395,#8396));
#2097=EDGE_LOOP('',(#8397,#8398,#8399,#8400));
#2098=EDGE_LOOP('',(#8401,#8402,#8403,#8404));
#2099=EDGE_LOOP('',(#8405,#8406,#8407,#8408));
#2100=EDGE_LOOP('',(#8409,#8410,#8411,#8412));
#2101=EDGE_LOOP('',(#8413,#8414,#8415,#8416));
#2102=EDGE_LOOP('',(#8417,#8418,#8419,#8420));
#2103=EDGE_LOOP('',(#8421,#8422,#8423,#8424));
#2104=EDGE_LOOP('',(#8425,#8426,#8427,#8428));
#2105=EDGE_LOOP('',(#8429,#8430,#8431,#8432));
#2106=EDGE_LOOP('',(#8433,#8434,#8435,#8436));
#2107=EDGE_LOOP('',(#8437,#8438,#8439,#8440));
#2108=EDGE_LOOP('',(#8441,#8442,#8443,#8444));
#2109=EDGE_LOOP('',(#8445,#8446,#8447,#8448));
#2110=EDGE_LOOP('',(#8449,#8450,#8451,#8452));
#2111=EDGE_LOOP('',(#8453,#8454,#8455,#8456));
#2112=EDGE_LOOP('',(#8457,#8458,#8459,#8460));
#2113=EDGE_LOOP('',(#8461,#8462,#8463,#8464));
#2114=EDGE_LOOP('',(#8465,#8466,#8467,#8468));
#2115=EDGE_LOOP('',(#8469,#8470,#8471,#8472));
#2116=EDGE_LOOP('',(#8473,#8474,#8475,#8476));
#2117=EDGE_LOOP('',(#8477,#8478,#8479,#8480));
#2118=EDGE_LOOP('',(#8481,#8482,#8483,#8484));
#2119=EDGE_LOOP('',(#8485,#8486,#8487,#8488));
#2120=EDGE_LOOP('',(#8489,#8490,#8491,#8492));
#2121=EDGE_LOOP('',(#8493,#8494,#8495,#8496));
#2122=EDGE_LOOP('',(#8497,#8498,#8499,#8500));
#2123=EDGE_LOOP('',(#8501,#8502,#8503,#8504));
#2124=EDGE_LOOP('',(#8505,#8506,#8507,#8508));
#2125=EDGE_LOOP('',(#8509,#8510,#8511,#8512));
#2126=EDGE_LOOP('',(#8513,#8514,#8515,#8516));
#2127=EDGE_LOOP('',(#8517,#8518,#8519,#8520));
#2128=EDGE_LOOP('',(#8521,#8522,#8523,#8524));
#2129=EDGE_LOOP('',(#8525,#8526,#8527,#8528));
#2130=EDGE_LOOP('',(#8529,#8530,#8531,#8532));
#2131=EDGE_LOOP('',(#8533,#8534,#8535,#8536));
#2132=EDGE_LOOP('',(#8537,#8538,#8539,#8540));
#2133=EDGE_LOOP('',(#8541,#8542,#8543,#8544));
#2134=EDGE_LOOP('',(#8545,#8546,#8547,#8548));
#2135=EDGE_LOOP('',(#8549,#8550,#8551,#8552));
#2136=EDGE_LOOP('',(#8553,#8554,#8555,#8556));
#2137=EDGE_LOOP('',(#8557,#8558,#8559,#8560));
#2138=EDGE_LOOP('',(#8561,#8562,#8563,#8564));
#2139=EDGE_LOOP('',(#8565,#8566,#8567,#8568));
#2140=EDGE_LOOP('',(#8569,#8570,#8571,#8572));
#2141=EDGE_LOOP('',(#8573,#8574,#8575,#8576));
#2142=EDGE_LOOP('',(#8577,#8578,#8579,#8580));
#2143=EDGE_LOOP('',(#8581,#8582,#8583,#8584));
#2144=EDGE_LOOP('',(#8585,#8586,#8587,#8588));
#2145=EDGE_LOOP('',(#8589,#8590,#8591,#8592));
#2146=EDGE_LOOP('',(#8593,#8594,#8595,#8596));
#2147=EDGE_LOOP('',(#8597,#8598,#8599,#8600));
#2148=EDGE_LOOP('',(#8601,#8602,#8603,#8604));
#2149=EDGE_LOOP('',(#8605,#8606,#8607,#8608));
#2150=EDGE_LOOP('',(#8609,#8610,#8611,#8612));
#2151=EDGE_LOOP('',(#8613,#8614,#8615,#8616));
#2152=EDGE_LOOP('',(#8617,#8618,#8619,#8620));
#2153=EDGE_LOOP('',(#8621,#8622,#8623,#8624));
#2154=EDGE_LOOP('',(#8625,#8626,#8627,#8628));
#2155=EDGE_LOOP('',(#8629,#8630,#8631,#8632));
#2156=EDGE_LOOP('',(#8633,#8634,#8635,#8636));
#2157=EDGE_LOOP('',(#8637,#8638,#8639,#8640));
#2158=EDGE_LOOP('',(#8641,#8642,#8643,#8644));
#2159=EDGE_LOOP('',(#8645,#8646,#8647,#8648));
#2160=EDGE_LOOP('',(#8649,#8650,#8651,#8652));
#2161=EDGE_LOOP('',(#8653,#8654,#8655,#8656));
#2162=EDGE_LOOP('',(#8657,#8658,#8659,#8660));
#2163=EDGE_LOOP('',(#8661,#8662,#8663,#8664));
#2164=EDGE_LOOP('',(#8665,#8666,#8667,#8668));
#2165=EDGE_LOOP('',(#8669,#8670,#8671,#8672));
#2166=EDGE_LOOP('',(#8673,#8674,#8675,#8676));
#2167=EDGE_LOOP('',(#8677,#8678,#8679,#8680));
#2168=EDGE_LOOP('',(#8681,#8682,#8683,#8684));
#2169=EDGE_LOOP('',(#8685,#8686,#8687,#8688));
#2170=EDGE_LOOP('',(#8689,#8690,#8691,#8692));
#2171=EDGE_LOOP('',(#8693,#8694,#8695,#8696));
#2172=EDGE_LOOP('',(#8697,#8698,#8699,#8700));
#2173=EDGE_LOOP('',(#8701,#8702,#8703,#8704));
#2174=EDGE_LOOP('',(#8705,#8706,#8707,#8708));
#2175=EDGE_LOOP('',(#8709,#8710,#8711,#8712));
#2176=EDGE_LOOP('',(#8713,#8714,#8715,#8716,#8717,#8718,#8719,#8720,#8721,
#8722,#8723,#8724,#8725,#8726,#8727,#8728,#8729,#8730,#8731,#8732,#8733,
#8734,#8735,#8736,#8737,#8738,#8739,#8740,#8741,#8742,#8743,#8744,#8745,
#8746,#8747,#8748,#8749,#8750,#8751,#8752,#8753,#8754,#8755,#8756,#8757,
#8758,#8759,#8760,#8761,#8762,#8763,#8764,#8765,#8766,#8767,#8768,#8769,
#8770,#8771,#8772,#8773,#8774,#8775,#8776,#8777,#8778,#8779,#8780,#8781,
#8782,#8783,#8784,#8785,#8786,#8787,#8788,#8789,#8790,#8791,#8792,#8793,
#8794,#8795,#8796,#8797,#8798,#8799,#8800,#8801,#8802,#8803,#8804,#8805,
#8806,#8807,#8808,#8809,#8810,#8811,#8812,#8813,#8814,#8815,#8816,#8817,
#8818,#8819,#8820,#8821,#8822,#8823,#8824,#8825,#8826,#8827,#8828,#8829,
#8830,#8831,#8832,#8833,#8834,#8835,#8836,#8837,#8838,#8839,#8840,#8841,
#8842,#8843,#8844,#8845,#8846,#8847,#8848,#8849,#8850,#8851,#8852,#8853,
#8854,#8855,#8856,#8857,#8858,#8859,#8860,#8861,#8862,#8863,#8864,#8865,
#8866,#8867,#8868,#8869,#8870,#8871,#8872));
#2177=EDGE_LOOP('',(#8873));
#2178=EDGE_LOOP('',(#8874,#8875,#8876,#8877,#8878,#8879,#8880,#8881,#8882,
#8883,#8884,#8885,#8886,#8887,#8888,#8889,#8890,#8891,#8892,#8893,#8894,
#8895,#8896,#8897,#8898,#8899,#8900,#8901,#8902,#8903,#8904,#8905,#8906,
#8907,#8908,#8909,#8910,#8911,#8912,#8913,#8914,#8915,#8916,#8917,#8918,
#8919,#8920,#8921,#8922,#8923,#8924,#8925,#8926,#8927,#8928,#8929,#8930,
#8931,#8932,#8933,#8934,#8935,#8936,#8937,#8938,#8939,#8940,#8941,#8942,
#8943,#8944,#8945,#8946,#8947,#8948,#8949,#8950,#8951,#8952,#8953,#8954,
#8955,#8956,#8957,#8958,#8959,#8960,#8961,#8962,#8963,#8964,#8965,#8966,
#8967,#8968,#8969,#8970,#8971,#8972,#8973,#8974,#8975,#8976,#8977,#8978,
#8979,#8980,#8981,#8982,#8983,#8984,#8985,#8986,#8987,#8988,#8989,#8990,
#8991,#8992,#8993,#8994,#8995,#8996,#8997,#8998,#8999,#9000,#9001,#9002,
#9003,#9004,#9005,#9006,#9007,#9008,#9009,#9010,#9011,#9012,#9013,#9014,
#9015,#9016,#9017,#9018,#9019,#9020,#9021,#9022,#9023,#9024,#9025,#9026,
#9027,#9028,#9029,#9030,#9031,#9032,#9033));
#2179=EDGE_LOOP('',(#9034));
#2180=EDGE_LOOP('',(#9035,#9036,#9037,#9038));
#2181=EDGE_LOOP('',(#9039,#9040,#9041,#9042));
#2182=EDGE_LOOP('',(#9043,#9044,#9045,#9046));
#2183=EDGE_LOOP('',(#9047,#9048,#9049,#9050));
#2184=EDGE_LOOP('',(#9051,#9052,#9053,#9054));
#2185=EDGE_LOOP('',(#9055,#9056,#9057,#9058));
#2186=EDGE_LOOP('',(#9059,#9060,#9061,#9062));
#2187=EDGE_LOOP('',(#9063,#9064,#9065,#9066));
#2188=EDGE_LOOP('',(#9067,#9068,#9069,#9070));
#2189=EDGE_LOOP('',(#9071,#9072,#9073,#9074));
#2190=EDGE_LOOP('',(#9075,#9076,#9077,#9078));
#2191=EDGE_LOOP('',(#9079,#9080,#9081,#9082));
#2192=EDGE_LOOP('',(#9083,#9084,#9085,#9086));
#2193=EDGE_LOOP('',(#9087,#9088,#9089,#9090));
#2194=EDGE_LOOP('',(#9091,#9092,#9093,#9094));
#2195=EDGE_LOOP('',(#9095,#9096,#9097,#9098));
#2196=EDGE_LOOP('',(#9099,#9100,#9101,#9102));
#2197=EDGE_LOOP('',(#9103,#9104,#9105,#9106));
#2198=EDGE_LOOP('',(#9107,#9108,#9109,#9110));
#2199=EDGE_LOOP('',(#9111,#9112,#9113,#9114));
#2200=EDGE_LOOP('',(#9115,#9116,#9117,#9118));
#2201=EDGE_LOOP('',(#9119,#9120,#9121,#9122));
#2202=EDGE_LOOP('',(#9123,#9124,#9125,#9126));
#2203=EDGE_LOOP('',(#9127,#9128,#9129,#9130));
#2204=EDGE_LOOP('',(#9131,#9132,#9133,#9134));
#2205=EDGE_LOOP('',(#9135,#9136,#9137,#9138));
#2206=EDGE_LOOP('',(#9139,#9140,#9141,#9142));
#2207=EDGE_LOOP('',(#9143,#9144,#9145,#9146));
#2208=EDGE_LOOP('',(#9147,#9148,#9149,#9150));
#2209=EDGE_LOOP('',(#9151));
#2210=EDGE_LOOP('',(#9152));
#2211=EDGE_LOOP('',(#9153,#9154,#9155,#9156));
#2212=EDGE_LOOP('',(#9157,#9158,#9159,#9160));
#2213=EDGE_LOOP('',(#9161,#9162,#9163,#9164));
#2214=EDGE_LOOP('',(#9165,#9166,#9167,#9168));
#2215=EDGE_LOOP('',(#9169,#9170,#9171,#9172));
#2216=EDGE_LOOP('',(#9173,#9174,#9175,#9176));
#2217=EDGE_LOOP('',(#9177,#9178,#9179,#9180));
#2218=EDGE_LOOP('',(#9181,#9182,#9183,#9184));
#2219=EDGE_LOOP('',(#9185,#9186,#9187,#9188));
#2220=EDGE_LOOP('',(#9189,#9190,#9191,#9192));
#2221=EDGE_LOOP('',(#9193,#9194,#9195,#9196));
#2222=EDGE_LOOP('',(#9197,#9198,#9199,#9200));
#2223=EDGE_LOOP('',(#9201,#9202,#9203,#9204));
#2224=EDGE_LOOP('',(#9205,#9206,#9207,#9208));
#2225=EDGE_LOOP('',(#9209,#9210,#9211,#9212));
#2226=EDGE_LOOP('',(#9213,#9214,#9215,#9216));
#2227=EDGE_LOOP('',(#9217,#9218,#9219,#9220));
#2228=EDGE_LOOP('',(#9221,#9222,#9223,#9224));
#2229=EDGE_LOOP('',(#9225,#9226,#9227,#9228));
#2230=EDGE_LOOP('',(#9229,#9230,#9231,#9232));
#2231=EDGE_LOOP('',(#9233,#9234,#9235,#9236));
#2232=EDGE_LOOP('',(#9237,#9238,#9239,#9240));
#2233=EDGE_LOOP('',(#9241,#9242,#9243,#9244));
#2234=EDGE_LOOP('',(#9245,#9246,#9247,#9248));
#2235=EDGE_LOOP('',(#9249,#9250,#9251,#9252));
#2236=EDGE_LOOP('',(#9253,#9254,#9255,#9256));
#2237=EDGE_LOOP('',(#9257,#9258,#9259,#9260));
#2238=EDGE_LOOP('',(#9261,#9262,#9263,#9264));
#2239=EDGE_LOOP('',(#9265,#9266,#9267,#9268));
#2240=EDGE_LOOP('',(#9269,#9270,#9271,#9272));
#2241=EDGE_LOOP('',(#9273,#9274,#9275,#9276));
#2242=EDGE_LOOP('',(#9277,#9278,#9279,#9280));
#2243=EDGE_LOOP('',(#9281,#9282,#9283,#9284));
#2244=EDGE_LOOP('',(#9285,#9286,#9287,#9288));
#2245=EDGE_LOOP('',(#9289,#9290,#9291,#9292));
#2246=EDGE_LOOP('',(#9293,#9294,#9295,#9296));
#2247=EDGE_LOOP('',(#9297,#9298,#9299,#9300));
#2248=EDGE_LOOP('',(#9301,#9302,#9303,#9304));
#2249=EDGE_LOOP('',(#9305,#9306,#9307,#9308));
#2250=EDGE_LOOP('',(#9309,#9310,#9311,#9312));
#2251=EDGE_LOOP('',(#9313,#9314,#9315,#9316));
#2252=EDGE_LOOP('',(#9317,#9318,#9319,#9320));
#2253=EDGE_LOOP('',(#9321,#9322,#9323,#9324));
#2254=EDGE_LOOP('',(#9325,#9326,#9327,#9328));
#2255=EDGE_LOOP('',(#9329,#9330,#9331,#9332));
#2256=EDGE_LOOP('',(#9333,#9334,#9335,#9336));
#2257=EDGE_LOOP('',(#9337,#9338,#9339,#9340));
#2258=EDGE_LOOP('',(#9341,#9342,#9343,#9344));
#2259=EDGE_LOOP('',(#9345,#9346,#9347,#9348));
#2260=EDGE_LOOP('',(#9349,#9350,#9351,#9352));
#2261=EDGE_LOOP('',(#9353,#9354,#9355,#9356));
#2262=EDGE_LOOP('',(#9357,#9358,#9359,#9360));
#2263=EDGE_LOOP('',(#9361,#9362,#9363,#9364));
#2264=EDGE_LOOP('',(#9365,#9366,#9367,#9368));
#2265=EDGE_LOOP('',(#9369,#9370,#9371,#9372));
#2266=EDGE_LOOP('',(#9373,#9374,#9375,#9376));
#2267=EDGE_LOOP('',(#9377,#9378,#9379,#9380));
#2268=EDGE_LOOP('',(#9381,#9382,#9383,#9384));
#2269=EDGE_LOOP('',(#9385,#9386,#9387,#9388));
#2270=EDGE_LOOP('',(#9389,#9390,#9391,#9392));
#2271=EDGE_LOOP('',(#9393,#9394,#9395,#9396));
#2272=EDGE_LOOP('',(#9397,#9398,#9399,#9400));
#2273=EDGE_LOOP('',(#9401,#9402,#9403,#9404));
#2274=EDGE_LOOP('',(#9405,#9406,#9407,#9408,#9409,#9410,#9411,#9412,#9413,
#9414,#9415,#9416,#9417,#9418,#9419,#9420,#9421,#9422,#9423,#9424,#9425,
#9426,#9427,#9428,#9429,#9430,#9431,#9432,#9433,#9434,#9435,#9436,#9437,
#9438,#9439,#9440,#9441,#9442,#9443,#9444,#9445,#9446,#9447,#9448,#9449,
#9450,#9451,#9452,#9453,#9454,#9455,#9456,#9457,#9458,#9459,#9460,#9461,
#9462,#9463,#9464,#9465,#9466,#9467,#9468,#9469,#9470,#9471,#9472,#9473,
#9474,#9475,#9476,#9477,#9478,#9479,#9480,#9481,#9482,#9483,#9484));
#2275=EDGE_LOOP('',(#9485));
#2276=EDGE_LOOP('',(#9486,#9487,#9488,#9489,#9490,#9491,#9492,#9493,#9494,
#9495,#9496,#9497,#9498,#9499,#9500,#9501,#9502,#9503,#9504,#9505,#9506,
#9507,#9508,#9509,#9510,#9511,#9512,#9513,#9514,#9515,#9516,#9517,#9518,
#9519,#9520,#9521,#9522,#9523,#9524,#9525,#9526,#9527,#9528,#9529,#9530,
#9531,#9532,#9533,#9534,#9535,#9536,#9537,#9538,#9539,#9540,#9541,#9542,
#9543,#9544,#9545,#9546,#9547,#9548,#9549,#9550,#9551,#9552,#9553,#9554,
#9555,#9556,#9557,#9558,#9559,#9560,#9561,#9562,#9563,#9564,#9565));
#2277=EDGE_LOOP('',(#9566));
#2278=EDGE_LOOP('',(#9567,#9568,#9569,#9570));
#2279=EDGE_LOOP('',(#9571,#9572,#9573,#9574));
#2280=EDGE_LOOP('',(#9575,#9576,#9577,#9578));
#2281=EDGE_LOOP('',(#9579,#9580,#9581,#9582));
#2282=EDGE_LOOP('',(#9583,#9584,#9585,#9586));
#2283=EDGE_LOOP('',(#9587,#9588,#9589,#9590));
#2284=EDGE_LOOP('',(#9591,#9592,#9593,#9594));
#2285=EDGE_LOOP('',(#9595,#9596,#9597,#9598));
#2286=EDGE_LOOP('',(#9599,#9600,#9601,#9602));
#2287=EDGE_LOOP('',(#9603,#9604,#9605,#9606));
#2288=EDGE_LOOP('',(#9607,#9608,#9609,#9610));
#2289=EDGE_LOOP('',(#9611,#9612,#9613,#9614));
#2290=EDGE_LOOP('',(#9615,#9616,#9617,#9618));
#2291=EDGE_LOOP('',(#9619,#9620,#9621,#9622));
#2292=EDGE_LOOP('',(#9623,#9624,#9625,#9626));
#2293=EDGE_LOOP('',(#9627,#9628,#9629,#9630));
#2294=EDGE_LOOP('',(#9631,#9632,#9633,#9634));
#2295=EDGE_LOOP('',(#9635,#9636,#9637,#9638));
#2296=EDGE_LOOP('',(#9639,#9640,#9641,#9642,#9643,#9644));
#2297=EDGE_LOOP('',(#9645,#9646,#9647,#9648,#9649));
#2298=EDGE_LOOP('',(#9650,#9651,#9652,#9653,#9654));
#2299=EDGE_LOOP('',(#9655,#9656,#9657,#9658,#9659,#9660));
#2300=EDGE_LOOP('',(#9661,#9662,#9663,#9664));
#2301=EDGE_LOOP('',(#9665,#9666,#9667,#9668));
#2302=EDGE_LOOP('',(#9669,#9670,#9671,#9672));
#2303=EDGE_LOOP('',(#9673));
#2304=EDGE_LOOP('',(#9674));
#2305=EDGE_LOOP('',(#9675));
#2306=EDGE_LOOP('',(#9676));
#2307=EDGE_LOOP('',(#9677,#9678));
#2308=EDGE_LOOP('',(#9679,#9680));
#2309=EDGE_LOOP('',(#9681,#9682));
#2310=EDGE_LOOP('',(#9683,#9684));
#2311=EDGE_LOOP('',(#9685,#9686));
#2312=EDGE_LOOP('',(#9687,#9688));
#2313=EDGE_LOOP('',(#9689,#9690));
#2314=EDGE_LOOP('',(#9691,#9692,#9693,#9694,#9695));
#2315=EDGE_LOOP('',(#9696,#9697,#9698,#9699));
#2316=EDGE_LOOP('',(#9700,#9701,#9702,#9703));
#2317=EDGE_LOOP('',(#9704,#9705,#9706,#9707,#9708));
#2318=EDGE_LOOP('',(#9709,#9710,#9711,#9712));
#2319=EDGE_LOOP('',(#9713,#9714,#9715,#9716,#9717));
#2320=EDGE_LOOP('',(#9718,#9719,#9720,#9721,#9722));
#2321=EDGE_LOOP('',(#9723,#9724,#9725,#9726));
#2322=EDGE_LOOP('',(#9727,#9728,#9729,#9730));
#2323=EDGE_LOOP('',(#9731,#9732,#9733,#9734));
#2324=EDGE_LOOP('',(#9735,#9736,#9737,#9738));
#2325=EDGE_LOOP('',(#9739,#9740,#9741,#9742));
#2326=EDGE_LOOP('',(#9743,#9744,#9745,#9746,#9747));
#2327=EDGE_LOOP('',(#9748,#9749,#9750,#9751,#9752));
#2328=EDGE_LOOP('',(#9753));
#2329=EDGE_LOOP('',(#9754));
#2330=EDGE_LOOP('',(#9755));
#2331=EDGE_LOOP('',(#9756));
#2332=EDGE_LOOP('',(#9757));
#2333=EDGE_LOOP('',(#9758));
#2334=EDGE_LOOP('',(#9759));
#2335=EDGE_LOOP('',(#9760));
#2336=EDGE_LOOP('',(#9761));
#2337=EDGE_LOOP('',(#9762));
#2338=EDGE_LOOP('',(#9763));
#2339=EDGE_LOOP('',(#9764));
#2340=EDGE_LOOP('',(#9765,#9766,#9767,#9768));
#2341=EDGE_LOOP('',(#9769,#9770,#9771,#9772));
#2342=EDGE_LOOP('',(#9773,#9774,#9775,#9776));
#2343=EDGE_LOOP('',(#9777,#9778,#9779,#9780,#9781,#9782,#9783,#9784,#9785,
#9786,#9787,#9788));
#2344=EDGE_LOOP('',(#9789));
#2345=EDGE_LOOP('',(#9790));
#2346=EDGE_LOOP('',(#9791,#9792,#9793,#9794));
#2347=EDGE_LOOP('',(#9795,#9796,#9797,#9798));
#2348=EDGE_LOOP('',(#9799,#9800,#9801,#9802));
#2349=EDGE_LOOP('',(#9803,#9804,#9805,#9806,#9807,#9808,#9809,#9810,#9811,
#9812,#9813,#9814));
#2350=EDGE_LOOP('',(#9815));
#2351=EDGE_LOOP('',(#9816));
#2352=EDGE_LOOP('',(#9817,#9818,#9819,#9820));
#2353=EDGE_LOOP('',(#9821,#9822,#9823,#9824));
#2354=EDGE_LOOP('',(#9825,#9826,#9827,#9828));
#2355=EDGE_LOOP('',(#9829,#9830,#9831,#9832,#9833,#9834,#9835,#9836,#9837,
#9838,#9839,#9840));
#2356=EDGE_LOOP('',(#9841));
#2357=EDGE_LOOP('',(#9842));
#2358=EDGE_LOOP('',(#9843,#9844,#9845,#9846));
#2359=EDGE_LOOP('',(#9847,#9848,#9849,#9850));
#2360=EDGE_LOOP('',(#9851,#9852,#9853,#9854));
#2361=EDGE_LOOP('',(#9855,#9856,#9857,#9858,#9859,#9860,#9861,#9862,#9863,
#9864,#9865,#9866));
#2362=EDGE_LOOP('',(#9867));
#2363=EDGE_LOOP('',(#9868));
#2364=EDGE_LOOP('',(#9869,#9870,#9871,#9872));
#2365=EDGE_LOOP('',(#9873,#9874,#9875,#9876));
#2366=EDGE_LOOP('',(#9877,#9878,#9879,#9880));
#2367=EDGE_LOOP('',(#9881,#9882,#9883,#9884,#9885,#9886,#9887,#9888,#9889,
#9890,#9891,#9892));
#2368=EDGE_LOOP('',(#9893));
#2369=EDGE_LOOP('',(#9894));
#2370=EDGE_LOOP('',(#9895,#9896,#9897,#9898));
#2371=EDGE_LOOP('',(#9899,#9900,#9901,#9902));
#2372=EDGE_LOOP('',(#9903,#9904,#9905,#9906));
#2373=EDGE_LOOP('',(#9907,#9908,#9909,#9910,#9911,#9912,#9913,#9914,#9915,
#9916,#9917,#9918));
#2374=EDGE_LOOP('',(#9919));
#2375=EDGE_LOOP('',(#9920));
#2376=EDGE_LOOP('',(#9921,#9922,#9923,#9924,#9925,#9926,#9927,#9928,#9929,
#9930,#9931,#9932));
#2377=EDGE_LOOP('',(#9933));
#2378=EDGE_LOOP('',(#9934));
#2379=EDGE_LOOP('',(#9935,#9936,#9937,#9938));
#2380=EDGE_LOOP('',(#9939,#9940,#9941,#9942));
#2381=EDGE_LOOP('',(#9943,#9944,#9945,#9946));
#2382=EDGE_LOOP('',(#9947,#9948,#9949,#9950));
#2383=EDGE_LOOP('',(#9951,#9952,#9953,#9954));
#2384=EDGE_LOOP('',(#9955,#9956,#9957,#9958));
#2385=EDGE_LOOP('',(#9959,#9960,#9961,#9962));
#2386=EDGE_LOOP('',(#9963));
#2387=EDGE_LOOP('',(#9964));
#2388=EDGE_LOOP('',(#9965));
#2389=EDGE_LOOP('',(#9966));
#2390=EDGE_LOOP('',(#9967,#9968,#9969,#9970));
#2391=EDGE_LOOP('',(#9971,#9972,#9973,#9974,#9975,#9976));
#2392=EDGE_LOOP('',(#9977,#9978,#9979,#9980));
#2393=EDGE_LOOP('',(#9981,#9982,#9983,#9984));
#2394=EDGE_LOOP('',(#9985));
#2395=EDGE_LOOP('',(#9986));
#2396=EDGE_LOOP('',(#9987));
#2397=EDGE_LOOP('',(#9988));
#2398=EDGE_LOOP('',(#9989,#9990,#9991,#9992));
#2399=EDGE_LOOP('',(#9993,#9994,#9995,#9996));
#2400=EDGE_LOOP('',(#9997,#9998,#9999,#10000));
#2401=EDGE_LOOP('',(#10001,#10002,#10003,#10004));
#2402=EDGE_LOOP('',(#10005,#10006,#10007,#10008));
#2403=EDGE_LOOP('',(#10009,#10010,#10011,#10012));
#2404=EDGE_LOOP('',(#10013,#10014,#10015,#10016,#10017,#10018));
#2405=EDGE_LOOP('',(#10019,#10020,#10021,#10022));
#2406=EDGE_LOOP('',(#10023));
#2407=EDGE_LOOP('',(#10024));
#2408=EDGE_LOOP('',(#10025));
#2409=EDGE_LOOP('',(#10026));
#2410=EDGE_LOOP('',(#10027,#10028,#10029,#10030));
#2411=EDGE_LOOP('',(#10031,#10032,#10033,#10034));
#2412=EDGE_LOOP('',(#10035,#10036,#10037,#10038));
#2413=EDGE_LOOP('',(#10039,#10040,#10041,#10042));
#2414=EDGE_LOOP('',(#10043,#10044,#10045,#10046));
#2415=EDGE_LOOP('',(#10047,#10048,#10049,#10050));
#2416=EDGE_LOOP('',(#10051,#10052,#10053,#10054,#10055,#10056));
#2417=EDGE_LOOP('',(#10057,#10058,#10059,#10060));
#2418=EDGE_LOOP('',(#10061));
#2419=EDGE_LOOP('',(#10062));
#2420=EDGE_LOOP('',(#10063));
#2421=EDGE_LOOP('',(#10064));
#2422=EDGE_LOOP('',(#10065,#10066,#10067,#10068));
#2423=EDGE_LOOP('',(#10069,#10070,#10071,#10072));
#2424=EDGE_LOOP('',(#10073,#10074,#10075,#10076));
#2425=EDGE_LOOP('',(#10077,#10078,#10079,#10080));
#2426=EDGE_LOOP('',(#10081,#10082,#10083,#10084));
#2427=EDGE_LOOP('',(#10085,#10086,#10087,#10088));
#2428=EDGE_LOOP('',(#10089,#10090,#10091,#10092,#10093,#10094));
#2429=EDGE_LOOP('',(#10095,#10096,#10097,#10098));
#2430=EDGE_LOOP('',(#10099));
#2431=EDGE_LOOP('',(#10100));
#2432=EDGE_LOOP('',(#10101));
#2433=EDGE_LOOP('',(#10102));
#2434=EDGE_LOOP('',(#10103,#10104,#10105,#10106));
#2435=EDGE_LOOP('',(#10107,#10108,#10109,#10110));
#2436=EDGE_LOOP('',(#10111,#10112,#10113,#10114));
#2437=EDGE_LOOP('',(#10115,#10116,#10117,#10118));
#2438=EDGE_LOOP('',(#10119,#10120,#10121,#10122));
#2439=EDGE_LOOP('',(#10123,#10124,#10125,#10126));
#2440=EDGE_LOOP('',(#10127,#10128,#10129,#10130,#10131,#10132));
#2441=EDGE_LOOP('',(#10133,#10134,#10135,#10136));
#2442=EDGE_LOOP('',(#10137));
#2443=EDGE_LOOP('',(#10138));
#2444=EDGE_LOOP('',(#10139));
#2445=EDGE_LOOP('',(#10140));
#2446=EDGE_LOOP('',(#10141,#10142,#10143,#10144));
#2447=EDGE_LOOP('',(#10145,#10146,#10147,#10148));
#2448=EDGE_LOOP('',(#10149,#10150,#10151,#10152));
#2449=EDGE_LOOP('',(#10153,#10154,#10155,#10156));
#2450=EDGE_LOOP('',(#10157,#10158,#10159,#10160));
#2451=EDGE_LOOP('',(#10161,#10162,#10163,#10164));
#2452=EDGE_LOOP('',(#10165,#10166,#10167,#10168,#10169,#10170));
#2453=EDGE_LOOP('',(#10171,#10172,#10173,#10174));
#2454=EDGE_LOOP('',(#10175));
#2455=EDGE_LOOP('',(#10176));
#2456=EDGE_LOOP('',(#10177));
#2457=EDGE_LOOP('',(#10178));
#2458=EDGE_LOOP('',(#10179,#10180,#10181,#10182));
#2459=EDGE_LOOP('',(#10183,#10184,#10185,#10186));
#2460=EDGE_LOOP('',(#10187,#10188,#10189,#10190));
#2461=EDGE_LOOP('',(#10191,#10192,#10193,#10194));
#2462=EDGE_LOOP('',(#10195,#10196,#10197,#10198));
#2463=EDGE_LOOP('',(#10199,#10200,#10201,#10202,#10203,#10204));
#2464=EDGE_LOOP('',(#10205,#10206,#10207,#10208));
#2465=EDGE_LOOP('',(#10209,#10210,#10211,#10212));
#2466=EDGE_LOOP('',(#10213,#10214,#10215,#10216));
#2467=EDGE_LOOP('',(#10217,#10218,#10219,#10220,#10221,#10222));
#2468=EDGE_LOOP('',(#10223,#10224,#10225,#10226,#10227));
#2469=EDGE_LOOP('',(#10228,#10229,#10230,#10231,#10232));
#2470=EDGE_LOOP('',(#10233,#10234,#10235,#10236,#10237,#10238));
#2471=EDGE_LOOP('',(#10239,#10240,#10241,#10242));
#2472=EDGE_LOOP('',(#10243,#10244,#10245,#10246));
#2473=EDGE_LOOP('',(#10247,#10248,#10249,#10250));
#2474=EDGE_LOOP('',(#10251));
#2475=EDGE_LOOP('',(#10252));
#2476=EDGE_LOOP('',(#10253));
#2477=EDGE_LOOP('',(#10254));
#2478=EDGE_LOOP('',(#10255,#10256));
#2479=EDGE_LOOP('',(#10257,#10258));
#2480=EDGE_LOOP('',(#10259,#10260));
#2481=EDGE_LOOP('',(#10261,#10262));
#2482=EDGE_LOOP('',(#10263,#10264));
#2483=EDGE_LOOP('',(#10265,#10266));
#2484=EDGE_LOOP('',(#10267,#10268));
#2485=EDGE_LOOP('',(#10269,#10270,#10271,#10272,#10273));
#2486=EDGE_LOOP('',(#10274,#10275,#10276,#10277));
#2487=EDGE_LOOP('',(#10278,#10279,#10280,#10281));
#2488=EDGE_LOOP('',(#10282,#10283,#10284,#10285,#10286));
#2489=EDGE_LOOP('',(#10287,#10288,#10289,#10290));
#2490=EDGE_LOOP('',(#10291,#10292,#10293,#10294,#10295));
#2491=EDGE_LOOP('',(#10296,#10297,#10298,#10299,#10300));
#2492=EDGE_LOOP('',(#10301,#10302,#10303,#10304));
#2493=EDGE_LOOP('',(#10305,#10306,#10307,#10308));
#2494=EDGE_LOOP('',(#10309,#10310,#10311,#10312));
#2495=EDGE_LOOP('',(#10313,#10314,#10315,#10316));
#2496=EDGE_LOOP('',(#10317,#10318,#10319,#10320));
#2497=EDGE_LOOP('',(#10321,#10322,#10323,#10324,#10325));
#2498=EDGE_LOOP('',(#10326,#10327,#10328,#10329,#10330));
#2499=EDGE_LOOP('',(#10331));
#2500=EDGE_LOOP('',(#10332));
#2501=EDGE_LOOP('',(#10333));
#2502=EDGE_LOOP('',(#10334));
#2503=EDGE_LOOP('',(#10335));
#2504=EDGE_LOOP('',(#10336));
#2505=EDGE_LOOP('',(#10337));
#2506=EDGE_LOOP('',(#10338));
#2507=EDGE_LOOP('',(#10339));
#2508=EDGE_LOOP('',(#10340));
#2509=EDGE_LOOP('',(#10341));
#2510=EDGE_LOOP('',(#10342));
#2511=EDGE_LOOP('',(#10343,#10344,#10345,#10346));
#2512=EDGE_LOOP('',(#10347,#10348,#10349,#10350));
#2513=EDGE_LOOP('',(#10351,#10352,#10353,#10354));
#2514=EDGE_LOOP('',(#10355,#10356,#10357,#10358,#10359,#10360,#10361,#10362,
#10363,#10364,#10365,#10366));
#2515=EDGE_LOOP('',(#10367));
#2516=EDGE_LOOP('',(#10368));
#2517=EDGE_LOOP('',(#10369,#10370,#10371,#10372));
#2518=EDGE_LOOP('',(#10373,#10374,#10375,#10376));
#2519=EDGE_LOOP('',(#10377,#10378,#10379,#10380));
#2520=EDGE_LOOP('',(#10381,#10382,#10383,#10384,#10385,#10386,#10387,#10388,
#10389,#10390,#10391,#10392));
#2521=EDGE_LOOP('',(#10393));
#2522=EDGE_LOOP('',(#10394));
#2523=EDGE_LOOP('',(#10395,#10396,#10397,#10398));
#2524=EDGE_LOOP('',(#10399,#10400,#10401,#10402));
#2525=EDGE_LOOP('',(#10403,#10404,#10405,#10406));
#2526=EDGE_LOOP('',(#10407,#10408,#10409,#10410,#10411,#10412,#10413,#10414,
#10415,#10416,#10417,#10418));
#2527=EDGE_LOOP('',(#10419));
#2528=EDGE_LOOP('',(#10420));
#2529=EDGE_LOOP('',(#10421,#10422,#10423,#10424));
#2530=EDGE_LOOP('',(#10425,#10426,#10427,#10428));
#2531=EDGE_LOOP('',(#10429,#10430,#10431,#10432));
#2532=EDGE_LOOP('',(#10433,#10434,#10435,#10436,#10437,#10438,#10439,#10440,
#10441,#10442,#10443,#10444));
#2533=EDGE_LOOP('',(#10445));
#2534=EDGE_LOOP('',(#10446));
#2535=EDGE_LOOP('',(#10447,#10448,#10449,#10450));
#2536=EDGE_LOOP('',(#10451,#10452,#10453,#10454));
#2537=EDGE_LOOP('',(#10455,#10456,#10457,#10458));
#2538=EDGE_LOOP('',(#10459,#10460,#10461,#10462,#10463,#10464,#10465,#10466,
#10467,#10468,#10469,#10470));
#2539=EDGE_LOOP('',(#10471));
#2540=EDGE_LOOP('',(#10472));
#2541=EDGE_LOOP('',(#10473,#10474,#10475,#10476));
#2542=EDGE_LOOP('',(#10477,#10478,#10479,#10480));
#2543=EDGE_LOOP('',(#10481,#10482,#10483,#10484));
#2544=EDGE_LOOP('',(#10485,#10486,#10487,#10488,#10489,#10490,#10491,#10492,
#10493,#10494,#10495,#10496));
#2545=EDGE_LOOP('',(#10497));
#2546=EDGE_LOOP('',(#10498));
#2547=EDGE_LOOP('',(#10499,#10500,#10501,#10502,#10503,#10504,#10505,#10506,
#10507,#10508,#10509,#10510));
#2548=EDGE_LOOP('',(#10511));
#2549=EDGE_LOOP('',(#10512));
#2550=EDGE_LOOP('',(#10513,#10514,#10515,#10516));
#2551=EDGE_LOOP('',(#10517,#10518,#10519,#10520));
#2552=EDGE_LOOP('',(#10521,#10522,#10523,#10524));
#2553=EDGE_LOOP('',(#10525,#10526,#10527,#10528));
#2554=EDGE_LOOP('',(#10529,#10530,#10531,#10532));
#2555=EDGE_LOOP('',(#10533,#10534,#10535,#10536));
#2556=EDGE_LOOP('',(#10537,#10538,#10539,#10540));
#2557=EDGE_LOOP('',(#10541));
#2558=EDGE_LOOP('',(#10542));
#2559=EDGE_LOOP('',(#10543));
#2560=EDGE_LOOP('',(#10544));
#2561=EDGE_LOOP('',(#10545,#10546,#10547,#10548));
#2562=EDGE_LOOP('',(#10549,#10550,#10551,#10552,#10553,#10554));
#2563=EDGE_LOOP('',(#10555,#10556,#10557,#10558));
#2564=EDGE_LOOP('',(#10559,#10560,#10561,#10562));
#2565=EDGE_LOOP('',(#10563));
#2566=EDGE_LOOP('',(#10564));
#2567=EDGE_LOOP('',(#10565));
#2568=EDGE_LOOP('',(#10566));
#2569=EDGE_LOOP('',(#10567,#10568,#10569,#10570));
#2570=EDGE_LOOP('',(#10571,#10572,#10573,#10574));
#2571=EDGE_LOOP('',(#10575,#10576,#10577,#10578));
#2572=EDGE_LOOP('',(#10579,#10580,#10581,#10582));
#2573=EDGE_LOOP('',(#10583,#10584,#10585,#10586));
#2574=EDGE_LOOP('',(#10587,#10588,#10589,#10590));
#2575=EDGE_LOOP('',(#10591,#10592,#10593,#10594,#10595,#10596));
#2576=EDGE_LOOP('',(#10597,#10598,#10599,#10600));
#2577=EDGE_LOOP('',(#10601));
#2578=EDGE_LOOP('',(#10602));
#2579=EDGE_LOOP('',(#10603));
#2580=EDGE_LOOP('',(#10604));
#2581=EDGE_LOOP('',(#10605,#10606,#10607,#10608));
#2582=EDGE_LOOP('',(#10609,#10610,#10611,#10612));
#2583=EDGE_LOOP('',(#10613,#10614,#10615,#10616));
#2584=EDGE_LOOP('',(#10617,#10618,#10619,#10620));
#2585=EDGE_LOOP('',(#10621,#10622,#10623,#10624));
#2586=EDGE_LOOP('',(#10625,#10626,#10627,#10628));
#2587=EDGE_LOOP('',(#10629,#10630,#10631,#10632,#10633,#10634));
#2588=EDGE_LOOP('',(#10635,#10636,#10637,#10638));
#2589=EDGE_LOOP('',(#10639));
#2590=EDGE_LOOP('',(#10640));
#2591=EDGE_LOOP('',(#10641));
#2592=EDGE_LOOP('',(#10642));
#2593=EDGE_LOOP('',(#10643,#10644,#10645,#10646));
#2594=EDGE_LOOP('',(#10647,#10648,#10649,#10650));
#2595=EDGE_LOOP('',(#10651,#10652,#10653,#10654));
#2596=EDGE_LOOP('',(#10655,#10656,#10657,#10658));
#2597=EDGE_LOOP('',(#10659,#10660,#10661,#10662));
#2598=EDGE_LOOP('',(#10663,#10664,#10665,#10666));
#2599=EDGE_LOOP('',(#10667,#10668,#10669,#10670,#10671,#10672));
#2600=EDGE_LOOP('',(#10673,#10674,#10675,#10676));
#2601=EDGE_LOOP('',(#10677));
#2602=EDGE_LOOP('',(#10678));
#2603=EDGE_LOOP('',(#10679));
#2604=EDGE_LOOP('',(#10680));
#2605=EDGE_LOOP('',(#10681,#10682,#10683,#10684));
#2606=EDGE_LOOP('',(#10685,#10686,#10687,#10688));
#2607=EDGE_LOOP('',(#10689,#10690,#10691,#10692));
#2608=EDGE_LOOP('',(#10693,#10694,#10695,#10696));
#2609=EDGE_LOOP('',(#10697,#10698,#10699,#10700));
#2610=EDGE_LOOP('',(#10701,#10702,#10703,#10704));
#2611=EDGE_LOOP('',(#10705,#10706,#10707,#10708,#10709,#10710));
#2612=EDGE_LOOP('',(#10711,#10712,#10713,#10714));
#2613=EDGE_LOOP('',(#10715));
#2614=EDGE_LOOP('',(#10716));
#2615=EDGE_LOOP('',(#10717));
#2616=EDGE_LOOP('',(#10718));
#2617=EDGE_LOOP('',(#10719,#10720,#10721,#10722));
#2618=EDGE_LOOP('',(#10723,#10724,#10725,#10726));
#2619=EDGE_LOOP('',(#10727,#10728,#10729,#10730));
#2620=EDGE_LOOP('',(#10731,#10732,#10733,#10734));
#2621=EDGE_LOOP('',(#10735,#10736,#10737,#10738));
#2622=EDGE_LOOP('',(#10739,#10740,#10741,#10742));
#2623=EDGE_LOOP('',(#10743,#10744,#10745,#10746,#10747,#10748));
#2624=EDGE_LOOP('',(#10749,#10750,#10751,#10752));
#2625=EDGE_LOOP('',(#10753));
#2626=EDGE_LOOP('',(#10754));
#2627=EDGE_LOOP('',(#10755));
#2628=EDGE_LOOP('',(#10756));
#2629=EDGE_LOOP('',(#10757,#10758,#10759,#10760));
#2630=EDGE_LOOP('',(#10761,#10762,#10763,#10764));
#2631=EDGE_LOOP('',(#10765,#10766,#10767,#10768));
#2632=EDGE_LOOP('',(#10769,#10770,#10771,#10772));
#2633=EDGE_LOOP('',(#10773,#10774,#10775,#10776));
#2634=EDGE_LOOP('',(#10777,#10778,#10779,#10780,#10781,#10782));
#2635=EDGE_LOOP('',(#10783,#10784,#10785,#10786));
#2636=EDGE_LOOP('',(#10787,#10788,#10789,#10790));
#2637=EDGE_LOOP('',(#10791,#10792,#10793,#10794));
#2638=EDGE_LOOP('',(#10795,#10796,#10797,#10798,#10799,#10800));
#2639=EDGE_LOOP('',(#10801,#10802,#10803,#10804,#10805));
#2640=EDGE_LOOP('',(#10806,#10807,#10808,#10809,#10810));
#2641=EDGE_LOOP('',(#10811,#10812,#10813,#10814,#10815,#10816));
#2642=EDGE_LOOP('',(#10817,#10818,#10819,#10820));
#2643=EDGE_LOOP('',(#10821,#10822,#10823,#10824));
#2644=EDGE_LOOP('',(#10825,#10826,#10827,#10828));
#2645=EDGE_LOOP('',(#10829));
#2646=EDGE_LOOP('',(#10830));
#2647=EDGE_LOOP('',(#10831));
#2648=EDGE_LOOP('',(#10832));
#2649=EDGE_LOOP('',(#10833,#10834));
#2650=EDGE_LOOP('',(#10835,#10836));
#2651=EDGE_LOOP('',(#10837,#10838));
#2652=EDGE_LOOP('',(#10839,#10840));
#2653=EDGE_LOOP('',(#10841,#10842));
#2654=EDGE_LOOP('',(#10843,#10844));
#2655=EDGE_LOOP('',(#10845,#10846));
#2656=EDGE_LOOP('',(#10847,#10848,#10849,#10850,#10851));
#2657=EDGE_LOOP('',(#10852,#10853,#10854,#10855));
#2658=EDGE_LOOP('',(#10856,#10857,#10858,#10859));
#2659=EDGE_LOOP('',(#10860,#10861,#10862,#10863,#10864));
#2660=EDGE_LOOP('',(#10865,#10866,#10867,#10868));
#2661=EDGE_LOOP('',(#10869,#10870,#10871,#10872,#10873));
#2662=EDGE_LOOP('',(#10874,#10875,#10876,#10877,#10878));
#2663=EDGE_LOOP('',(#10879,#10880,#10881,#10882));
#2664=EDGE_LOOP('',(#10883,#10884,#10885,#10886));
#2665=EDGE_LOOP('',(#10887,#10888,#10889,#10890));
#2666=EDGE_LOOP('',(#10891,#10892,#10893,#10894));
#2667=EDGE_LOOP('',(#10895,#10896,#10897,#10898));
#2668=EDGE_LOOP('',(#10899,#10900,#10901,#10902,#10903));
#2669=EDGE_LOOP('',(#10904,#10905,#10906,#10907,#10908));
#2670=EDGE_LOOP('',(#10909));
#2671=EDGE_LOOP('',(#10910));
#2672=EDGE_LOOP('',(#10911));
#2673=EDGE_LOOP('',(#10912));
#2674=EDGE_LOOP('',(#10913));
#2675=EDGE_LOOP('',(#10914));
#2676=EDGE_LOOP('',(#10915));
#2677=EDGE_LOOP('',(#10916));
#2678=EDGE_LOOP('',(#10917));
#2679=EDGE_LOOP('',(#10918));
#2680=EDGE_LOOP('',(#10919));
#2681=EDGE_LOOP('',(#10920));
#2682=EDGE_LOOP('',(#10921,#10922,#10923,#10924));
#2683=EDGE_LOOP('',(#10925,#10926,#10927,#10928));
#2684=EDGE_LOOP('',(#10929,#10930,#10931,#10932));
#2685=EDGE_LOOP('',(#10933,#10934,#10935,#10936,#10937,#10938,#10939,#10940,
#10941,#10942,#10943,#10944));
#2686=EDGE_LOOP('',(#10945));
#2687=EDGE_LOOP('',(#10946));
#2688=EDGE_LOOP('',(#10947,#10948,#10949,#10950));
#2689=EDGE_LOOP('',(#10951,#10952,#10953,#10954));
#2690=EDGE_LOOP('',(#10955,#10956,#10957,#10958));
#2691=EDGE_LOOP('',(#10959,#10960,#10961,#10962,#10963,#10964,#10965,#10966,
#10967,#10968,#10969,#10970));
#2692=EDGE_LOOP('',(#10971));
#2693=EDGE_LOOP('',(#10972));
#2694=EDGE_LOOP('',(#10973,#10974,#10975,#10976));
#2695=EDGE_LOOP('',(#10977,#10978,#10979,#10980));
#2696=EDGE_LOOP('',(#10981,#10982,#10983,#10984));
#2697=EDGE_LOOP('',(#10985,#10986,#10987,#10988,#10989,#10990,#10991,#10992,
#10993,#10994,#10995,#10996));
#2698=EDGE_LOOP('',(#10997));
#2699=EDGE_LOOP('',(#10998));
#2700=EDGE_LOOP('',(#10999,#11000,#11001,#11002));
#2701=EDGE_LOOP('',(#11003,#11004,#11005,#11006));
#2702=EDGE_LOOP('',(#11007,#11008,#11009,#11010));
#2703=EDGE_LOOP('',(#11011,#11012,#11013,#11014,#11015,#11016,#11017,#11018,
#11019,#11020,#11021,#11022));
#2704=EDGE_LOOP('',(#11023));
#2705=EDGE_LOOP('',(#11024));
#2706=EDGE_LOOP('',(#11025,#11026,#11027,#11028));
#2707=EDGE_LOOP('',(#11029,#11030,#11031,#11032));
#2708=EDGE_LOOP('',(#11033,#11034,#11035,#11036));
#2709=EDGE_LOOP('',(#11037,#11038,#11039,#11040,#11041,#11042,#11043,#11044,
#11045,#11046,#11047,#11048));
#2710=EDGE_LOOP('',(#11049));
#2711=EDGE_LOOP('',(#11050));
#2712=EDGE_LOOP('',(#11051,#11052,#11053,#11054));
#2713=EDGE_LOOP('',(#11055,#11056,#11057,#11058));
#2714=EDGE_LOOP('',(#11059,#11060,#11061,#11062));
#2715=EDGE_LOOP('',(#11063,#11064,#11065,#11066,#11067,#11068,#11069,#11070,
#11071,#11072,#11073,#11074));
#2716=EDGE_LOOP('',(#11075));
#2717=EDGE_LOOP('',(#11076));
#2718=EDGE_LOOP('',(#11077,#11078,#11079,#11080,#11081,#11082,#11083,#11084,
#11085,#11086,#11087,#11088));
#2719=EDGE_LOOP('',(#11089));
#2720=EDGE_LOOP('',(#11090));
#2721=EDGE_LOOP('',(#11091,#11092,#11093,#11094));
#2722=EDGE_LOOP('',(#11095,#11096,#11097,#11098));
#2723=EDGE_LOOP('',(#11099,#11100,#11101,#11102));
#2724=EDGE_LOOP('',(#11103,#11104,#11105,#11106));
#2725=EDGE_LOOP('',(#11107,#11108,#11109,#11110));
#2726=EDGE_LOOP('',(#11111,#11112,#11113,#11114));
#2727=EDGE_LOOP('',(#11115,#11116,#11117,#11118));
#2728=EDGE_LOOP('',(#11119));
#2729=EDGE_LOOP('',(#11120));
#2730=EDGE_LOOP('',(#11121));
#2731=EDGE_LOOP('',(#11122));
#2732=EDGE_LOOP('',(#11123,#11124,#11125,#11126));
#2733=EDGE_LOOP('',(#11127,#11128,#11129,#11130,#11131,#11132));
#2734=EDGE_LOOP('',(#11133,#11134,#11135,#11136));
#2735=EDGE_LOOP('',(#11137,#11138,#11139,#11140));
#2736=EDGE_LOOP('',(#11141));
#2737=EDGE_LOOP('',(#11142));
#2738=EDGE_LOOP('',(#11143));
#2739=EDGE_LOOP('',(#11144));
#2740=EDGE_LOOP('',(#11145,#11146,#11147,#11148));
#2741=EDGE_LOOP('',(#11149,#11150,#11151,#11152));
#2742=EDGE_LOOP('',(#11153,#11154,#11155,#11156));
#2743=EDGE_LOOP('',(#11157,#11158,#11159,#11160));
#2744=EDGE_LOOP('',(#11161,#11162,#11163,#11164));
#2745=EDGE_LOOP('',(#11165,#11166,#11167,#11168));
#2746=EDGE_LOOP('',(#11169,#11170,#11171,#11172,#11173,#11174));
#2747=EDGE_LOOP('',(#11175,#11176,#11177,#11178));
#2748=EDGE_LOOP('',(#11179));
#2749=EDGE_LOOP('',(#11180));
#2750=EDGE_LOOP('',(#11181));
#2751=EDGE_LOOP('',(#11182));
#2752=EDGE_LOOP('',(#11183,#11184,#11185,#11186));
#2753=EDGE_LOOP('',(#11187,#11188,#11189,#11190));
#2754=EDGE_LOOP('',(#11191,#11192,#11193,#11194));
#2755=EDGE_LOOP('',(#11195,#11196,#11197,#11198));
#2756=EDGE_LOOP('',(#11199,#11200,#11201,#11202));
#2757=EDGE_LOOP('',(#11203,#11204,#11205,#11206));
#2758=EDGE_LOOP('',(#11207,#11208,#11209,#11210,#11211,#11212));
#2759=EDGE_LOOP('',(#11213,#11214,#11215,#11216));
#2760=EDGE_LOOP('',(#11217));
#2761=EDGE_LOOP('',(#11218));
#2762=EDGE_LOOP('',(#11219));
#2763=EDGE_LOOP('',(#11220));
#2764=EDGE_LOOP('',(#11221,#11222,#11223,#11224));
#2765=EDGE_LOOP('',(#11225,#11226,#11227,#11228));
#2766=EDGE_LOOP('',(#11229,#11230,#11231,#11232));
#2767=EDGE_LOOP('',(#11233,#11234,#11235,#11236));
#2768=EDGE_LOOP('',(#11237,#11238,#11239,#11240));
#2769=EDGE_LOOP('',(#11241,#11242,#11243,#11244));
#2770=EDGE_LOOP('',(#11245,#11246,#11247,#11248,#11249,#11250));
#2771=EDGE_LOOP('',(#11251,#11252,#11253,#11254));
#2772=EDGE_LOOP('',(#11255));
#2773=EDGE_LOOP('',(#11256));
#2774=EDGE_LOOP('',(#11257));
#2775=EDGE_LOOP('',(#11258));
#2776=EDGE_LOOP('',(#11259,#11260,#11261,#11262));
#2777=EDGE_LOOP('',(#11263,#11264,#11265,#11266));
#2778=EDGE_LOOP('',(#11267,#11268,#11269,#11270));
#2779=EDGE_LOOP('',(#11271,#11272,#11273,#11274));
#2780=EDGE_LOOP('',(#11275,#11276,#11277,#11278));
#2781=EDGE_LOOP('',(#11279,#11280,#11281,#11282));
#2782=EDGE_LOOP('',(#11283,#11284,#11285,#11286,#11287,#11288));
#2783=EDGE_LOOP('',(#11289,#11290,#11291,#11292));
#2784=EDGE_LOOP('',(#11293));
#2785=EDGE_LOOP('',(#11294));
#2786=EDGE_LOOP('',(#11295));
#2787=EDGE_LOOP('',(#11296));
#2788=EDGE_LOOP('',(#11297,#11298,#11299,#11300));
#2789=EDGE_LOOP('',(#11301,#11302,#11303,#11304));
#2790=EDGE_LOOP('',(#11305,#11306,#11307,#11308));
#2791=EDGE_LOOP('',(#11309,#11310,#11311,#11312));
#2792=EDGE_LOOP('',(#11313,#11314,#11315,#11316));
#2793=EDGE_LOOP('',(#11317,#11318,#11319,#11320));
#2794=EDGE_LOOP('',(#11321,#11322,#11323,#11324,#11325,#11326));
#2795=EDGE_LOOP('',(#11327,#11328,#11329,#11330));
#2796=EDGE_LOOP('',(#11331));
#2797=EDGE_LOOP('',(#11332));
#2798=EDGE_LOOP('',(#11333));
#2799=EDGE_LOOP('',(#11334));
#2800=EDGE_LOOP('',(#11335,#11336,#11337,#11338));
#2801=EDGE_LOOP('',(#11339,#11340,#11341,#11342));
#2802=EDGE_LOOP('',(#11343,#11344,#11345,#11346));
#2803=EDGE_LOOP('',(#11347,#11348,#11349,#11350));
#2804=EDGE_LOOP('',(#11351,#11352,#11353,#11354));
#2805=EDGE_LOOP('',(#11355,#11356,#11357,#11358,#11359,#11360));
#2806=EDGE_LOOP('',(#11361,#11362,#11363,#11364));
#2807=EDGE_LOOP('',(#11365,#11366,#11367,#11368));
#2808=EDGE_LOOP('',(#11369,#11370,#11371,#11372));
#2809=EDGE_LOOP('',(#11373,#11374,#11375,#11376,#11377,#11378));
#2810=EDGE_LOOP('',(#11379,#11380,#11381,#11382,#11383));
#2811=EDGE_LOOP('',(#11384,#11385,#11386,#11387,#11388));
#2812=EDGE_LOOP('',(#11389,#11390,#11391,#11392,#11393,#11394));
#2813=EDGE_LOOP('',(#11395,#11396,#11397,#11398));
#2814=EDGE_LOOP('',(#11399,#11400,#11401,#11402));
#2815=EDGE_LOOP('',(#11403,#11404,#11405,#11406));
#2816=EDGE_LOOP('',(#11407));
#2817=EDGE_LOOP('',(#11408));
#2818=EDGE_LOOP('',(#11409));
#2819=EDGE_LOOP('',(#11410));
#2820=EDGE_LOOP('',(#11411,#11412));
#2821=EDGE_LOOP('',(#11413,#11414));
#2822=EDGE_LOOP('',(#11415,#11416));
#2823=EDGE_LOOP('',(#11417,#11418));
#2824=EDGE_LOOP('',(#11419,#11420));
#2825=EDGE_LOOP('',(#11421,#11422));
#2826=EDGE_LOOP('',(#11423,#11424));
#2827=EDGE_LOOP('',(#11425,#11426,#11427,#11428,#11429));
#2828=EDGE_LOOP('',(#11430,#11431,#11432,#11433));
#2829=EDGE_LOOP('',(#11434,#11435,#11436,#11437));
#2830=EDGE_LOOP('',(#11438,#11439,#11440,#11441,#11442));
#2831=EDGE_LOOP('',(#11443,#11444,#11445,#11446));
#2832=EDGE_LOOP('',(#11447,#11448,#11449,#11450,#11451));
#2833=EDGE_LOOP('',(#11452,#11453,#11454,#11455,#11456));
#2834=EDGE_LOOP('',(#11457,#11458,#11459,#11460));
#2835=EDGE_LOOP('',(#11461,#11462,#11463,#11464));
#2836=EDGE_LOOP('',(#11465,#11466,#11467,#11468));
#2837=EDGE_LOOP('',(#11469,#11470,#11471,#11472));
#2838=EDGE_LOOP('',(#11473,#11474,#11475,#11476));
#2839=EDGE_LOOP('',(#11477,#11478,#11479,#11480,#11481));
#2840=EDGE_LOOP('',(#11482,#11483,#11484,#11485,#11486));
#2841=EDGE_LOOP('',(#11487));
#2842=EDGE_LOOP('',(#11488));
#2843=EDGE_LOOP('',(#11489));
#2844=EDGE_LOOP('',(#11490));
#2845=EDGE_LOOP('',(#11491));
#2846=EDGE_LOOP('',(#11492));
#2847=EDGE_LOOP('',(#11493));
#2848=EDGE_LOOP('',(#11494));
#2849=EDGE_LOOP('',(#11495));
#2850=EDGE_LOOP('',(#11496));
#2851=EDGE_LOOP('',(#11497));
#2852=EDGE_LOOP('',(#11498));
#2853=EDGE_LOOP('',(#11499,#11500,#11501,#11502));
#2854=EDGE_LOOP('',(#11503,#11504,#11505,#11506));
#2855=EDGE_LOOP('',(#11507,#11508,#11509,#11510));
#2856=EDGE_LOOP('',(#11511,#11512,#11513,#11514,#11515,#11516,#11517,#11518,
#11519,#11520,#11521,#11522));
#2857=EDGE_LOOP('',(#11523));
#2858=EDGE_LOOP('',(#11524));
#2859=EDGE_LOOP('',(#11525,#11526,#11527,#11528));
#2860=EDGE_LOOP('',(#11529,#11530,#11531,#11532));
#2861=EDGE_LOOP('',(#11533,#11534,#11535,#11536));
#2862=EDGE_LOOP('',(#11537,#11538,#11539,#11540,#11541,#11542,#11543,#11544,
#11545,#11546,#11547,#11548));
#2863=EDGE_LOOP('',(#11549));
#2864=EDGE_LOOP('',(#11550));
#2865=EDGE_LOOP('',(#11551,#11552,#11553,#11554));
#2866=EDGE_LOOP('',(#11555,#11556,#11557,#11558));
#2867=EDGE_LOOP('',(#11559,#11560,#11561,#11562));
#2868=EDGE_LOOP('',(#11563,#11564,#11565,#11566,#11567,#11568,#11569,#11570,
#11571,#11572,#11573,#11574));
#2869=EDGE_LOOP('',(#11575));
#2870=EDGE_LOOP('',(#11576));
#2871=EDGE_LOOP('',(#11577,#11578,#11579,#11580));
#2872=EDGE_LOOP('',(#11581,#11582,#11583,#11584));
#2873=EDGE_LOOP('',(#11585,#11586,#11587,#11588));
#2874=EDGE_LOOP('',(#11589,#11590,#11591,#11592,#11593,#11594,#11595,#11596,
#11597,#11598,#11599,#11600));
#2875=EDGE_LOOP('',(#11601));
#2876=EDGE_LOOP('',(#11602));
#2877=EDGE_LOOP('',(#11603,#11604,#11605,#11606));
#2878=EDGE_LOOP('',(#11607,#11608,#11609,#11610));
#2879=EDGE_LOOP('',(#11611,#11612,#11613,#11614));
#2880=EDGE_LOOP('',(#11615,#11616,#11617,#11618,#11619,#11620,#11621,#11622,
#11623,#11624,#11625,#11626));
#2881=EDGE_LOOP('',(#11627));
#2882=EDGE_LOOP('',(#11628));
#2883=EDGE_LOOP('',(#11629,#11630,#11631,#11632));
#2884=EDGE_LOOP('',(#11633,#11634,#11635,#11636));
#2885=EDGE_LOOP('',(#11637,#11638,#11639,#11640));
#2886=EDGE_LOOP('',(#11641,#11642,#11643,#11644,#11645,#11646,#11647,#11648,
#11649,#11650,#11651,#11652));
#2887=EDGE_LOOP('',(#11653));
#2888=EDGE_LOOP('',(#11654));
#2889=EDGE_LOOP('',(#11655,#11656,#11657,#11658,#11659,#11660,#11661,#11662,
#11663,#11664,#11665,#11666));
#2890=EDGE_LOOP('',(#11667));
#2891=EDGE_LOOP('',(#11668));
#2892=EDGE_LOOP('',(#11669,#11670,#11671,#11672));
#2893=EDGE_LOOP('',(#11673,#11674,#11675,#11676));
#2894=EDGE_LOOP('',(#11677,#11678,#11679,#11680));
#2895=EDGE_LOOP('',(#11681,#11682,#11683,#11684));
#2896=EDGE_LOOP('',(#11685,#11686,#11687,#11688));
#2897=EDGE_LOOP('',(#11689,#11690,#11691,#11692));
#2898=EDGE_LOOP('',(#11693,#11694,#11695,#11696));
#2899=EDGE_LOOP('',(#11697));
#2900=EDGE_LOOP('',(#11698));
#2901=EDGE_LOOP('',(#11699));
#2902=EDGE_LOOP('',(#11700));
#2903=EDGE_LOOP('',(#11701,#11702,#11703,#11704));
#2904=EDGE_LOOP('',(#11705,#11706,#11707,#11708,#11709,#11710));
#2905=EDGE_LOOP('',(#11711,#11712,#11713,#11714));
#2906=EDGE_LOOP('',(#11715,#11716,#11717,#11718));
#2907=EDGE_LOOP('',(#11719));
#2908=EDGE_LOOP('',(#11720));
#2909=EDGE_LOOP('',(#11721));
#2910=EDGE_LOOP('',(#11722));
#2911=EDGE_LOOP('',(#11723,#11724,#11725,#11726));
#2912=EDGE_LOOP('',(#11727,#11728,#11729,#11730));
#2913=EDGE_LOOP('',(#11731,#11732,#11733,#11734));
#2914=EDGE_LOOP('',(#11735,#11736,#11737,#11738));
#2915=EDGE_LOOP('',(#11739,#11740,#11741,#11742));
#2916=EDGE_LOOP('',(#11743,#11744,#11745,#11746));
#2917=EDGE_LOOP('',(#11747,#11748,#11749,#11750,#11751,#11752));
#2918=EDGE_LOOP('',(#11753,#11754,#11755,#11756));
#2919=EDGE_LOOP('',(#11757));
#2920=EDGE_LOOP('',(#11758));
#2921=EDGE_LOOP('',(#11759));
#2922=EDGE_LOOP('',(#11760));
#2923=EDGE_LOOP('',(#11761,#11762,#11763,#11764));
#2924=EDGE_LOOP('',(#11765,#11766,#11767,#11768));
#2925=EDGE_LOOP('',(#11769,#11770,#11771,#11772));
#2926=EDGE_LOOP('',(#11773,#11774,#11775,#11776));
#2927=EDGE_LOOP('',(#11777,#11778,#11779,#11780));
#2928=EDGE_LOOP('',(#11781,#11782,#11783,#11784));
#2929=EDGE_LOOP('',(#11785,#11786,#11787,#11788,#11789,#11790));
#2930=EDGE_LOOP('',(#11791,#11792,#11793,#11794));
#2931=EDGE_LOOP('',(#11795));
#2932=EDGE_LOOP('',(#11796));
#2933=EDGE_LOOP('',(#11797));
#2934=EDGE_LOOP('',(#11798));
#2935=EDGE_LOOP('',(#11799,#11800,#11801,#11802));
#2936=EDGE_LOOP('',(#11803,#11804,#11805,#11806));
#2937=EDGE_LOOP('',(#11807,#11808,#11809,#11810));
#2938=EDGE_LOOP('',(#11811,#11812,#11813,#11814));
#2939=EDGE_LOOP('',(#11815,#11816,#11817,#11818));
#2940=EDGE_LOOP('',(#11819,#11820,#11821,#11822));
#2941=EDGE_LOOP('',(#11823,#11824,#11825,#11826,#11827,#11828));
#2942=EDGE_LOOP('',(#11829,#11830,#11831,#11832));
#2943=EDGE_LOOP('',(#11833));
#2944=EDGE_LOOP('',(#11834));
#2945=EDGE_LOOP('',(#11835));
#2946=EDGE_LOOP('',(#11836));
#2947=EDGE_LOOP('',(#11837,#11838,#11839,#11840));
#2948=EDGE_LOOP('',(#11841,#11842,#11843,#11844));
#2949=EDGE_LOOP('',(#11845,#11846,#11847,#11848));
#2950=EDGE_LOOP('',(#11849,#11850,#11851,#11852));
#2951=EDGE_LOOP('',(#11853,#11854,#11855,#11856));
#2952=EDGE_LOOP('',(#11857,#11858,#11859,#11860));
#2953=EDGE_LOOP('',(#11861,#11862,#11863,#11864,#11865,#11866));
#2954=EDGE_LOOP('',(#11867,#11868,#11869,#11870));
#2955=EDGE_LOOP('',(#11871));
#2956=EDGE_LOOP('',(#11872));
#2957=EDGE_LOOP('',(#11873));
#2958=EDGE_LOOP('',(#11874));
#2959=EDGE_LOOP('',(#11875,#11876,#11877,#11878));
#2960=EDGE_LOOP('',(#11879,#11880,#11881,#11882));
#2961=EDGE_LOOP('',(#11883,#11884,#11885,#11886));
#2962=EDGE_LOOP('',(#11887,#11888,#11889,#11890));
#2963=EDGE_LOOP('',(#11891,#11892,#11893,#11894));
#2964=EDGE_LOOP('',(#11895,#11896,#11897,#11898));
#2965=EDGE_LOOP('',(#11899,#11900,#11901,#11902,#11903,#11904));
#2966=EDGE_LOOP('',(#11905,#11906,#11907,#11908));
#2967=EDGE_LOOP('',(#11909));
#2968=EDGE_LOOP('',(#11910));
#2969=EDGE_LOOP('',(#11911));
#2970=EDGE_LOOP('',(#11912));
#2971=EDGE_LOOP('',(#11913,#11914,#11915,#11916));
#2972=EDGE_LOOP('',(#11917,#11918,#11919,#11920));
#2973=EDGE_LOOP('',(#11921,#11922,#11923,#11924));
#2974=EDGE_LOOP('',(#11925,#11926,#11927,#11928));
#2975=EDGE_LOOP('',(#11929,#11930,#11931,#11932));
#2976=EDGE_LOOP('',(#11933,#11934,#11935,#11936,#11937,#11938));
#2977=EDGE_LOOP('',(#11939,#11940,#11941,#11942));
#2978=EDGE_LOOP('',(#11943,#11944,#11945,#11946));
#2979=EDGE_LOOP('',(#11947,#11948,#11949,#11950));
#2980=EDGE_LOOP('',(#11951,#11952,#11953,#11954));
#2981=EDGE_LOOP('',(#11955));
#2982=EDGE_LOOP('',(#11956));
#2983=EDGE_LOOP('',(#11957,#11958,#11959,#11960));
#2984=EDGE_LOOP('',(#11961,#11962,#11963,#11964));
#2985=EDGE_LOOP('',(#11965));
#2986=EDGE_LOOP('',(#11966));
#2987=EDGE_LOOP('',(#11967,#11968,#11969,#11970));
#2988=EDGE_LOOP('',(#11971,#11972,#11973,#11974));
#2989=EDGE_LOOP('',(#11975,#11976,#11977,#11978));
#2990=EDGE_LOOP('',(#11979,#11980,#11981,#11982));
#2991=EDGE_LOOP('',(#11983,#11984,#11985,#11986));
#2992=EDGE_LOOP('',(#11987,#11988,#11989,#11990));
#2993=EDGE_LOOP('',(#11991,#11992,#11993,#11994));
#2994=EDGE_LOOP('',(#11995));
#2995=EDGE_LOOP('',(#11996));
#2996=EDGE_LOOP('',(#11997,#11998,#11999,#12000));
#2997=EDGE_LOOP('',(#12001,#12002,#12003,#12004));
#2998=EDGE_LOOP('',(#12005,#12006,#12007,#12008));
#2999=EDGE_LOOP('',(#12009,#12010,#12011,#12012));
#3000=EDGE_LOOP('',(#12013,#12014,#12015,#12016));
#3001=EDGE_LOOP('',(#12017));
#3002=EDGE_LOOP('',(#12018));
#3003=LINE('',#18825,#3451);
#3004=LINE('',#18831,#3452);
#3005=LINE('',#18840,#3453);
#3006=LINE('',#18843,#3454);
#3007=LINE('',#18846,#3455);
#3008=LINE('',#18848,#3456);
#3009=LINE('',#18849,#3457);
#3010=LINE('',#18855,#3458);
#3011=LINE('',#18858,#3459);
#3012=LINE('',#18861,#3460);
#3013=LINE('',#18863,#3461);
#3014=LINE('',#18864,#3462);
#3015=LINE('',#18870,#3463);
#3016=LINE('',#18873,#3464);
#3017=LINE('',#18876,#3465);
#3018=LINE('',#18878,#3466);
#3019=LINE('',#18879,#3467);
#3020=LINE('',#18885,#3468);
#3021=LINE('',#18888,#3469);
#3022=LINE('',#18891,#3470);
#3023=LINE('',#18893,#3471);
#3024=LINE('',#18894,#3472);
#3025=LINE('',#18900,#3473);
#3026=LINE('',#18903,#3474);
#3027=LINE('',#18906,#3475);
#3028=LINE('',#18908,#3476);
#3029=LINE('',#18909,#3477);
#3030=LINE('',#18915,#3478);
#3031=LINE('',#18918,#3479);
#3032=LINE('',#18921,#3480);
#3033=LINE('',#18923,#3481);
#3034=LINE('',#18924,#3482);
#3035=LINE('',#18930,#3483);
#3036=LINE('',#18933,#3484);
#3037=LINE('',#18936,#3485);
#3038=LINE('',#18938,#3486);
#3039=LINE('',#18939,#3487);
#3040=LINE('',#18945,#3488);
#3041=LINE('',#18948,#3489);
#3042=LINE('',#18951,#3490);
#3043=LINE('',#18953,#3491);
#3044=LINE('',#18954,#3492);
#3045=LINE('',#18960,#3493);
#3046=LINE('',#18963,#3494);
#3047=LINE('',#18966,#3495);
#3048=LINE('',#18968,#3496);
#3049=LINE('',#18969,#3497);
#3050=LINE('',#18975,#3498);
#3051=LINE('',#18978,#3499);
#3052=LINE('',#18981,#3500);
#3053=LINE('',#18983,#3501);
#3054=LINE('',#18984,#3502);
#3055=LINE('',#18990,#3503);
#3056=LINE('',#18993,#3504);
#3057=LINE('',#18996,#3505);
#3058=LINE('',#18998,#3506);
#3059=LINE('',#18999,#3507);
#3060=LINE('',#19005,#3508);
#3061=LINE('',#19008,#3509);
#3062=LINE('',#19011,#3510);
#3063=LINE('',#19013,#3511);
#3064=LINE('',#19014,#3512);
#3065=LINE('',#19020,#3513);
#3066=LINE('',#19023,#3514);
#3067=LINE('',#19026,#3515);
#3068=LINE('',#19028,#3516);
#3069=LINE('',#19029,#3517);
#3070=LINE('',#19035,#3518);
#3071=LINE('',#19038,#3519);
#3072=LINE('',#19041,#3520);
#3073=LINE('',#19043,#3521);
#3074=LINE('',#19044,#3522);
#3075=LINE('',#19050,#3523);
#3076=LINE('',#19053,#3524);
#3077=LINE('',#19056,#3525);
#3078=LINE('',#19058,#3526);
#3079=LINE('',#19059,#3527);
#3080=LINE('',#19065,#3528);
#3081=LINE('',#19068,#3529);
#3082=LINE('',#19071,#3530);
#3083=LINE('',#19073,#3531);
#3084=LINE('',#19074,#3532);
#3085=LINE('',#19080,#3533);
#3086=LINE('',#19083,#3534);
#3087=LINE('',#19086,#3535);
#3088=LINE('',#19088,#3536);
#3089=LINE('',#19089,#3537);
#3090=LINE('',#19095,#3538);
#3091=LINE('',#19098,#3539);
#3092=LINE('',#19101,#3540);
#3093=LINE('',#19103,#3541);
#3094=LINE('',#19104,#3542);
#3095=LINE('',#19110,#3543);
#3096=LINE('',#19113,#3544);
#3097=LINE('',#19116,#3545);
#3098=LINE('',#19118,#3546);
#3099=LINE('',#19119,#3547);
#3100=LINE('',#19125,#3548);
#3101=LINE('',#19128,#3549);
#3102=LINE('',#19131,#3550);
#3103=LINE('',#19133,#3551);
#3104=LINE('',#19134,#3552);
#3105=LINE('',#19140,#3553);
#3106=LINE('',#19143,#3554);
#3107=LINE('',#19146,#3555);
#3108=LINE('',#19148,#3556);
#3109=LINE('',#19149,#3557);
#3110=LINE('',#19155,#3558);
#3111=LINE('',#19158,#3559);
#3112=LINE('',#19161,#3560);
#3113=LINE('',#19163,#3561);
#3114=LINE('',#19164,#3562);
#3115=LINE('',#19170,#3563);
#3116=LINE('',#19173,#3564);
#3117=LINE('',#19176,#3565);
#3118=LINE('',#19178,#3566);
#3119=LINE('',#19179,#3567);
#3120=LINE('',#19185,#3568);
#3121=LINE('',#19188,#3569);
#3122=LINE('',#19191,#3570);
#3123=LINE('',#19193,#3571);
#3124=LINE('',#19194,#3572);
#3125=LINE('',#19200,#3573);
#3126=LINE('',#19203,#3574);
#3127=LINE('',#19206,#3575);
#3128=LINE('',#19208,#3576);
#3129=LINE('',#19209,#3577);
#3130=LINE('',#19215,#3578);
#3131=LINE('',#19218,#3579);
#3132=LINE('',#19221,#3580);
#3133=LINE('',#19223,#3581);
#3134=LINE('',#19224,#3582);
#3135=LINE('',#19230,#3583);
#3136=LINE('',#19233,#3584);
#3137=LINE('',#19236,#3585);
#3138=LINE('',#19238,#3586);
#3139=LINE('',#19239,#3587);
#3140=LINE('',#19245,#3588);
#3141=LINE('',#19248,#3589);
#3142=LINE('',#19251,#3590);
#3143=LINE('',#19253,#3591);
#3144=LINE('',#19254,#3592);
#3145=LINE('',#19260,#3593);
#3146=LINE('',#19263,#3594);
#3147=LINE('',#19266,#3595);
#3148=LINE('',#19268,#3596);
#3149=LINE('',#19269,#3597);
#3150=LINE('',#19275,#3598);
#3151=LINE('',#19278,#3599);
#3152=LINE('',#19281,#3600);
#3153=LINE('',#19283,#3601);
#3154=LINE('',#19284,#3602);
#3155=LINE('',#19290,#3603);
#3156=LINE('',#19293,#3604);
#3157=LINE('',#19296,#3605);
#3158=LINE('',#19298,#3606);
#3159=LINE('',#19299,#3607);
#3160=LINE('',#19305,#3608);
#3161=LINE('',#19308,#3609);
#3162=LINE('',#19311,#3610);
#3163=LINE('',#19313,#3611);
#3164=LINE('',#19314,#3612);
#3165=LINE('',#19320,#3613);
#3166=LINE('',#19323,#3614);
#3167=LINE('',#19326,#3615);
#3168=LINE('',#19328,#3616);
#3169=LINE('',#19329,#3617);
#3170=LINE('',#19335,#3618);
#3171=LINE('',#19338,#3619);
#3172=LINE('',#19341,#3620);
#3173=LINE('',#19343,#3621);
#3174=LINE('',#19344,#3622);
#3175=LINE('',#19350,#3623);
#3176=LINE('',#19353,#3624);
#3177=LINE('',#19356,#3625);
#3178=LINE('',#19358,#3626);
#3179=LINE('',#19359,#3627);
#3180=LINE('',#19365,#3628);
#3181=LINE('',#19368,#3629);
#3182=LINE('',#19371,#3630);
#3183=LINE('',#19373,#3631);
#3184=LINE('',#19374,#3632);
#3185=LINE('',#19380,#3633);
#3186=LINE('',#19383,#3634);
#3187=LINE('',#19386,#3635);
#3188=LINE('',#19388,#3636);
#3189=LINE('',#19389,#3637);
#3190=LINE('',#19395,#3638);
#3191=LINE('',#19398,#3639);
#3192=LINE('',#19401,#3640);
#3193=LINE('',#19403,#3641);
#3194=LINE('',#19404,#3642);
#3195=LINE('',#19706,#3643);
#3196=LINE('',#19712,#3644);
#3197=LINE('',#20312,#3645);
#3198=LINE('',#20318,#3646);
#3199=LINE('',#20918,#3647);
#3200=LINE('',#20924,#3648);
#3201=LINE('',#21524,#3649);
#3202=LINE('',#21530,#3650);
#3203=LINE('',#22130,#3651);
#3204=LINE('',#22136,#3652);
#3205=LINE('',#22736,#3653);
#3206=LINE('',#22742,#3654);
#3207=LINE('',#23342,#3655);
#3208=LINE('',#23348,#3656);
#3209=LINE('',#23948,#3657);
#3210=LINE('',#23954,#3658);
#3211=LINE('',#24554,#3659);
#3212=LINE('',#24560,#3660);
#3213=LINE('',#25160,#3661);
#3214=LINE('',#25166,#3662);
#3215=LINE('',#25766,#3663);
#3216=LINE('',#25772,#3664);
#3217=LINE('',#26372,#3665);
#3218=LINE('',#26378,#3666);
#3219=LINE('',#26978,#3667);
#3220=LINE('',#26984,#3668);
#3221=LINE('',#27584,#3669);
#3222=LINE('',#27590,#3670);
#3223=LINE('',#28190,#3671);
#3224=LINE('',#28196,#3672);
#3225=LINE('',#28796,#3673);
#3226=LINE('',#28802,#3674);
#3227=LINE('',#29402,#3675);
#3228=LINE('',#29408,#3676);
#3229=LINE('',#30008,#3677);
#3230=LINE('',#30014,#3678);
#3231=LINE('',#30614,#3679);
#3232=LINE('',#30620,#3680);
#3233=LINE('',#30942,#3681);
#3234=LINE('',#31096,#3682);
#3235=LINE('',#31107,#3683);
#3236=LINE('',#31262,#3684);
#3237=LINE('',#31285,#3685);
#3238=LINE('',#31305,#3686);
#3239=LINE('',#31307,#3687);
#3240=LINE('',#31309,#3688);
#3241=LINE('',#31310,#3689);
#3242=LINE('',#31312,#3690);
#3243=LINE('',#31463,#3691);
#3244=LINE('',#31465,#3692);
#3245=LINE('',#31622,#3693);
#3246=LINE('',#31628,#3694);
#3247=LINE('',#31637,#3695);
#3248=LINE('',#31640,#3696);
#3249=LINE('',#31643,#3697);
#3250=LINE('',#31645,#3698);
#3251=LINE('',#31646,#3699);
#3252=LINE('',#31652,#3700);
#3253=LINE('',#31655,#3701);
#3254=LINE('',#31658,#3702);
#3255=LINE('',#31660,#3703);
#3256=LINE('',#31661,#3704);
#3257=LINE('',#31667,#3705);
#3258=LINE('',#31670,#3706);
#3259=LINE('',#31673,#3707);
#3260=LINE('',#31675,#3708);
#3261=LINE('',#31676,#3709);
#3262=LINE('',#31682,#3710);
#3263=LINE('',#31685,#3711);
#3264=LINE('',#31688,#3712);
#3265=LINE('',#31690,#3713);
#3266=LINE('',#31691,#3714);
#3267=LINE('',#31697,#3715);
#3268=LINE('',#31700,#3716);
#3269=LINE('',#31703,#3717);
#3270=LINE('',#31705,#3718);
#3271=LINE('',#31706,#3719);
#3272=LINE('',#31712,#3720);
#3273=LINE('',#31715,#3721);
#3274=LINE('',#31718,#3722);
#3275=LINE('',#31720,#3723);
#3276=LINE('',#31721,#3724);
#3277=LINE('',#31727,#3725);
#3278=LINE('',#31730,#3726);
#3279=LINE('',#31733,#3727);
#3280=LINE('',#31735,#3728);
#3281=LINE('',#31736,#3729);
#3282=LINE('',#31742,#3730);
#3283=LINE('',#31745,#3731);
#3284=LINE('',#31748,#3732);
#3285=LINE('',#31750,#3733);
#3286=LINE('',#31751,#3734);
#3287=LINE('',#31757,#3735);
#3288=LINE('',#31760,#3736);
#3289=LINE('',#31763,#3737);
#3290=LINE('',#31765,#3738);
#3291=LINE('',#31766,#3739);
#3292=LINE('',#31772,#3740);
#3293=LINE('',#31775,#3741);
#3294=LINE('',#31778,#3742);
#3295=LINE('',#31780,#3743);
#3296=LINE('',#31781,#3744);
#3297=LINE('',#31787,#3745);
#3298=LINE('',#31790,#3746);
#3299=LINE('',#31793,#3747);
#3300=LINE('',#31795,#3748);
#3301=LINE('',#31796,#3749);
#3302=LINE('',#31802,#3750);
#3303=LINE('',#31805,#3751);
#3304=LINE('',#31808,#3752);
#3305=LINE('',#31810,#3753);
#3306=LINE('',#31811,#3754);
#3307=LINE('',#31817,#3755);
#3308=LINE('',#31820,#3756);
#3309=LINE('',#31823,#3757);
#3310=LINE('',#31825,#3758);
#3311=LINE('',#31826,#3759);
#3312=LINE('',#31832,#3760);
#3313=LINE('',#31835,#3761);
#3314=LINE('',#31838,#3762);
#3315=LINE('',#31840,#3763);
#3316=LINE('',#31841,#3764);
#3317=LINE('',#31847,#3765);
#3318=LINE('',#31850,#3766);
#3319=LINE('',#31853,#3767);
#3320=LINE('',#31855,#3768);
#3321=LINE('',#31856,#3769);
#3322=LINE('',#31862,#3770);
#3323=LINE('',#31865,#3771);
#3324=LINE('',#31868,#3772);
#3325=LINE('',#31870,#3773);
#3326=LINE('',#31871,#3774);
#3327=LINE('',#31877,#3775);
#3328=LINE('',#31880,#3776);
#3329=LINE('',#31883,#3777);
#3330=LINE('',#31885,#3778);
#3331=LINE('',#31886,#3779);
#3332=LINE('',#31892,#3780);
#3333=LINE('',#31895,#3781);
#3334=LINE('',#31898,#3782);
#3335=LINE('',#31900,#3783);
#3336=LINE('',#31901,#3784);
#3337=LINE('',#32203,#3785);
#3338=LINE('',#32209,#3786);
#3339=LINE('',#32809,#3787);
#3340=LINE('',#32815,#3788);
#3341=LINE('',#33415,#3789);
#3342=LINE('',#33421,#3790);
#3343=LINE('',#34021,#3791);
#3344=LINE('',#34027,#3792);
#3345=LINE('',#34627,#3793);
#3346=LINE('',#34633,#3794);
#3347=LINE('',#35233,#3795);
#3348=LINE('',#35239,#3796);
#3349=LINE('',#35839,#3797);
#3350=LINE('',#35845,#3798);
#3351=LINE('',#36445,#3799);
#3352=LINE('',#36451,#3800);
#3353=LINE('',#37051,#3801);
#3354=LINE('',#37057,#3802);
#3355=LINE('',#37369,#3803);
#3356=LINE('',#37523,#3804);
#3357=LINE('',#37534,#3805);
#3358=LINE('',#37689,#3806);
#3359=LINE('',#37702,#3807);
#3360=LINE('',#37712,#3808);
#3361=LINE('',#37714,#3809);
#3362=LINE('',#37716,#3810);
#3363=LINE('',#37717,#3811);
#3364=LINE('',#37719,#3812);
#3365=LINE('',#37870,#3813);
#3366=LINE('',#37872,#3814);
#3367=LINE('',#38051,#3815);
#3368=LINE('',#38054,#3816);
#3369=LINE('',#38057,#3817);
#3370=LINE('',#38061,#3818);
#3371=LINE('',#38066,#3819);
#3372=LINE('',#38129,#3820);
#3373=LINE('',#38134,#3821);
#3374=LINE('',#38137,#3822);
#3375=LINE('',#38144,#3823);
#3376=LINE('',#38147,#3824);
#3377=LINE('',#38153,#3825);
#3378=LINE('',#38159,#3826);
#3379=LINE('',#38166,#3827);
#3380=LINE('',#38170,#3828);
#3381=LINE('',#39464,#3829);
#3382=LINE('',#39467,#3830);
#3383=LINE('',#39470,#3831);
#3384=LINE('',#39474,#3832);
#3385=LINE('',#39479,#3833);
#3386=LINE('',#39542,#3834);
#3387=LINE('',#39547,#3835);
#3388=LINE('',#39550,#3836);
#3389=LINE('',#39557,#3837);
#3390=LINE('',#39560,#3838);
#3391=LINE('',#39566,#3839);
#3392=LINE('',#39572,#3840);
#3393=LINE('',#39579,#3841);
#3394=LINE('',#39583,#3842);
#3395=LINE('',#40877,#3843);
#3396=LINE('',#40880,#3844);
#3397=LINE('',#40883,#3845);
#3398=LINE('',#40888,#3846);
#3399=LINE('',#40891,#3847);
#3400=LINE('',#40955,#3848);
#3401=LINE('',#40959,#3849);
#3402=LINE('',#40964,#3850);
#3403=LINE('',#40970,#3851);
#3404=LINE('',#40974,#3852);
#3405=LINE('',#40979,#3853);
#3406=LINE('',#40985,#3854);
#3407=LINE('',#40993,#3855);
#3408=LINE('',#40996,#3856);
#3409=LINE('',#42290,#3857);
#3410=LINE('',#42293,#3858);
#3411=LINE('',#42296,#3859);
#3412=LINE('',#42301,#3860);
#3413=LINE('',#42304,#3861);
#3414=LINE('',#42368,#3862);
#3415=LINE('',#42372,#3863);
#3416=LINE('',#42377,#3864);
#3417=LINE('',#42383,#3865);
#3418=LINE('',#42387,#3866);
#3419=LINE('',#42392,#3867);
#3420=LINE('',#42398,#3868);
#3421=LINE('',#42406,#3869);
#3422=LINE('',#42409,#3870);
#3423=LINE('',#43681,#3871);
#3424=LINE('',#43686,#3872);
#3425=LINE('',#43688,#3873);
#3426=LINE('',#43690,#3874);
#3427=LINE('',#43691,#3875);
#3428=LINE('',#43696,#3876);
#3429=LINE('',#43701,#3877);
#3430=LINE('',#43703,#3878);
#3431=LINE('',#43705,#3879);
#3432=LINE('',#43706,#3880);
#3433=LINE('',#43708,#3881);
#3434=LINE('',#43709,#3882);
#3435=LINE('',#43711,#3883);
#3436=LINE('',#43713,#3884);
#3437=LINE('',#43720,#3885);
#3438=LINE('',#43726,#3886);
#3439=LINE('',#43731,#3887);
#3440=LINE('',#43733,#3888);
#3441=LINE('',#43735,#3889);
#3442=LINE('',#43736,#3890);
#3443=LINE('',#43739,#3891);
#3444=LINE('',#43741,#3892);
#3445=LINE('',#43742,#3893);
#3446=LINE('',#43745,#3894);
#3447=LINE('',#43746,#3895);
#3448=LINE('',#43749,#3896);
#3449=LINE('',#43750,#3897);
#3450=LINE('',#43752,#3898);
#3451=VECTOR('',#14921,7.5);
#3452=VECTOR('',#14928,7.5);
#3453=VECTOR('',#14939,10.);
#3454=VECTOR('',#14942,10.);
#3455=VECTOR('',#14945,10.);
#3456=VECTOR('',#14946,10.);
#3457=VECTOR('',#14947,10.);
#3458=VECTOR('',#14952,10.);
#3459=VECTOR('',#14955,10.);
#3460=VECTOR('',#14958,10.);
#3461=VECTOR('',#14959,10.);
#3462=VECTOR('',#14960,10.);
#3463=VECTOR('',#14965,10.);
#3464=VECTOR('',#14968,10.);
#3465=VECTOR('',#14971,10.);
#3466=VECTOR('',#14972,10.);
#3467=VECTOR('',#14973,10.);
#3468=VECTOR('',#14978,10.);
#3469=VECTOR('',#14981,10.);
#3470=VECTOR('',#14984,10.);
#3471=VECTOR('',#14985,10.);
#3472=VECTOR('',#14986,10.);
#3473=VECTOR('',#14991,10.);
#3474=VECTOR('',#14994,10.);
#3475=VECTOR('',#14997,10.);
#3476=VECTOR('',#14998,10.);
#3477=VECTOR('',#14999,10.);
#3478=VECTOR('',#15004,10.);
#3479=VECTOR('',#15007,10.);
#3480=VECTOR('',#15010,10.);
#3481=VECTOR('',#15011,10.);
#3482=VECTOR('',#15012,10.);
#3483=VECTOR('',#15017,10.);
#3484=VECTOR('',#15020,10.);
#3485=VECTOR('',#15023,10.);
#3486=VECTOR('',#15024,10.);
#3487=VECTOR('',#15025,10.);
#3488=VECTOR('',#15030,10.);
#3489=VECTOR('',#15033,10.);
#3490=VECTOR('',#15036,10.);
#3491=VECTOR('',#15037,10.);
#3492=VECTOR('',#15038,10.);
#3493=VECTOR('',#15043,10.);
#3494=VECTOR('',#15046,10.);
#3495=VECTOR('',#15049,10.);
#3496=VECTOR('',#15050,10.);
#3497=VECTOR('',#15051,10.);
#3498=VECTOR('',#15056,10.);
#3499=VECTOR('',#15059,10.);
#3500=VECTOR('',#15062,10.);
#3501=VECTOR('',#15063,10.);
#3502=VECTOR('',#15064,10.);
#3503=VECTOR('',#15069,10.);
#3504=VECTOR('',#15072,10.);
#3505=VECTOR('',#15075,10.);
#3506=VECTOR('',#15076,10.);
#3507=VECTOR('',#15077,10.);
#3508=VECTOR('',#15082,10.);
#3509=VECTOR('',#15085,10.);
#3510=VECTOR('',#15088,10.);
#3511=VECTOR('',#15089,10.);
#3512=VECTOR('',#15090,10.);
#3513=VECTOR('',#15095,10.);
#3514=VECTOR('',#15098,10.);
#3515=VECTOR('',#15101,10.);
#3516=VECTOR('',#15102,10.);
#3517=VECTOR('',#15103,10.);
#3518=VECTOR('',#15108,10.);
#3519=VECTOR('',#15111,10.);
#3520=VECTOR('',#15114,10.);
#3521=VECTOR('',#15115,10.);
#3522=VECTOR('',#15116,10.);
#3523=VECTOR('',#15121,10.);
#3524=VECTOR('',#15124,10.);
#3525=VECTOR('',#15127,10.);
#3526=VECTOR('',#15128,10.);
#3527=VECTOR('',#15129,10.);
#3528=VECTOR('',#15134,10.);
#3529=VECTOR('',#15137,10.);
#3530=VECTOR('',#15140,10.);
#3531=VECTOR('',#15141,10.);
#3532=VECTOR('',#15142,10.);
#3533=VECTOR('',#15147,10.);
#3534=VECTOR('',#15150,10.);
#3535=VECTOR('',#15153,10.);
#3536=VECTOR('',#15154,10.);
#3537=VECTOR('',#15155,10.);
#3538=VECTOR('',#15160,10.);
#3539=VECTOR('',#15163,10.);
#3540=VECTOR('',#15166,10.);
#3541=VECTOR('',#15167,10.);
#3542=VECTOR('',#15168,10.);
#3543=VECTOR('',#15173,10.);
#3544=VECTOR('',#15176,10.);
#3545=VECTOR('',#15179,10.);
#3546=VECTOR('',#15180,10.);
#3547=VECTOR('',#15181,10.);
#3548=VECTOR('',#15186,10.);
#3549=VECTOR('',#15189,10.);
#3550=VECTOR('',#15192,10.);
#3551=VECTOR('',#15193,10.);
#3552=VECTOR('',#15194,10.);
#3553=VECTOR('',#15199,10.);
#3554=VECTOR('',#15202,10.);
#3555=VECTOR('',#15205,10.);
#3556=VECTOR('',#15206,10.);
#3557=VECTOR('',#15207,10.);
#3558=VECTOR('',#15212,10.);
#3559=VECTOR('',#15215,10.);
#3560=VECTOR('',#15218,10.);
#3561=VECTOR('',#15219,10.);
#3562=VECTOR('',#15220,10.);
#3563=VECTOR('',#15225,10.);
#3564=VECTOR('',#15228,10.);
#3565=VECTOR('',#15231,10.);
#3566=VECTOR('',#15232,10.);
#3567=VECTOR('',#15233,10.);
#3568=VECTOR('',#15238,10.);
#3569=VECTOR('',#15241,10.);
#3570=VECTOR('',#15244,10.);
#3571=VECTOR('',#15245,10.);
#3572=VECTOR('',#15246,10.);
#3573=VECTOR('',#15251,10.);
#3574=VECTOR('',#15254,10.);
#3575=VECTOR('',#15257,10.);
#3576=VECTOR('',#15258,10.);
#3577=VECTOR('',#15259,10.);
#3578=VECTOR('',#15264,10.);
#3579=VECTOR('',#15267,10.);
#3580=VECTOR('',#15270,10.);
#3581=VECTOR('',#15271,10.);
#3582=VECTOR('',#15272,10.);
#3583=VECTOR('',#15277,10.);
#3584=VECTOR('',#15280,10.);
#3585=VECTOR('',#15283,10.);
#3586=VECTOR('',#15284,10.);
#3587=VECTOR('',#15285,10.);
#3588=VECTOR('',#15290,10.);
#3589=VECTOR('',#15293,10.);
#3590=VECTOR('',#15296,10.);
#3591=VECTOR('',#15297,10.);
#3592=VECTOR('',#15298,10.);
#3593=VECTOR('',#15303,10.);
#3594=VECTOR('',#15306,10.);
#3595=VECTOR('',#15309,10.);
#3596=VECTOR('',#15310,10.);
#3597=VECTOR('',#15311,10.);
#3598=VECTOR('',#15316,10.);
#3599=VECTOR('',#15319,10.);
#3600=VECTOR('',#15322,10.);
#3601=VECTOR('',#15323,10.);
#3602=VECTOR('',#15324,10.);
#3603=VECTOR('',#15329,10.);
#3604=VECTOR('',#15332,10.);
#3605=VECTOR('',#15335,10.);
#3606=VECTOR('',#15336,10.);
#3607=VECTOR('',#15337,10.);
#3608=VECTOR('',#15342,10.);
#3609=VECTOR('',#15345,10.);
#3610=VECTOR('',#15348,10.);
#3611=VECTOR('',#15349,10.);
#3612=VECTOR('',#15350,10.);
#3613=VECTOR('',#15355,10.);
#3614=VECTOR('',#15358,10.);
#3615=VECTOR('',#15361,10.);
#3616=VECTOR('',#15362,10.);
#3617=VECTOR('',#15363,10.);
#3618=VECTOR('',#15368,10.);
#3619=VECTOR('',#15371,10.);
#3620=VECTOR('',#15374,10.);
#3621=VECTOR('',#15375,10.);
#3622=VECTOR('',#15376,10.);
#3623=VECTOR('',#15381,10.);
#3624=VECTOR('',#15384,10.);
#3625=VECTOR('',#15387,10.);
#3626=VECTOR('',#15388,10.);
#3627=VECTOR('',#15389,10.);
#3628=VECTOR('',#15394,10.);
#3629=VECTOR('',#15397,10.);
#3630=VECTOR('',#15400,10.);
#3631=VECTOR('',#15401,10.);
#3632=VECTOR('',#15402,10.);
#3633=VECTOR('',#15407,10.);
#3634=VECTOR('',#15410,10.);
#3635=VECTOR('',#15413,10.);
#3636=VECTOR('',#15414,10.);
#3637=VECTOR('',#15415,10.);
#3638=VECTOR('',#15420,10.);
#3639=VECTOR('',#15423,10.);
#3640=VECTOR('',#15426,10.);
#3641=VECTOR('',#15427,10.);
#3642=VECTOR('',#15428,10.);
#3643=VECTOR('',#15429,10.);
#3644=VECTOR('',#15436,10.);
#3645=VECTOR('',#15437,10.);
#3646=VECTOR('',#15444,10.);
#3647=VECTOR('',#15445,10.);
#3648=VECTOR('',#15452,10.);
#3649=VECTOR('',#15453,10.);
#3650=VECTOR('',#15460,10.);
#3651=VECTOR('',#15461,10.);
#3652=VECTOR('',#15468,10.);
#3653=VECTOR('',#15469,10.);
#3654=VECTOR('',#15476,10.);
#3655=VECTOR('',#15477,10.);
#3656=VECTOR('',#15484,10.);
#3657=VECTOR('',#15485,10.);
#3658=VECTOR('',#15492,10.);
#3659=VECTOR('',#15493,10.);
#3660=VECTOR('',#15500,10.);
#3661=VECTOR('',#15501,10.);
#3662=VECTOR('',#15508,10.);
#3663=VECTOR('',#15509,10.);
#3664=VECTOR('',#15516,10.);
#3665=VECTOR('',#15517,10.);
#3666=VECTOR('',#15524,10.);
#3667=VECTOR('',#15525,10.);
#3668=VECTOR('',#15532,10.);
#3669=VECTOR('',#15533,10.);
#3670=VECTOR('',#15540,10.);
#3671=VECTOR('',#15541,10.);
#3672=VECTOR('',#15548,10.);
#3673=VECTOR('',#15549,10.);
#3674=VECTOR('',#15556,10.);
#3675=VECTOR('',#15557,10.);
#3676=VECTOR('',#15564,10.);
#3677=VECTOR('',#15565,10.);
#3678=VECTOR('',#15572,10.);
#3679=VECTOR('',#15573,10.);
#3680=VECTOR('',#15580,10.);
#3681=VECTOR('',#15621,10.);
#3682=VECTOR('',#15624,10.);
#3683=VECTOR('',#15637,10.);
#3684=VECTOR('',#15640,10.);
#3685=VECTOR('',#15683,10.);
#3686=VECTOR('',#15722,10.);
#3687=VECTOR('',#15725,10.);
#3688=VECTOR('',#15728,10.);
#3689=VECTOR('',#15729,10.);
#3690=VECTOR('',#15732,10.);
#3691=VECTOR('',#15733,10.);
#3692=VECTOR('',#15736,10.);
#3693=VECTOR('',#15745,7.50000000000001);
#3694=VECTOR('',#15752,7.50000000000001);
#3695=VECTOR('',#15763,10.);
#3696=VECTOR('',#15766,10.);
#3697=VECTOR('',#15769,10.);
#3698=VECTOR('',#15770,10.);
#3699=VECTOR('',#15771,10.);
#3700=VECTOR('',#15776,10.);
#3701=VECTOR('',#15779,10.);
#3702=VECTOR('',#15782,10.);
#3703=VECTOR('',#15783,10.);
#3704=VECTOR('',#15784,10.);
#3705=VECTOR('',#15789,10.);
#3706=VECTOR('',#15792,10.);
#3707=VECTOR('',#15795,10.);
#3708=VECTOR('',#15796,10.);
#3709=VECTOR('',#15797,10.);
#3710=VECTOR('',#15802,10.);
#3711=VECTOR('',#15805,10.);
#3712=VECTOR('',#15808,10.);
#3713=VECTOR('',#15809,10.);
#3714=VECTOR('',#15810,10.);
#3715=VECTOR('',#15815,10.);
#3716=VECTOR('',#15818,10.);
#3717=VECTOR('',#15821,10.);
#3718=VECTOR('',#15822,10.);
#3719=VECTOR('',#15823,10.);
#3720=VECTOR('',#15828,10.);
#3721=VECTOR('',#15831,10.);
#3722=VECTOR('',#15834,10.);
#3723=VECTOR('',#15835,10.);
#3724=VECTOR('',#15836,10.);
#3725=VECTOR('',#15841,10.);
#3726=VECTOR('',#15844,10.);
#3727=VECTOR('',#15847,10.);
#3728=VECTOR('',#15848,10.);
#3729=VECTOR('',#15849,10.);
#3730=VECTOR('',#15854,10.);
#3731=VECTOR('',#15857,10.);
#3732=VECTOR('',#15860,10.);
#3733=VECTOR('',#15861,10.);
#3734=VECTOR('',#15862,10.);
#3735=VECTOR('',#15867,10.);
#3736=VECTOR('',#15870,10.);
#3737=VECTOR('',#15873,10.);
#3738=VECTOR('',#15874,10.);
#3739=VECTOR('',#15875,10.);
#3740=VECTOR('',#15880,10.);
#3741=VECTOR('',#15883,10.);
#3742=VECTOR('',#15886,10.);
#3743=VECTOR('',#15887,10.);
#3744=VECTOR('',#15888,10.);
#3745=VECTOR('',#15893,10.);
#3746=VECTOR('',#15896,10.);
#3747=VECTOR('',#15899,10.);
#3748=VECTOR('',#15900,10.);
#3749=VECTOR('',#15901,10.);
#3750=VECTOR('',#15906,10.);
#3751=VECTOR('',#15909,10.);
#3752=VECTOR('',#15912,10.);
#3753=VECTOR('',#15913,10.);
#3754=VECTOR('',#15914,10.);
#3755=VECTOR('',#15919,10.);
#3756=VECTOR('',#15922,10.);
#3757=VECTOR('',#15925,10.);
#3758=VECTOR('',#15926,10.);
#3759=VECTOR('',#15927,10.);
#3760=VECTOR('',#15932,10.);
#3761=VECTOR('',#15935,10.);
#3762=VECTOR('',#15938,10.);
#3763=VECTOR('',#15939,10.);
#3764=VECTOR('',#15940,10.);
#3765=VECTOR('',#15945,10.);
#3766=VECTOR('',#15948,10.);
#3767=VECTOR('',#15951,10.);
#3768=VECTOR('',#15952,10.);
#3769=VECTOR('',#15953,10.);
#3770=VECTOR('',#15958,10.);
#3771=VECTOR('',#15961,10.);
#3772=VECTOR('',#15964,10.);
#3773=VECTOR('',#15965,10.);
#3774=VECTOR('',#15966,10.);
#3775=VECTOR('',#15971,10.);
#3776=VECTOR('',#15974,10.);
#3777=VECTOR('',#15977,10.);
#3778=VECTOR('',#15978,10.);
#3779=VECTOR('',#15979,10.);
#3780=VECTOR('',#15984,10.);
#3781=VECTOR('',#15987,10.);
#3782=VECTOR('',#15990,10.);
#3783=VECTOR('',#15991,10.);
#3784=VECTOR('',#15992,10.);
#3785=VECTOR('',#15993,10.);
#3786=VECTOR('',#16000,10.);
#3787=VECTOR('',#16001,10.);
#3788=VECTOR('',#16008,10.);
#3789=VECTOR('',#16009,10.);
#3790=VECTOR('',#16016,10.);
#3791=VECTOR('',#16017,10.);
#3792=VECTOR('',#16024,10.);
#3793=VECTOR('',#16025,10.);
#3794=VECTOR('',#16032,10.);
#3795=VECTOR('',#16033,10.);
#3796=VECTOR('',#16040,10.);
#3797=VECTOR('',#16041,10.);
#3798=VECTOR('',#16048,10.);
#3799=VECTOR('',#16049,10.);
#3800=VECTOR('',#16056,10.);
#3801=VECTOR('',#16057,10.);
#3802=VECTOR('',#16064,10.);
#3803=VECTOR('',#16085,10.);
#3804=VECTOR('',#16088,10.);
#3805=VECTOR('',#16101,10.);
#3806=VECTOR('',#16104,10.);
#3807=VECTOR('',#16127,10.);
#3808=VECTOR('',#16146,10.);
#3809=VECTOR('',#16149,10.);
#3810=VECTOR('',#16152,10.);
#3811=VECTOR('',#16153,10.);
#3812=VECTOR('',#16156,10.);
#3813=VECTOR('',#16157,10.);
#3814=VECTOR('',#16160,10.);
#3815=VECTOR('',#16197,8.14999999999999);
#3816=VECTOR('',#16202,7.5);
#3817=VECTOR('',#16205,7.5);
#3818=VECTOR('',#16210,12.4653846153846);
#3819=VECTOR('',#16217,12.4653846153846);
#3820=VECTOR('',#16290,17.6897435897436);
#3821=VECTOR('',#16297,16.2686153846154);
#3822=VECTOR('',#16300,16.0346153846154);
#3823=VECTOR('',#16311,16.0346153846154);
#3824=VECTOR('',#16314,16.2686153846154);
#3825=VECTOR('',#16321,17.6897435897436);
#3826=VECTOR('',#16328,20.35);
#3827=VECTOR('',#16335,21.);
#3828=VECTOR('',#16342,21.);
#3829=VECTOR('',#16837,8.14999999999999);
#3830=VECTOR('',#16842,7.5);
#3831=VECTOR('',#16845,7.5);
#3832=VECTOR('',#16850,12.4653846153846);
#3833=VECTOR('',#16857,12.4653846153846);
#3834=VECTOR('',#16930,17.6897435897436);
#3835=VECTOR('',#16937,16.2686153846154);
#3836=VECTOR('',#16940,16.0346153846154);
#3837=VECTOR('',#16951,16.0346153846154);
#3838=VECTOR('',#16954,16.2686153846154);
#3839=VECTOR('',#16961,17.6897435897436);
#3840=VECTOR('',#16968,20.35);
#3841=VECTOR('',#16975,21.);
#3842=VECTOR('',#16982,21.);
#3843=VECTOR('',#17477,8.14999999999999);
#3844=VECTOR('',#17482,7.5);
#3845=VECTOR('',#17485,7.5);
#3846=VECTOR('',#17492,12.4653846153846);
#3847=VECTOR('',#17495,12.4653846153846);
#3848=VECTOR('',#17570,17.6897435897436);
#3849=VECTOR('',#17575,16.2686153846154);
#3850=VECTOR('',#17582,16.0346153846154);
#3851=VECTOR('',#17591,16.0346153846154);
#3852=VECTOR('',#17596,16.2686153846154);
#3853=VECTOR('',#17601,17.6897435897436);
#3854=VECTOR('',#17608,20.35);
#3855=VECTOR('',#17617,21.);
#3856=VECTOR('',#17622,21.);
#3857=VECTOR('',#18117,8.14999999999999);
#3858=VECTOR('',#18122,7.5);
#3859=VECTOR('',#18125,7.5);
#3860=VECTOR('',#18132,12.4653846153846);
#3861=VECTOR('',#18135,12.4653846153846);
#3862=VECTOR('',#18210,17.6897435897436);
#3863=VECTOR('',#18215,16.2686153846154);
#3864=VECTOR('',#18222,16.0346153846154);
#3865=VECTOR('',#18231,16.0346153846154);
#3866=VECTOR('',#18236,16.2686153846154);
#3867=VECTOR('',#18241,17.6897435897436);
#3868=VECTOR('',#18248,20.35);
#3869=VECTOR('',#18257,21.);
#3870=VECTOR('',#18262,21.);
#3871=VECTOR('',#18729,21.);
#3872=VECTOR('',#18734,10.);
#3873=VECTOR('',#18735,10.);
#3874=VECTOR('',#18736,10.);
#3875=VECTOR('',#18737,10.);
#3876=VECTOR('',#18742,21.);
#3877=VECTOR('',#18747,10.);
#3878=VECTOR('',#18748,10.);
#3879=VECTOR('',#18749,10.);
#3880=VECTOR('',#18750,10.);
#3881=VECTOR('',#18753,10.);
#3882=VECTOR('',#18754,10.);
#3883=VECTOR('',#18757,10.);
#3884=VECTOR('',#18760,10.);
#3885=VECTOR('',#18769,21.);
#3886=VECTOR('',#18776,21.);
#3887=VECTOR('',#18781,10.);
#3888=VECTOR('',#18782,10.);
#3889=VECTOR('',#18783,10.);
#3890=VECTOR('',#18784,10.);
#3891=VECTOR('',#18787,10.);
#3892=VECTOR('',#18788,10.);
#3893=VECTOR('',#18789,10.);
#3894=VECTOR('',#18792,10.);
#3895=VECTOR('',#18793,10.);
#3896=VECTOR('',#18796,10.);
#3897=VECTOR('',#18797,10.);
#3898=VECTOR('',#18800,10.);
#3899=CIRCLE('',#13187,7.5);
#3900=CIRCLE('',#13188,7.5);
#3901=CIRCLE('',#13190,7.5);
#3902=CIRCLE('',#13191,7.5);
#3903=CIRCLE('',#13195,1.);
#3904=CIRCLE('',#13196,1.);
#3905=CIRCLE('',#13199,1.);
#3906=CIRCLE('',#13200,1.);
#3907=CIRCLE('',#13203,1.);
#3908=CIRCLE('',#13204,1.);
#3909=CIRCLE('',#13207,1.);
#3910=CIRCLE('',#13208,1.);
#3911=CIRCLE('',#13211,1.);
#3912=CIRCLE('',#13212,1.);
#3913=CIRCLE('',#13215,1.);
#3914=CIRCLE('',#13216,1.);
#3915=CIRCLE('',#13219,1.);
#3916=CIRCLE('',#13220,1.);
#3917=CIRCLE('',#13223,1.);
#3918=CIRCLE('',#13224,1.);
#3919=CIRCLE('',#13227,1.);
#3920=CIRCLE('',#13228,1.);
#3921=CIRCLE('',#13231,1.);
#3922=CIRCLE('',#13232,1.);
#3923=CIRCLE('',#13235,1.);
#3924=CIRCLE('',#13236,1.);
#3925=CIRCLE('',#13239,1.);
#3926=CIRCLE('',#13240,1.);
#3927=CIRCLE('',#13243,1.);
#3928=CIRCLE('',#13244,1.);
#3929=CIRCLE('',#13247,1.);
#3930=CIRCLE('',#13248,1.);
#3931=CIRCLE('',#13251,1.);
#3932=CIRCLE('',#13252,1.);
#3933=CIRCLE('',#13255,1.);
#3934=CIRCLE('',#13256,1.);
#3935=CIRCLE('',#13259,1.);
#3936=CIRCLE('',#13260,1.);
#3937=CIRCLE('',#13263,1.);
#3938=CIRCLE('',#13264,1.);
#3939=CIRCLE('',#13267,1.);
#3940=CIRCLE('',#13268,1.);
#3941=CIRCLE('',#13271,1.);
#3942=CIRCLE('',#13272,1.);
#3943=CIRCLE('',#13275,1.);
#3944=CIRCLE('',#13276,1.);
#3945=CIRCLE('',#13279,1.);
#3946=CIRCLE('',#13280,1.);
#3947=CIRCLE('',#13283,1.);
#3948=CIRCLE('',#13284,1.);
#3949=CIRCLE('',#13287,1.);
#3950=CIRCLE('',#13288,1.);
#3951=CIRCLE('',#13291,1.);
#3952=CIRCLE('',#13292,1.);
#3953=CIRCLE('',#13295,1.);
#3954=CIRCLE('',#13296,1.);
#3955=CIRCLE('',#13299,1.);
#3956=CIRCLE('',#13300,1.);
#3957=CIRCLE('',#13303,1.);
#3958=CIRCLE('',#13304,1.);
#3959=CIRCLE('',#13307,1.);
#3960=CIRCLE('',#13308,1.);
#3961=CIRCLE('',#13311,1.);
#3962=CIRCLE('',#13312,1.);
#3963=CIRCLE('',#13315,1.);
#3964=CIRCLE('',#13316,1.);
#3965=CIRCLE('',#13319,1.);
#3966=CIRCLE('',#13320,1.);
#3967=CIRCLE('',#13323,1.);
#3968=CIRCLE('',#13324,1.);
#3969=CIRCLE('',#13327,1.);
#3970=CIRCLE('',#13328,1.);
#3971=CIRCLE('',#13331,1.);
#3972=CIRCLE('',#13332,1.);
#3973=CIRCLE('',#13335,1.);
#3974=CIRCLE('',#13336,1.);
#3975=CIRCLE('',#13339,1.);
#3976=CIRCLE('',#13340,1.);
#3977=CIRCLE('',#13343,1.);
#3978=CIRCLE('',#13344,1.);
#3979=CIRCLE('',#13347,43.9999999999887);
#3980=CIRCLE('',#13348,43.9999999999887);
#3981=CIRCLE('',#13350,43.9999999999887);
#3982=CIRCLE('',#13351,43.9999999999887);
#3983=CIRCLE('',#13353,43.9999999999887);
#3984=CIRCLE('',#13354,43.9999999999887);
#3985=CIRCLE('',#13356,43.9999999999887);
#3986=CIRCLE('',#13357,43.9999999999887);
#3987=CIRCLE('',#13359,43.9999999999887);
#3988=CIRCLE('',#13360,43.9999999999887);
#3989=CIRCLE('',#13362,43.9999999999887);
#3990=CIRCLE('',#13363,43.9999999999887);
#3991=CIRCLE('',#13365,43.9999999999887);
#3992=CIRCLE('',#13366,43.9999999999887);
#3993=CIRCLE('',#13368,43.9999999999887);
#3994=CIRCLE('',#13369,43.9999999999887);
#3995=CIRCLE('',#13371,43.9999999999887);
#3996=CIRCLE('',#13372,43.9999999999887);
#3997=CIRCLE('',#13374,43.9999999999887);
#3998=CIRCLE('',#13375,43.9999999999887);
#3999=CIRCLE('',#13377,43.9999999999887);
#4000=CIRCLE('',#13378,43.9999999999887);
#4001=CIRCLE('',#13380,43.9999999999887);
#4002=CIRCLE('',#13381,43.9999999999887);
#4003=CIRCLE('',#13383,43.9999999999887);
#4004=CIRCLE('',#13384,43.9999999999887);
#4005=CIRCLE('',#13386,43.9999999999887);
#4006=CIRCLE('',#13387,43.9999999999887);
#4007=CIRCLE('',#13389,43.9999999999887);
#4008=CIRCLE('',#13390,43.9999999999887);
#4009=CIRCLE('',#13392,43.9999999999887);
#4010=CIRCLE('',#13393,43.9999999999887);
#4011=CIRCLE('',#13395,43.9999999999887);
#4012=CIRCLE('',#13396,43.9999999999887);
#4013=CIRCLE('',#13398,43.9999999999887);
#4014=CIRCLE('',#13399,43.9999999999887);
#4015=CIRCLE('',#13401,43.9999999999887);
#4016=CIRCLE('',#13402,43.9999999999887);
#4017=CIRCLE('',#13404,35.372);
#4018=CIRCLE('',#13405,35.372);
#4019=CIRCLE('',#13406,35.372);
#4020=CIRCLE('',#13407,35.372);
#4021=CIRCLE('',#13408,35.372);
#4022=CIRCLE('',#13409,35.372);
#4023=CIRCLE('',#13410,35.372);
#4024=CIRCLE('',#13411,35.372);
#4025=CIRCLE('',#13412,35.372);
#4026=CIRCLE('',#13413,35.372);
#4027=CIRCLE('',#13414,35.372);
#4028=CIRCLE('',#13415,35.372);
#4029=CIRCLE('',#13416,35.372);
#4030=CIRCLE('',#13417,35.372);
#4031=CIRCLE('',#13418,35.372);
#4032=CIRCLE('',#13419,35.372);
#4033=CIRCLE('',#13420,35.372);
#4034=CIRCLE('',#13421,35.372);
#4035=CIRCLE('',#13422,1.);
#4036=CIRCLE('',#13423,43.9999999999887);
#4037=CIRCLE('',#13424,1.);
#4038=CIRCLE('',#13425,35.372);
#4039=CIRCLE('',#13426,35.372);
#4040=CIRCLE('',#13428,35.372);
#4041=CIRCLE('',#13429,1.);
#4042=CIRCLE('',#13430,43.9999999999887);
#4043=CIRCLE('',#13431,1.);
#4044=CIRCLE('',#13432,35.372);
#4045=CIRCLE('',#13433,35.372);
#4046=CIRCLE('',#13434,35.372);
#4047=CIRCLE('',#13435,35.372);
#4048=CIRCLE('',#13436,35.372);
#4049=CIRCLE('',#13437,35.372);
#4050=CIRCLE('',#13438,35.372);
#4051=CIRCLE('',#13439,35.372);
#4052=CIRCLE('',#13440,35.372);
#4053=CIRCLE('',#13441,35.372);
#4054=CIRCLE('',#13442,35.372);
#4055=CIRCLE('',#13443,35.372);
#4056=CIRCLE('',#13444,35.372);
#4057=CIRCLE('',#13445,35.372);
#4058=CIRCLE('',#13446,35.372);
#4059=CIRCLE('',#13447,35.372);
#4060=CIRCLE('',#13448,35.372);
#4061=CIRCLE('',#13449,35.372);
#4062=CIRCLE('',#13450,35.372);
#4063=CIRCLE('',#13478,7.5);
#4064=CIRCLE('',#13479,7.50000000000001);
#4065=CIRCLE('',#13481,7.50000000000001);
#4066=CIRCLE('',#13482,7.5);
#4067=CIRCLE('',#13486,1.);
#4068=CIRCLE('',#13487,1.);
#4069=CIRCLE('',#13490,1.);
#4070=CIRCLE('',#13491,1.);
#4071=CIRCLE('',#13494,1.);
#4072=CIRCLE('',#13495,1.);
#4073=CIRCLE('',#13498,1.);
#4074=CIRCLE('',#13499,1.);
#4075=CIRCLE('',#13502,1.);
#4076=CIRCLE('',#13503,1.);
#4077=CIRCLE('',#13506,1.);
#4078=CIRCLE('',#13507,1.);
#4079=CIRCLE('',#13510,1.);
#4080=CIRCLE('',#13511,1.);
#4081=CIRCLE('',#13514,1.);
#4082=CIRCLE('',#13515,1.);
#4083=CIRCLE('',#13518,1.);
#4084=CIRCLE('',#13519,1.);
#4085=CIRCLE('',#13522,1.);
#4086=CIRCLE('',#13523,1.);
#4087=CIRCLE('',#13526,1.);
#4088=CIRCLE('',#13527,1.);
#4089=CIRCLE('',#13530,1.);
#4090=CIRCLE('',#13531,1.);
#4091=CIRCLE('',#13534,1.);
#4092=CIRCLE('',#13535,1.);
#4093=CIRCLE('',#13538,1.);
#4094=CIRCLE('',#13539,1.);
#4095=CIRCLE('',#13542,1.);
#4096=CIRCLE('',#13543,1.);
#4097=CIRCLE('',#13546,1.);
#4098=CIRCLE('',#13547,1.);
#4099=CIRCLE('',#13550,1.);
#4100=CIRCLE('',#13551,1.);
#4101=CIRCLE('',#13554,1.);
#4102=CIRCLE('',#13555,1.);
#4103=CIRCLE('',#13558,23.9999999999999);
#4104=CIRCLE('',#13559,23.9999999999999);
#4105=CIRCLE('',#13561,23.9999999999999);
#4106=CIRCLE('',#13562,23.9999999999999);
#4107=CIRCLE('',#13564,23.9999999999999);
#4108=CIRCLE('',#13565,23.9999999999999);
#4109=CIRCLE('',#13567,23.9999999999999);
#4110=CIRCLE('',#13568,23.9999999999999);
#4111=CIRCLE('',#13570,23.9999999999999);
#4112=CIRCLE('',#13571,23.9999999999999);
#4113=CIRCLE('',#13573,23.9999999999999);
#4114=CIRCLE('',#13574,23.9999999999999);
#4115=CIRCLE('',#13576,23.9999999999999);
#4116=CIRCLE('',#13577,23.9999999999999);
#4117=CIRCLE('',#13579,23.9999999999999);
#4118=CIRCLE('',#13580,23.9999999999999);
#4119=CIRCLE('',#13582,23.9999999999999);
#4120=CIRCLE('',#13583,23.9999999999999);
#4121=CIRCLE('',#13585,15.372);
#4122=CIRCLE('',#13586,15.372);
#4123=CIRCLE('',#13587,15.372);
#4124=CIRCLE('',#13588,15.372);
#4125=CIRCLE('',#13589,15.372);
#4126=CIRCLE('',#13590,15.372);
#4127=CIRCLE('',#13591,15.372);
#4128=CIRCLE('',#13592,15.372);
#4129=CIRCLE('',#13593,1.);
#4130=CIRCLE('',#13594,23.9999999999999);
#4131=CIRCLE('',#13595,1.);
#4132=CIRCLE('',#13596,15.372);
#4133=CIRCLE('',#13597,15.372);
#4134=CIRCLE('',#13599,15.372);
#4135=CIRCLE('',#13600,1.);
#4136=CIRCLE('',#13601,23.9999999999999);
#4137=CIRCLE('',#13602,1.);
#4138=CIRCLE('',#13603,15.372);
#4139=CIRCLE('',#13604,15.372);
#4140=CIRCLE('',#13605,15.372);
#4141=CIRCLE('',#13606,15.372);
#4142=CIRCLE('',#13607,15.372);
#4143=CIRCLE('',#13608,15.372);
#4144=CIRCLE('',#13609,15.372);
#4145=CIRCLE('',#13610,15.372);
#4146=CIRCLE('',#13611,15.372);
#4147=CIRCLE('',#13629,12.4653846153846);
#4148=CIRCLE('',#13630,3.56616156686793);
#4149=CIRCLE('',#13631,12.4653846153846);
#4150=CIRCLE('',#13633,7.64278544417155);
#4151=CIRCLE('',#13634,7.64278544417155);
#4152=CIRCLE('',#13635,0.4875);
#4153=CIRCLE('',#13636,7.5);
#4154=CIRCLE('',#13637,7.5);
#4155=CIRCLE('',#13639,7.5);
#4156=CIRCLE('',#13640,7.5);
#4157=CIRCLE('',#13641,0.4875);
#4158=CIRCLE('',#13642,7.64278544417155);
#4159=CIRCLE('',#13644,8.14999999999999);
#4160=CIRCLE('',#13647,8.14999999999999);
#4161=CIRCLE('',#13649,12.4653846153846);
#4162=CIRCLE('',#13651,12.4653846153846);
#4163=CIRCLE('',#13655,3.56616156686793);
#4164=CIRCLE('',#13657,3.56616156686793);
#4165=CIRCLE('',#13659,3.56616156686793);
#4166=CIRCLE('',#13661,3.56616156686793);
#4167=CIRCLE('',#13663,3.56616156686793);
#4168=CIRCLE('',#13665,3.56616156686793);
#4169=CIRCLE('',#13667,3.56616156686793);
#4170=CIRCLE('',#13669,16.3271153846154);
#4171=CIRCLE('',#13670,0.0585);
#4172=CIRCLE('',#13671,16.2686153846154);
#4173=CIRCLE('',#13672,16.2686153846154);
#4174=CIRCLE('',#13674,16.0346153846154);
#4175=CIRCLE('',#13675,0.0585);
#4176=CIRCLE('',#13676,16.0931153846154);
#4177=CIRCLE('',#13678,16.3271153846154);
#4178=CIRCLE('',#13679,0.0585);
#4179=CIRCLE('',#13680,16.2686153846154);
#4180=CIRCLE('',#13682,16.0346153846154);
#4181=CIRCLE('',#13683,16.0346153846154);
#4182=CIRCLE('',#13684,0.0585);
#4183=CIRCLE('',#13685,16.0931153846154);
#4184=CIRCLE('',#13687,17.6897435897436);
#4185=CIRCLE('',#13688,17.6897435897436);
#4186=CIRCLE('',#13690,16.2686153846154);
#4187=CIRCLE('',#13692,16.0346153846154);
#4188=CIRCLE('',#13694,3.56616156686793);
#4189=CIRCLE('',#13695,16.0346153846154);
#4190=CIRCLE('',#13698,16.2686153846154);
#4191=CIRCLE('',#13700,17.6897435897436);
#4192=CIRCLE('',#13701,17.6897435897436);
#4193=CIRCLE('',#13703,21.);
#4194=CIRCLE('',#13704,20.35);
#4195=CIRCLE('',#13706,21.);
#4196=CIRCLE('',#13707,20.35);
#4197=CIRCLE('',#13708,21.);
#4198=CIRCLE('',#13717,3.96060240207311);
#4199=CIRCLE('',#13718,1.69469015025);
#4200=CIRCLE('',#13719,3.96060240207311);
#4201=CIRCLE('',#13721,3.39763111739558);
#4202=CIRCLE('',#13722,3.56616156686792);
#4203=CIRCLE('',#13723,3.39763111739558);
#4204=CIRCLE('',#13724,3.39763111739558);
#4205=CIRCLE('',#13725,3.39763111739558);
#4206=CIRCLE('',#13726,3.39763111739558);
#4207=CIRCLE('',#13727,3.39763111739558);
#4208=CIRCLE('',#13728,3.45272288248773);
#4209=CIRCLE('',#13729,3.45272288248773);
#4210=CIRCLE('',#13731,3.96060240207311);
#4211=CIRCLE('',#13732,1.69469015025);
#4212=CIRCLE('',#13733,3.96060240207311);
#4213=CIRCLE('',#13735,3.39763111739558);
#4214=CIRCLE('',#13736,3.56616156686792);
#4215=CIRCLE('',#13737,3.39763111739558);
#4216=CIRCLE('',#13738,3.39763111739558);
#4217=CIRCLE('',#13739,3.39763111739558);
#4218=CIRCLE('',#13740,3.39763111739558);
#4219=CIRCLE('',#13741,3.39763111739558);
#4220=CIRCLE('',#13742,3.45272288248773);
#4221=CIRCLE('',#13743,3.45272288248773);
#4222=CIRCLE('',#13745,3.96060240207311);
#4223=CIRCLE('',#13746,1.69469015025);
#4224=CIRCLE('',#13747,3.96060240207311);
#4225=CIRCLE('',#13749,3.39763111739558);
#4226=CIRCLE('',#13750,3.56616156686792);
#4227=CIRCLE('',#13751,3.39763111739558);
#4228=CIRCLE('',#13752,3.39763111739558);
#4229=CIRCLE('',#13753,3.39763111739558);
#4230=CIRCLE('',#13754,3.39763111739558);
#4231=CIRCLE('',#13755,3.39763111739558);
#4232=CIRCLE('',#13756,3.45272288248773);
#4233=CIRCLE('',#13757,3.45272288248773);
#4234=CIRCLE('',#13759,3.96060240207311);
#4235=CIRCLE('',#13760,1.69469015025);
#4236=CIRCLE('',#13761,3.96060240207311);
#4237=CIRCLE('',#13763,3.39763111739558);
#4238=CIRCLE('',#13764,3.56616156686792);
#4239=CIRCLE('',#13765,3.39763111739558);
#4240=CIRCLE('',#13766,3.39763111739558);
#4241=CIRCLE('',#13767,3.39763111739558);
#4242=CIRCLE('',#13768,3.39763111739558);
#4243=CIRCLE('',#13769,3.39763111739558);
#4244=CIRCLE('',#13770,3.45272288248773);
#4245=CIRCLE('',#13771,3.45272288248773);
#4246=CIRCLE('',#13773,3.96060240207311);
#4247=CIRCLE('',#13774,1.69469015025);
#4248=CIRCLE('',#13775,3.96060240207311);
#4249=CIRCLE('',#13777,3.39763111739558);
#4250=CIRCLE('',#13778,3.56616156686792);
#4251=CIRCLE('',#13779,3.39763111739558);
#4252=CIRCLE('',#13780,3.39763111739558);
#4253=CIRCLE('',#13781,3.39763111739558);
#4254=CIRCLE('',#13782,3.39763111739558);
#4255=CIRCLE('',#13783,3.39763111739558);
#4256=CIRCLE('',#13784,3.45272288248773);
#4257=CIRCLE('',#13785,3.45272288248773);
#4258=CIRCLE('',#13787,3.96060240207311);
#4259=CIRCLE('',#13788,1.69469015025);
#4260=CIRCLE('',#13789,3.96060240207311);
#4261=CIRCLE('',#13791,3.39763111739558);
#4262=CIRCLE('',#13792,3.39763111739558);
#4263=CIRCLE('',#13793,3.39763111739558);
#4264=CIRCLE('',#13794,3.56616156686792);
#4265=CIRCLE('',#13795,3.39763111739558);
#4266=CIRCLE('',#13796,3.39763111739558);
#4267=CIRCLE('',#13797,3.39763111739558);
#4268=CIRCLE('',#13798,3.45272288248773);
#4269=CIRCLE('',#13799,3.45272288248773);
#4270=CIRCLE('',#13801,3.39763111739558);
#4271=CIRCLE('',#13802,3.56616156686792);
#4272=CIRCLE('',#13803,3.39763111739558);
#4273=CIRCLE('',#13804,3.39763111739558);
#4274=CIRCLE('',#13805,3.39763111739558);
#4275=CIRCLE('',#13806,3.39763111739558);
#4276=CIRCLE('',#13807,3.39763111739558);
#4277=CIRCLE('',#13808,3.45272288248773);
#4278=CIRCLE('',#13809,3.45272288248773);
#4279=CIRCLE('',#13811,3.96060240207311);
#4280=CIRCLE('',#13812,1.69469015025);
#4281=CIRCLE('',#13813,3.96060240207311);
#4282=CIRCLE('',#13815,14.25);
#4283=CIRCLE('',#13816,14.25);
#4284=CIRCLE('',#13818,15.1423076923077);
#4285=CIRCLE('',#13819,15.1423076923077);
#4286=CIRCLE('',#13825,14.25);
#4287=CIRCLE('',#13826,15.1423076923077);
#4288=CIRCLE('',#13828,14.25);
#4289=CIRCLE('',#13829,15.1423076923077);
#4290=CIRCLE('',#13835,14.25);
#4291=CIRCLE('',#13836,15.1423076923077);
#4292=CIRCLE('',#13838,14.25);
#4293=CIRCLE('',#13839,15.1423076923077);
#4294=CIRCLE('',#13843,14.25);
#4295=CIRCLE('',#13844,14.25);
#4296=CIRCLE('',#13846,15.1423076923077);
#4297=CIRCLE('',#13847,15.1423076923077);
#4298=CIRCLE('',#13853,14.25);
#4299=CIRCLE('',#13854,15.1423076923077);
#4300=CIRCLE('',#13856,14.25);
#4301=CIRCLE('',#13857,15.1423076923077);
#4302=CIRCLE('',#13861,14.25);
#4303=CIRCLE('',#13862,14.25);
#4304=CIRCLE('',#13864,15.1423076923077);
#4305=CIRCLE('',#13865,15.1423076923077);
#4306=CIRCLE('',#13871,14.25);
#4307=CIRCLE('',#13872,15.1423076923077);
#4308=CIRCLE('',#13874,14.25);
#4309=CIRCLE('',#13875,15.1423076923077);
#4310=CIRCLE('',#13879,14.25);
#4311=CIRCLE('',#13880,14.25);
#4312=CIRCLE('',#13882,15.1423076923077);
#4313=CIRCLE('',#13883,15.1423076923077);
#4314=CIRCLE('',#13889,14.25);
#4315=CIRCLE('',#13890,15.1423076923077);
#4316=CIRCLE('',#13892,14.25);
#4317=CIRCLE('',#13893,15.1423076923077);
#4318=CIRCLE('',#13897,14.25);
#4319=CIRCLE('',#13898,14.25);
#4320=CIRCLE('',#13900,15.1423076923077);
#4321=CIRCLE('',#13901,15.1423076923077);
#4322=CIRCLE('',#13907,14.25);
#4323=CIRCLE('',#13908,15.1423076923077);
#4324=CIRCLE('',#13910,14.25);
#4325=CIRCLE('',#13911,15.1423076923077);
#4326=CIRCLE('',#13915,14.25);
#4327=CIRCLE('',#13916,14.25);
#4328=CIRCLE('',#13918,15.1423076923077);
#4329=CIRCLE('',#13919,15.1423076923077);
#4330=CIRCLE('',#13925,14.25);
#4331=CIRCLE('',#13926,15.1423076923077);
#4332=CIRCLE('',#13928,14.25);
#4333=CIRCLE('',#13929,15.1423076923077);
#4334=CIRCLE('',#13933,14.25);
#4335=CIRCLE('',#13934,15.1423076923077);
#4336=CIRCLE('',#13936,14.25);
#4337=CIRCLE('',#13937,15.1423076923077);
#4338=CIRCLE('',#13942,12.4653846153846);
#4339=CIRCLE('',#13943,3.56616156686793);
#4340=CIRCLE('',#13944,12.4653846153846);
#4341=CIRCLE('',#13946,7.64278544417155);
#4342=CIRCLE('',#13947,7.64278544417155);
#4343=CIRCLE('',#13948,0.4875);
#4344=CIRCLE('',#13949,7.5);
#4345=CIRCLE('',#13950,7.5);
#4346=CIRCLE('',#13952,7.5);
#4347=CIRCLE('',#13953,7.5);
#4348=CIRCLE('',#13954,0.4875);
#4349=CIRCLE('',#13955,7.64278544417155);
#4350=CIRCLE('',#13957,8.14999999999999);
#4351=CIRCLE('',#13960,8.14999999999999);
#4352=CIRCLE('',#13962,12.4653846153846);
#4353=CIRCLE('',#13964,12.4653846153846);
#4354=CIRCLE('',#13968,3.56616156686793);
#4355=CIRCLE('',#13970,3.56616156686793);
#4356=CIRCLE('',#13972,3.56616156686793);
#4357=CIRCLE('',#13974,3.56616156686793);
#4358=CIRCLE('',#13976,3.56616156686793);
#4359=CIRCLE('',#13978,3.56616156686793);
#4360=CIRCLE('',#13980,3.56616156686793);
#4361=CIRCLE('',#13982,16.3271153846154);
#4362=CIRCLE('',#13983,0.0585);
#4363=CIRCLE('',#13984,16.2686153846154);
#4364=CIRCLE('',#13985,16.2686153846154);
#4365=CIRCLE('',#13987,16.0346153846154);
#4366=CIRCLE('',#13988,0.0585);
#4367=CIRCLE('',#13989,16.0931153846154);
#4368=CIRCLE('',#13991,16.3271153846154);
#4369=CIRCLE('',#13992,0.0585);
#4370=CIRCLE('',#13993,16.2686153846154);
#4371=CIRCLE('',#13995,16.0346153846154);
#4372=CIRCLE('',#13996,16.0346153846154);
#4373=CIRCLE('',#13997,0.0585);
#4374=CIRCLE('',#13998,16.0931153846154);
#4375=CIRCLE('',#14000,17.6897435897436);
#4376=CIRCLE('',#14001,17.6897435897436);
#4377=CIRCLE('',#14003,16.2686153846154);
#4378=CIRCLE('',#14005,16.0346153846154);
#4379=CIRCLE('',#14007,3.56616156686793);
#4380=CIRCLE('',#14008,16.0346153846154);
#4381=CIRCLE('',#14011,16.2686153846154);
#4382=CIRCLE('',#14013,17.6897435897436);
#4383=CIRCLE('',#14014,17.6897435897436);
#4384=CIRCLE('',#14016,21.);
#4385=CIRCLE('',#14017,20.35);
#4386=CIRCLE('',#14019,21.);
#4387=CIRCLE('',#14020,20.35);
#4388=CIRCLE('',#14021,21.);
#4389=CIRCLE('',#14030,3.96060240207311);
#4390=CIRCLE('',#14031,1.69469015025);
#4391=CIRCLE('',#14032,3.96060240207311);
#4392=CIRCLE('',#14034,3.39763111739558);
#4393=CIRCLE('',#14035,3.56616156686792);
#4394=CIRCLE('',#14036,3.39763111739558);
#4395=CIRCLE('',#14037,3.39763111739558);
#4396=CIRCLE('',#14038,3.39763111739558);
#4397=CIRCLE('',#14039,3.39763111739558);
#4398=CIRCLE('',#14040,3.39763111739558);
#4399=CIRCLE('',#14041,3.45272288248773);
#4400=CIRCLE('',#14042,3.45272288248773);
#4401=CIRCLE('',#14044,3.96060240207311);
#4402=CIRCLE('',#14045,1.69469015025);
#4403=CIRCLE('',#14046,3.96060240207311);
#4404=CIRCLE('',#14048,3.39763111739558);
#4405=CIRCLE('',#14049,3.56616156686792);
#4406=CIRCLE('',#14050,3.39763111739558);
#4407=CIRCLE('',#14051,3.39763111739558);
#4408=CIRCLE('',#14052,3.39763111739558);
#4409=CIRCLE('',#14053,3.39763111739558);
#4410=CIRCLE('',#14054,3.39763111739558);
#4411=CIRCLE('',#14055,3.45272288248773);
#4412=CIRCLE('',#14056,3.45272288248773);
#4413=CIRCLE('',#14058,3.96060240207311);
#4414=CIRCLE('',#14059,1.69469015025);
#4415=CIRCLE('',#14060,3.96060240207311);
#4416=CIRCLE('',#14062,3.39763111739558);
#4417=CIRCLE('',#14063,3.56616156686792);
#4418=CIRCLE('',#14064,3.39763111739558);
#4419=CIRCLE('',#14065,3.39763111739558);
#4420=CIRCLE('',#14066,3.39763111739558);
#4421=CIRCLE('',#14067,3.39763111739558);
#4422=CIRCLE('',#14068,3.39763111739558);
#4423=CIRCLE('',#14069,3.45272288248773);
#4424=CIRCLE('',#14070,3.45272288248773);
#4425=CIRCLE('',#14072,3.96060240207311);
#4426=CIRCLE('',#14073,1.69469015025);
#4427=CIRCLE('',#14074,3.96060240207311);
#4428=CIRCLE('',#14076,3.39763111739558);
#4429=CIRCLE('',#14077,3.56616156686792);
#4430=CIRCLE('',#14078,3.39763111739558);
#4431=CIRCLE('',#14079,3.39763111739558);
#4432=CIRCLE('',#14080,3.39763111739558);
#4433=CIRCLE('',#14081,3.39763111739558);
#4434=CIRCLE('',#14082,3.39763111739558);
#4435=CIRCLE('',#14083,3.45272288248773);
#4436=CIRCLE('',#14084,3.45272288248773);
#4437=CIRCLE('',#14086,3.96060240207311);
#4438=CIRCLE('',#14087,1.69469015025);
#4439=CIRCLE('',#14088,3.96060240207311);
#4440=CIRCLE('',#14090,3.39763111739558);
#4441=CIRCLE('',#14091,3.56616156686792);
#4442=CIRCLE('',#14092,3.39763111739558);
#4443=CIRCLE('',#14093,3.39763111739558);
#4444=CIRCLE('',#14094,3.39763111739558);
#4445=CIRCLE('',#14095,3.39763111739558);
#4446=CIRCLE('',#14096,3.39763111739558);
#4447=CIRCLE('',#14097,3.45272288248773);
#4448=CIRCLE('',#14098,3.45272288248773);
#4449=CIRCLE('',#14100,3.96060240207311);
#4450=CIRCLE('',#14101,1.69469015025);
#4451=CIRCLE('',#14102,3.96060240207311);
#4452=CIRCLE('',#14104,3.39763111739558);
#4453=CIRCLE('',#14105,3.39763111739558);
#4454=CIRCLE('',#14106,3.39763111739558);
#4455=CIRCLE('',#14107,3.56616156686792);
#4456=CIRCLE('',#14108,3.39763111739558);
#4457=CIRCLE('',#14109,3.39763111739558);
#4458=CIRCLE('',#14110,3.39763111739558);
#4459=CIRCLE('',#14111,3.45272288248773);
#4460=CIRCLE('',#14112,3.45272288248773);
#4461=CIRCLE('',#14114,3.39763111739558);
#4462=CIRCLE('',#14115,3.56616156686792);
#4463=CIRCLE('',#14116,3.39763111739558);
#4464=CIRCLE('',#14117,3.39763111739558);
#4465=CIRCLE('',#14118,3.39763111739558);
#4466=CIRCLE('',#14119,3.39763111739558);
#4467=CIRCLE('',#14120,3.39763111739558);
#4468=CIRCLE('',#14121,3.45272288248773);
#4469=CIRCLE('',#14122,3.45272288248773);
#4470=CIRCLE('',#14124,3.96060240207311);
#4471=CIRCLE('',#14125,1.69469015025);
#4472=CIRCLE('',#14126,3.96060240207311);
#4473=CIRCLE('',#14128,14.25);
#4474=CIRCLE('',#14129,14.25);
#4475=CIRCLE('',#14131,15.1423076923077);
#4476=CIRCLE('',#14132,15.1423076923077);
#4477=CIRCLE('',#14138,14.25);
#4478=CIRCLE('',#14139,15.1423076923077);
#4479=CIRCLE('',#14141,14.25);
#4480=CIRCLE('',#14142,15.1423076923077);
#4481=CIRCLE('',#14148,14.25);
#4482=CIRCLE('',#14149,15.1423076923077);
#4483=CIRCLE('',#14151,14.25);
#4484=CIRCLE('',#14152,15.1423076923077);
#4485=CIRCLE('',#14156,14.25);
#4486=CIRCLE('',#14157,14.25);
#4487=CIRCLE('',#14159,15.1423076923077);
#4488=CIRCLE('',#14160,15.1423076923077);
#4489=CIRCLE('',#14166,14.25);
#4490=CIRCLE('',#14167,15.1423076923077);
#4491=CIRCLE('',#14169,14.25);
#4492=CIRCLE('',#14170,15.1423076923077);
#4493=CIRCLE('',#14174,14.25);
#4494=CIRCLE('',#14175,14.25);
#4495=CIRCLE('',#14177,15.1423076923077);
#4496=CIRCLE('',#14178,15.1423076923077);
#4497=CIRCLE('',#14184,14.25);
#4498=CIRCLE('',#14185,15.1423076923077);
#4499=CIRCLE('',#14187,14.25);
#4500=CIRCLE('',#14188,15.1423076923077);
#4501=CIRCLE('',#14192,14.25);
#4502=CIRCLE('',#14193,14.25);
#4503=CIRCLE('',#14195,15.1423076923077);
#4504=CIRCLE('',#14196,15.1423076923077);
#4505=CIRCLE('',#14202,14.25);
#4506=CIRCLE('',#14203,15.1423076923077);
#4507=CIRCLE('',#14205,14.25);
#4508=CIRCLE('',#14206,15.1423076923077);
#4509=CIRCLE('',#14210,14.25);
#4510=CIRCLE('',#14211,14.25);
#4511=CIRCLE('',#14213,15.1423076923077);
#4512=CIRCLE('',#14214,15.1423076923077);
#4513=CIRCLE('',#14220,14.25);
#4514=CIRCLE('',#14221,15.1423076923077);
#4515=CIRCLE('',#14223,14.25);
#4516=CIRCLE('',#14224,15.1423076923077);
#4517=CIRCLE('',#14228,14.25);
#4518=CIRCLE('',#14229,14.25);
#4519=CIRCLE('',#14231,15.1423076923077);
#4520=CIRCLE('',#14232,15.1423076923077);
#4521=CIRCLE('',#14238,14.25);
#4522=CIRCLE('',#14239,15.1423076923077);
#4523=CIRCLE('',#14241,14.25);
#4524=CIRCLE('',#14242,15.1423076923077);
#4525=CIRCLE('',#14246,14.25);
#4526=CIRCLE('',#14247,15.1423076923077);
#4527=CIRCLE('',#14249,14.25);
#4528=CIRCLE('',#14250,15.1423076923077);
#4529=CIRCLE('',#14255,12.4653846153846);
#4530=CIRCLE('',#14256,3.56616156686793);
#4531=CIRCLE('',#14257,12.4653846153846);
#4532=CIRCLE('',#14259,7.64278544417155);
#4533=CIRCLE('',#14260,0.4875);
#4534=CIRCLE('',#14261,7.5);
#4535=CIRCLE('',#14262,7.5);
#4536=CIRCLE('',#14263,7.64278544417155);
#4537=CIRCLE('',#14265,7.5);
#4538=CIRCLE('',#14266,0.4875);
#4539=CIRCLE('',#14267,7.64278544417155);
#4540=CIRCLE('',#14268,7.5);
#4541=CIRCLE('',#14270,8.14999999999999);
#4542=CIRCLE('',#14273,8.14999999999999);
#4543=CIRCLE('',#14275,12.4653846153846);
#4544=CIRCLE('',#14277,12.4653846153846);
#4545=CIRCLE('',#14281,3.56616156686793);
#4546=CIRCLE('',#14283,3.56616156686793);
#4547=CIRCLE('',#14285,3.56616156686793);
#4548=CIRCLE('',#14287,3.56616156686793);
#4549=CIRCLE('',#14289,3.56616156686793);
#4550=CIRCLE('',#14291,3.56616156686793);
#4551=CIRCLE('',#14293,3.56616156686793);
#4552=CIRCLE('',#14295,16.3271153846154);
#4553=CIRCLE('',#14296,0.0585);
#4554=CIRCLE('',#14297,16.2686153846154);
#4555=CIRCLE('',#14298,16.2686153846154);
#4556=CIRCLE('',#14300,16.0346153846154);
#4557=CIRCLE('',#14301,0.0585);
#4558=CIRCLE('',#14302,16.0931153846154);
#4559=CIRCLE('',#14304,16.3271153846154);
#4560=CIRCLE('',#14305,0.0585);
#4561=CIRCLE('',#14306,16.2686153846154);
#4562=CIRCLE('',#14308,16.0346153846154);
#4563=CIRCLE('',#14309,0.0585);
#4564=CIRCLE('',#14310,16.0931153846154);
#4565=CIRCLE('',#14311,16.0346153846154);
#4566=CIRCLE('',#14313,17.6897435897436);
#4567=CIRCLE('',#14314,17.6897435897436);
#4568=CIRCLE('',#14316,16.2686153846154);
#4569=CIRCLE('',#14318,16.0346153846154);
#4570=CIRCLE('',#14320,3.56616156686793);
#4571=CIRCLE('',#14321,16.0346153846154);
#4572=CIRCLE('',#14324,16.2686153846154);
#4573=CIRCLE('',#14326,17.6897435897436);
#4574=CIRCLE('',#14327,17.6897435897436);
#4575=CIRCLE('',#14329,21.);
#4576=CIRCLE('',#14330,20.35);
#4577=CIRCLE('',#14332,21.);
#4578=CIRCLE('',#14333,21.);
#4579=CIRCLE('',#14334,20.35);
#4580=CIRCLE('',#14343,3.96060240207311);
#4581=CIRCLE('',#14344,1.69469015025);
#4582=CIRCLE('',#14345,3.96060240207311);
#4583=CIRCLE('',#14347,3.39763111739558);
#4584=CIRCLE('',#14348,3.39763111739558);
#4585=CIRCLE('',#14349,3.39763111739558);
#4586=CIRCLE('',#14350,3.56616156686792);
#4587=CIRCLE('',#14351,3.39763111739558);
#4588=CIRCLE('',#14352,3.39763111739558);
#4589=CIRCLE('',#14353,3.39763111739558);
#4590=CIRCLE('',#14354,3.45272288248773);
#4591=CIRCLE('',#14355,3.45272288248773);
#4592=CIRCLE('',#14357,3.96060240207311);
#4593=CIRCLE('',#14358,1.69469015025);
#4594=CIRCLE('',#14359,3.96060240207311);
#4595=CIRCLE('',#14361,3.39763111739558);
#4596=CIRCLE('',#14362,3.39763111739558);
#4597=CIRCLE('',#14363,3.39763111739558);
#4598=CIRCLE('',#14364,3.56616156686792);
#4599=CIRCLE('',#14365,3.39763111739558);
#4600=CIRCLE('',#14366,3.39763111739558);
#4601=CIRCLE('',#14367,3.39763111739558);
#4602=CIRCLE('',#14368,3.45272288248773);
#4603=CIRCLE('',#14369,3.45272288248773);
#4604=CIRCLE('',#14371,3.96060240207311);
#4605=CIRCLE('',#14372,1.69469015025);
#4606=CIRCLE('',#14373,3.96060240207311);
#4607=CIRCLE('',#14375,3.39763111739558);
#4608=CIRCLE('',#14376,3.39763111739558);
#4609=CIRCLE('',#14377,3.39763111739558);
#4610=CIRCLE('',#14378,3.56616156686792);
#4611=CIRCLE('',#14379,3.39763111739558);
#4612=CIRCLE('',#14380,3.39763111739558);
#4613=CIRCLE('',#14381,3.39763111739558);
#4614=CIRCLE('',#14382,3.45272288248773);
#4615=CIRCLE('',#14383,3.45272288248773);
#4616=CIRCLE('',#14385,3.96060240207311);
#4617=CIRCLE('',#14386,1.69469015025);
#4618=CIRCLE('',#14387,3.96060240207311);
#4619=CIRCLE('',#14389,3.39763111739558);
#4620=CIRCLE('',#14390,3.39763111739558);
#4621=CIRCLE('',#14391,3.39763111739558);
#4622=CIRCLE('',#14392,3.56616156686792);
#4623=CIRCLE('',#14393,3.39763111739558);
#4624=CIRCLE('',#14394,3.39763111739558);
#4625=CIRCLE('',#14395,3.39763111739558);
#4626=CIRCLE('',#14396,3.45272288248773);
#4627=CIRCLE('',#14397,3.45272288248773);
#4628=CIRCLE('',#14399,3.96060240207311);
#4629=CIRCLE('',#14400,1.69469015025);
#4630=CIRCLE('',#14401,3.96060240207311);
#4631=CIRCLE('',#14403,3.39763111739558);
#4632=CIRCLE('',#14404,3.39763111739558);
#4633=CIRCLE('',#14405,3.39763111739558);
#4634=CIRCLE('',#14406,3.56616156686792);
#4635=CIRCLE('',#14407,3.39763111739558);
#4636=CIRCLE('',#14408,3.39763111739558);
#4637=CIRCLE('',#14409,3.39763111739558);
#4638=CIRCLE('',#14410,3.45272288248773);
#4639=CIRCLE('',#14411,3.45272288248773);
#4640=CIRCLE('',#14413,3.96060240207311);
#4641=CIRCLE('',#14414,1.69469015025);
#4642=CIRCLE('',#14415,3.96060240207311);
#4643=CIRCLE('',#14417,3.39763111739558);
#4644=CIRCLE('',#14418,3.56616156686792);
#4645=CIRCLE('',#14419,3.39763111739558);
#4646=CIRCLE('',#14420,3.39763111739558);
#4647=CIRCLE('',#14421,3.39763111739558);
#4648=CIRCLE('',#14422,3.39763111739558);
#4649=CIRCLE('',#14423,3.39763111739558);
#4650=CIRCLE('',#14424,3.45272288248773);
#4651=CIRCLE('',#14425,3.45272288248773);
#4652=CIRCLE('',#14427,3.39763111739558);
#4653=CIRCLE('',#14428,3.39763111739558);
#4654=CIRCLE('',#14429,3.39763111739558);
#4655=CIRCLE('',#14430,3.56616156686792);
#4656=CIRCLE('',#14431,3.39763111739558);
#4657=CIRCLE('',#14432,3.39763111739558);
#4658=CIRCLE('',#14433,3.39763111739558);
#4659=CIRCLE('',#14434,3.45272288248773);
#4660=CIRCLE('',#14435,3.45272288248773);
#4661=CIRCLE('',#14437,3.96060240207311);
#4662=CIRCLE('',#14438,1.69469015025);
#4663=CIRCLE('',#14439,3.96060240207311);
#4664=CIRCLE('',#14441,14.25);
#4665=CIRCLE('',#14442,14.25);
#4666=CIRCLE('',#14444,15.1423076923077);
#4667=CIRCLE('',#14445,15.1423076923077);
#4668=CIRCLE('',#14451,14.25);
#4669=CIRCLE('',#14452,15.1423076923077);
#4670=CIRCLE('',#14454,15.1423076923077);
#4671=CIRCLE('',#14455,14.25);
#4672=CIRCLE('',#14461,15.1423076923077);
#4673=CIRCLE('',#14462,14.25);
#4674=CIRCLE('',#14464,14.25);
#4675=CIRCLE('',#14465,15.1423076923077);
#4676=CIRCLE('',#14469,14.25);
#4677=CIRCLE('',#14470,14.25);
#4678=CIRCLE('',#14472,15.1423076923077);
#4679=CIRCLE('',#14473,15.1423076923077);
#4680=CIRCLE('',#14479,15.1423076923077);
#4681=CIRCLE('',#14480,14.25);
#4682=CIRCLE('',#14482,14.25);
#4683=CIRCLE('',#14483,15.1423076923077);
#4684=CIRCLE('',#14487,14.25);
#4685=CIRCLE('',#14488,14.25);
#4686=CIRCLE('',#14490,15.1423076923077);
#4687=CIRCLE('',#14491,15.1423076923077);
#4688=CIRCLE('',#14497,15.1423076923077);
#4689=CIRCLE('',#14498,14.25);
#4690=CIRCLE('',#14500,14.25);
#4691=CIRCLE('',#14501,15.1423076923077);
#4692=CIRCLE('',#14505,14.25);
#4693=CIRCLE('',#14506,14.25);
#4694=CIRCLE('',#14508,15.1423076923077);
#4695=CIRCLE('',#14509,15.1423076923077);
#4696=CIRCLE('',#14515,15.1423076923077);
#4697=CIRCLE('',#14516,14.25);
#4698=CIRCLE('',#14518,14.25);
#4699=CIRCLE('',#14519,15.1423076923077);
#4700=CIRCLE('',#14523,14.25);
#4701=CIRCLE('',#14524,14.25);
#4702=CIRCLE('',#14526,15.1423076923077);
#4703=CIRCLE('',#14527,15.1423076923077);
#4704=CIRCLE('',#14533,15.1423076923077);
#4705=CIRCLE('',#14534,14.25);
#4706=CIRCLE('',#14536,14.25);
#4707=CIRCLE('',#14537,15.1423076923077);
#4708=CIRCLE('',#14541,14.25);
#4709=CIRCLE('',#14542,14.25);
#4710=CIRCLE('',#14544,15.1423076923077);
#4711=CIRCLE('',#14545,15.1423076923077);
#4712=CIRCLE('',#14551,15.1423076923077);
#4713=CIRCLE('',#14552,14.25);
#4714=CIRCLE('',#14554,14.25);
#4715=CIRCLE('',#14555,15.1423076923077);
#4716=CIRCLE('',#14559,15.1423076923077);
#4717=CIRCLE('',#14560,14.25);
#4718=CIRCLE('',#14562,14.25);
#4719=CIRCLE('',#14563,15.1423076923077);
#4720=CIRCLE('',#14568,12.4653846153846);
#4721=CIRCLE('',#14569,3.56616156686793);
#4722=CIRCLE('',#14570,12.4653846153846);
#4723=CIRCLE('',#14572,7.64278544417155);
#4724=CIRCLE('',#14573,0.4875);
#4725=CIRCLE('',#14574,7.5);
#4726=CIRCLE('',#14575,7.5);
#4727=CIRCLE('',#14576,7.64278544417155);
#4728=CIRCLE('',#14578,7.5);
#4729=CIRCLE('',#14579,0.4875);
#4730=CIRCLE('',#14580,7.64278544417155);
#4731=CIRCLE('',#14581,7.5);
#4732=CIRCLE('',#14583,8.14999999999999);
#4733=CIRCLE('',#14586,8.14999999999999);
#4734=CIRCLE('',#14588,12.4653846153846);
#4735=CIRCLE('',#14590,12.4653846153846);
#4736=CIRCLE('',#14594,3.56616156686793);
#4737=CIRCLE('',#14596,3.56616156686793);
#4738=CIRCLE('',#14598,3.56616156686793);
#4739=CIRCLE('',#14600,3.56616156686793);
#4740=CIRCLE('',#14602,3.56616156686793);
#4741=CIRCLE('',#14604,3.56616156686793);
#4742=CIRCLE('',#14606,3.56616156686793);
#4743=CIRCLE('',#14608,16.3271153846154);
#4744=CIRCLE('',#14609,0.0585);
#4745=CIRCLE('',#14610,16.2686153846154);
#4746=CIRCLE('',#14611,16.2686153846154);
#4747=CIRCLE('',#14613,16.0346153846154);
#4748=CIRCLE('',#14614,0.0585);
#4749=CIRCLE('',#14615,16.0931153846154);
#4750=CIRCLE('',#14617,16.3271153846154);
#4751=CIRCLE('',#14618,0.0585);
#4752=CIRCLE('',#14619,16.2686153846154);
#4753=CIRCLE('',#14621,16.0346153846154);
#4754=CIRCLE('',#14622,0.0585);
#4755=CIRCLE('',#14623,16.0931153846154);
#4756=CIRCLE('',#14624,16.0346153846154);
#4757=CIRCLE('',#14626,17.6897435897436);
#4758=CIRCLE('',#14627,17.6897435897436);
#4759=CIRCLE('',#14629,16.2686153846154);
#4760=CIRCLE('',#14631,16.0346153846154);
#4761=CIRCLE('',#14633,3.56616156686793);
#4762=CIRCLE('',#14634,16.0346153846154);
#4763=CIRCLE('',#14637,16.2686153846154);
#4764=CIRCLE('',#14639,17.6897435897436);
#4765=CIRCLE('',#14640,17.6897435897436);
#4766=CIRCLE('',#14642,21.);
#4767=CIRCLE('',#14643,20.35);
#4768=CIRCLE('',#14645,21.);
#4769=CIRCLE('',#14646,21.);
#4770=CIRCLE('',#14647,20.35);
#4771=CIRCLE('',#14656,3.96060240207311);
#4772=CIRCLE('',#14657,1.69469015025);
#4773=CIRCLE('',#14658,3.96060240207311);
#4774=CIRCLE('',#14660,3.39763111739558);
#4775=CIRCLE('',#14661,3.39763111739558);
#4776=CIRCLE('',#14662,3.39763111739558);
#4777=CIRCLE('',#14663,3.56616156686792);
#4778=CIRCLE('',#14664,3.39763111739558);
#4779=CIRCLE('',#14665,3.39763111739558);
#4780=CIRCLE('',#14666,3.39763111739558);
#4781=CIRCLE('',#14667,3.45272288248773);
#4782=CIRCLE('',#14668,3.45272288248773);
#4783=CIRCLE('',#14670,3.96060240207311);
#4784=CIRCLE('',#14671,1.69469015025);
#4785=CIRCLE('',#14672,3.96060240207311);
#4786=CIRCLE('',#14674,3.39763111739558);
#4787=CIRCLE('',#14675,3.39763111739558);
#4788=CIRCLE('',#14676,3.39763111739558);
#4789=CIRCLE('',#14677,3.56616156686792);
#4790=CIRCLE('',#14678,3.39763111739558);
#4791=CIRCLE('',#14679,3.39763111739558);
#4792=CIRCLE('',#14680,3.39763111739558);
#4793=CIRCLE('',#14681,3.45272288248773);
#4794=CIRCLE('',#14682,3.45272288248773);
#4795=CIRCLE('',#14684,3.96060240207311);
#4796=CIRCLE('',#14685,1.69469015025);
#4797=CIRCLE('',#14686,3.96060240207311);
#4798=CIRCLE('',#14688,3.39763111739558);
#4799=CIRCLE('',#14689,3.39763111739558);
#4800=CIRCLE('',#14690,3.39763111739558);
#4801=CIRCLE('',#14691,3.56616156686792);
#4802=CIRCLE('',#14692,3.39763111739558);
#4803=CIRCLE('',#14693,3.39763111739558);
#4804=CIRCLE('',#14694,3.39763111739558);
#4805=CIRCLE('',#14695,3.45272288248773);
#4806=CIRCLE('',#14696,3.45272288248773);
#4807=CIRCLE('',#14698,3.96060240207311);
#4808=CIRCLE('',#14699,1.69469015025);
#4809=CIRCLE('',#14700,3.96060240207311);
#4810=CIRCLE('',#14702,3.39763111739558);
#4811=CIRCLE('',#14703,3.39763111739558);
#4812=CIRCLE('',#14704,3.39763111739558);
#4813=CIRCLE('',#14705,3.56616156686792);
#4814=CIRCLE('',#14706,3.39763111739558);
#4815=CIRCLE('',#14707,3.39763111739558);
#4816=CIRCLE('',#14708,3.39763111739558);
#4817=CIRCLE('',#14709,3.45272288248773);
#4818=CIRCLE('',#14710,3.45272288248773);
#4819=CIRCLE('',#14712,3.96060240207311);
#4820=CIRCLE('',#14713,1.69469015025);
#4821=CIRCLE('',#14714,3.96060240207311);
#4822=CIRCLE('',#14716,3.39763111739558);
#4823=CIRCLE('',#14717,3.39763111739558);
#4824=CIRCLE('',#14718,3.39763111739558);
#4825=CIRCLE('',#14719,3.56616156686792);
#4826=CIRCLE('',#14720,3.39763111739558);
#4827=CIRCLE('',#14721,3.39763111739558);
#4828=CIRCLE('',#14722,3.39763111739558);
#4829=CIRCLE('',#14723,3.45272288248773);
#4830=CIRCLE('',#14724,3.45272288248773);
#4831=CIRCLE('',#14726,3.96060240207311);
#4832=CIRCLE('',#14727,1.69469015025);
#4833=CIRCLE('',#14728,3.96060240207311);
#4834=CIRCLE('',#14730,3.39763111739558);
#4835=CIRCLE('',#14731,3.56616156686792);
#4836=CIRCLE('',#14732,3.39763111739558);
#4837=CIRCLE('',#14733,3.39763111739558);
#4838=CIRCLE('',#14734,3.39763111739558);
#4839=CIRCLE('',#14735,3.39763111739558);
#4840=CIRCLE('',#14736,3.39763111739558);
#4841=CIRCLE('',#14737,3.45272288248773);
#4842=CIRCLE('',#14738,3.45272288248773);
#4843=CIRCLE('',#14740,3.39763111739558);
#4844=CIRCLE('',#14741,3.39763111739558);
#4845=CIRCLE('',#14742,3.39763111739558);
#4846=CIRCLE('',#14743,3.56616156686792);
#4847=CIRCLE('',#14744,3.39763111739558);
#4848=CIRCLE('',#14745,3.39763111739558);
#4849=CIRCLE('',#14746,3.39763111739558);
#4850=CIRCLE('',#14747,3.45272288248773);
#4851=CIRCLE('',#14748,3.45272288248773);
#4852=CIRCLE('',#14750,3.96060240207311);
#4853=CIRCLE('',#14751,1.69469015025);
#4854=CIRCLE('',#14752,3.96060240207311);
#4855=CIRCLE('',#14754,14.25);
#4856=CIRCLE('',#14755,14.25);
#4857=CIRCLE('',#14757,15.1423076923077);
#4858=CIRCLE('',#14758,15.1423076923077);
#4859=CIRCLE('',#14764,14.25);
#4860=CIRCLE('',#14765,15.1423076923077);
#4861=CIRCLE('',#14767,15.1423076923077);
#4862=CIRCLE('',#14768,14.25);
#4863=CIRCLE('',#14774,15.1423076923077);
#4864=CIRCLE('',#14775,14.25);
#4865=CIRCLE('',#14777,14.25);
#4866=CIRCLE('',#14778,15.1423076923077);
#4867=CIRCLE('',#14782,14.25);
#4868=CIRCLE('',#14783,14.25);
#4869=CIRCLE('',#14785,15.1423076923077);
#4870=CIRCLE('',#14786,15.1423076923077);
#4871=CIRCLE('',#14792,15.1423076923077);
#4872=CIRCLE('',#14793,14.25);
#4873=CIRCLE('',#14795,14.25);
#4874=CIRCLE('',#14796,15.1423076923077);
#4875=CIRCLE('',#14800,14.25);
#4876=CIRCLE('',#14801,14.25);
#4877=CIRCLE('',#14803,15.1423076923077);
#4878=CIRCLE('',#14804,15.1423076923077);
#4879=CIRCLE('',#14810,15.1423076923077);
#4880=CIRCLE('',#14811,14.25);
#4881=CIRCLE('',#14813,14.25);
#4882=CIRCLE('',#14814,15.1423076923077);
#4883=CIRCLE('',#14818,14.25);
#4884=CIRCLE('',#14819,14.25);
#4885=CIRCLE('',#14821,15.1423076923077);
#4886=CIRCLE('',#14822,15.1423076923077);
#4887=CIRCLE('',#14828,15.1423076923077);
#4888=CIRCLE('',#14829,14.25);
#4889=CIRCLE('',#14831,14.25);
#4890=CIRCLE('',#14832,15.1423076923077);
#4891=CIRCLE('',#14836,14.25);
#4892=CIRCLE('',#14837,14.25);
#4893=CIRCLE('',#14839,15.1423076923077);
#4894=CIRCLE('',#14840,15.1423076923077);
#4895=CIRCLE('',#14846,15.1423076923077);
#4896=CIRCLE('',#14847,14.25);
#4897=CIRCLE('',#14849,14.25);
#4898=CIRCLE('',#14850,15.1423076923077);
#4899=CIRCLE('',#14854,14.25);
#4900=CIRCLE('',#14855,14.25);
#4901=CIRCLE('',#14857,15.1423076923077);
#4902=CIRCLE('',#14858,15.1423076923077);
#4903=CIRCLE('',#14864,15.1423076923077);
#4904=CIRCLE('',#14865,14.25);
#4905=CIRCLE('',#14867,14.25);
#4906=CIRCLE('',#14868,15.1423076923077);
#4907=CIRCLE('',#14872,15.1423076923077);
#4908=CIRCLE('',#14873,14.25);
#4909=CIRCLE('',#14875,14.25);
#4910=CIRCLE('',#14876,15.1423076923077);
#4911=CIRCLE('',#14881,21.);
#4912=CIRCLE('',#14882,21.);
#4913=CIRCLE('',#14884,21.);
#4914=CIRCLE('',#14886,21.);
#4915=CIRCLE('',#14894,21.);
#4916=CIRCLE('',#14895,21.);
#4917=CIRCLE('',#14897,21.);
#4918=CIRCLE('',#14898,21.);
#4919=VERTEX_POINT('',#18822);
#4920=VERTEX_POINT('',#18824);
#4921=VERTEX_POINT('',#18828);
#4922=VERTEX_POINT('',#18830);
#4923=VERTEX_POINT('',#18836);
#4924=VERTEX_POINT('',#18837);
#4925=VERTEX_POINT('',#18839);
#4926=VERTEX_POINT('',#18841);
#4927=VERTEX_POINT('',#18845);
#4928=VERTEX_POINT('',#18847);
#4929=VERTEX_POINT('',#18851);
#4930=VERTEX_POINT('',#18852);
#4931=VERTEX_POINT('',#18854);
#4932=VERTEX_POINT('',#18856);
#4933=VERTEX_POINT('',#18860);
#4934=VERTEX_POINT('',#18862);
#4935=VERTEX_POINT('',#18866);
#4936=VERTEX_POINT('',#18867);
#4937=VERTEX_POINT('',#18869);
#4938=VERTEX_POINT('',#18871);
#4939=VERTEX_POINT('',#18875);
#4940=VERTEX_POINT('',#18877);
#4941=VERTEX_POINT('',#18881);
#4942=VERTEX_POINT('',#18882);
#4943=VERTEX_POINT('',#18884);
#4944=VERTEX_POINT('',#18886);
#4945=VERTEX_POINT('',#18890);
#4946=VERTEX_POINT('',#18892);
#4947=VERTEX_POINT('',#18896);
#4948=VERTEX_POINT('',#18897);
#4949=VERTEX_POINT('',#18899);
#4950=VERTEX_POINT('',#18901);
#4951=VERTEX_POINT('',#18905);
#4952=VERTEX_POINT('',#18907);
#4953=VERTEX_POINT('',#18911);
#4954=VERTEX_POINT('',#18912);
#4955=VERTEX_POINT('',#18914);
#4956=VERTEX_POINT('',#18916);
#4957=VERTEX_POINT('',#18920);
#4958=VERTEX_POINT('',#18922);
#4959=VERTEX_POINT('',#18926);
#4960=VERTEX_POINT('',#18927);
#4961=VERTEX_POINT('',#18929);
#4962=VERTEX_POINT('',#18931);
#4963=VERTEX_POINT('',#18935);
#4964=VERTEX_POINT('',#18937);
#4965=VERTEX_POINT('',#18941);
#4966=VERTEX_POINT('',#18942);
#4967=VERTEX_POINT('',#18944);
#4968=VERTEX_POINT('',#18946);
#4969=VERTEX_POINT('',#18950);
#4970=VERTEX_POINT('',#18952);
#4971=VERTEX_POINT('',#18956);
#4972=VERTEX_POINT('',#18957);
#4973=VERTEX_POINT('',#18959);
#4974=VERTEX_POINT('',#18961);
#4975=VERTEX_POINT('',#18965);
#4976=VERTEX_POINT('',#18967);
#4977=VERTEX_POINT('',#18971);
#4978=VERTEX_POINT('',#18972);
#4979=VERTEX_POINT('',#18974);
#4980=VERTEX_POINT('',#18976);
#4981=VERTEX_POINT('',#18980);
#4982=VERTEX_POINT('',#18982);
#4983=VERTEX_POINT('',#18986);
#4984=VERTEX_POINT('',#18987);
#4985=VERTEX_POINT('',#18989);
#4986=VERTEX_POINT('',#18991);
#4987=VERTEX_POINT('',#18995);
#4988=VERTEX_POINT('',#18997);
#4989=VERTEX_POINT('',#19001);
#4990=VERTEX_POINT('',#19002);
#4991=VERTEX_POINT('',#19004);
#4992=VERTEX_POINT('',#19006);
#4993=VERTEX_POINT('',#19010);
#4994=VERTEX_POINT('',#19012);
#4995=VERTEX_POINT('',#19016);
#4996=VERTEX_POINT('',#19017);
#4997=VERTEX_POINT('',#19019);
#4998=VERTEX_POINT('',#19021);
#4999=VERTEX_POINT('',#19025);
#5000=VERTEX_POINT('',#19027);
#5001=VERTEX_POINT('',#19031);
#5002=VERTEX_POINT('',#19032);
#5003=VERTEX_POINT('',#19034);
#5004=VERTEX_POINT('',#19036);
#5005=VERTEX_POINT('',#19040);
#5006=VERTEX_POINT('',#19042);
#5007=VERTEX_POINT('',#19046);
#5008=VERTEX_POINT('',#19047);
#5009=VERTEX_POINT('',#19049);
#5010=VERTEX_POINT('',#19051);
#5011=VERTEX_POINT('',#19055);
#5012=VERTEX_POINT('',#19057);
#5013=VERTEX_POINT('',#19061);
#5014=VERTEX_POINT('',#19062);
#5015=VERTEX_POINT('',#19064);
#5016=VERTEX_POINT('',#19066);
#5017=VERTEX_POINT('',#19070);
#5018=VERTEX_POINT('',#19072);
#5019=VERTEX_POINT('',#19076);
#5020=VERTEX_POINT('',#19077);
#5021=VERTEX_POINT('',#19079);
#5022=VERTEX_POINT('',#19081);
#5023=VERTEX_POINT('',#19085);
#5024=VERTEX_POINT('',#19087);
#5025=VERTEX_POINT('',#19091);
#5026=VERTEX_POINT('',#19092);
#5027=VERTEX_POINT('',#19094);
#5028=VERTEX_POINT('',#19096);
#5029=VERTEX_POINT('',#19100);
#5030=VERTEX_POINT('',#19102);
#5031=VERTEX_POINT('',#19106);
#5032=VERTEX_POINT('',#19107);
#5033=VERTEX_POINT('',#19109);
#5034=VERTEX_POINT('',#19111);
#5035=VERTEX_POINT('',#19115);
#5036=VERTEX_POINT('',#19117);
#5037=VERTEX_POINT('',#19121);
#5038=VERTEX_POINT('',#19122);
#5039=VERTEX_POINT('',#19124);
#5040=VERTEX_POINT('',#19126);
#5041=VERTEX_POINT('',#19130);
#5042=VERTEX_POINT('',#19132);
#5043=VERTEX_POINT('',#19136);
#5044=VERTEX_POINT('',#19137);
#5045=VERTEX_POINT('',#19139);
#5046=VERTEX_POINT('',#19141);
#5047=VERTEX_POINT('',#19145);
#5048=VERTEX_POINT('',#19147);
#5049=VERTEX_POINT('',#19151);
#5050=VERTEX_POINT('',#19152);
#5051=VERTEX_POINT('',#19154);
#5052=VERTEX_POINT('',#19156);
#5053=VERTEX_POINT('',#19160);
#5054=VERTEX_POINT('',#19162);
#5055=VERTEX_POINT('',#19166);
#5056=VERTEX_POINT('',#19167);
#5057=VERTEX_POINT('',#19169);
#5058=VERTEX_POINT('',#19171);
#5059=VERTEX_POINT('',#19175);
#5060=VERTEX_POINT('',#19177);
#5061=VERTEX_POINT('',#19181);
#5062=VERTEX_POINT('',#19182);
#5063=VERTEX_POINT('',#19184);
#5064=VERTEX_POINT('',#19186);
#5065=VERTEX_POINT('',#19190);
#5066=VERTEX_POINT('',#19192);
#5067=VERTEX_POINT('',#19196);
#5068=VERTEX_POINT('',#19197);
#5069=VERTEX_POINT('',#19199);
#5070=VERTEX_POINT('',#19201);
#5071=VERTEX_POINT('',#19205);
#5072=VERTEX_POINT('',#19207);
#5073=VERTEX_POINT('',#19211);
#5074=VERTEX_POINT('',#19212);
#5075=VERTEX_POINT('',#19214);
#5076=VERTEX_POINT('',#19216);
#5077=VERTEX_POINT('',#19220);
#5078=VERTEX_POINT('',#19222);
#5079=VERTEX_POINT('',#19226);
#5080=VERTEX_POINT('',#19227);
#5081=VERTEX_POINT('',#19229);
#5082=VERTEX_POINT('',#19231);
#5083=VERTEX_POINT('',#19235);
#5084=VERTEX_POINT('',#19237);
#5085=VERTEX_POINT('',#19241);
#5086=VERTEX_POINT('',#19242);
#5087=VERTEX_POINT('',#19244);
#5088=VERTEX_POINT('',#19246);
#5089=VERTEX_POINT('',#19250);
#5090=VERTEX_POINT('',#19252);
#5091=VERTEX_POINT('',#19256);
#5092=VERTEX_POINT('',#19257);
#5093=VERTEX_POINT('',#19259);
#5094=VERTEX_POINT('',#19261);
#5095=VERTEX_POINT('',#19265);
#5096=VERTEX_POINT('',#19267);
#5097=VERTEX_POINT('',#19271);
#5098=VERTEX_POINT('',#19272);
#5099=VERTEX_POINT('',#19274);
#5100=VERTEX_POINT('',#19276);
#5101=VERTEX_POINT('',#19280);
#5102=VERTEX_POINT('',#19282);
#5103=VERTEX_POINT('',#19286);
#5104=VERTEX_POINT('',#19287);
#5105=VERTEX_POINT('',#19289);
#5106=VERTEX_POINT('',#19291);
#5107=VERTEX_POINT('',#19295);
#5108=VERTEX_POINT('',#19297);
#5109=VERTEX_POINT('',#19301);
#5110=VERTEX_POINT('',#19302);
#5111=VERTEX_POINT('',#19304);
#5112=VERTEX_POINT('',#19306);
#5113=VERTEX_POINT('',#19310);
#5114=VERTEX_POINT('',#19312);
#5115=VERTEX_POINT('',#19316);
#5116=VERTEX_POINT('',#19317);
#5117=VERTEX_POINT('',#19319);
#5118=VERTEX_POINT('',#19321);
#5119=VERTEX_POINT('',#19325);
#5120=VERTEX_POINT('',#19327);
#5121=VERTEX_POINT('',#19331);
#5122=VERTEX_POINT('',#19332);
#5123=VERTEX_POINT('',#19334);
#5124=VERTEX_POINT('',#19336);
#5125=VERTEX_POINT('',#19340);
#5126=VERTEX_POINT('',#19342);
#5127=VERTEX_POINT('',#19346);
#5128=VERTEX_POINT('',#19347);
#5129=VERTEX_POINT('',#19349);
#5130=VERTEX_POINT('',#19351);
#5131=VERTEX_POINT('',#19355);
#5132=VERTEX_POINT('',#19357);
#5133=VERTEX_POINT('',#19361);
#5134=VERTEX_POINT('',#19362);
#5135=VERTEX_POINT('',#19364);
#5136=VERTEX_POINT('',#19366);
#5137=VERTEX_POINT('',#19370);
#5138=VERTEX_POINT('',#19372);
#5139=VERTEX_POINT('',#19376);
#5140=VERTEX_POINT('',#19377);
#5141=VERTEX_POINT('',#19379);
#5142=VERTEX_POINT('',#19381);
#5143=VERTEX_POINT('',#19385);
#5144=VERTEX_POINT('',#19387);
#5145=VERTEX_POINT('',#19391);
#5146=VERTEX_POINT('',#19392);
#5147=VERTEX_POINT('',#19394);
#5148=VERTEX_POINT('',#19396);
#5149=VERTEX_POINT('',#19400);
#5150=VERTEX_POINT('',#19402);
#5151=VERTEX_POINT('',#19555);
#5152=VERTEX_POINT('',#19630);
#5153=VERTEX_POINT('',#19708);
#5154=VERTEX_POINT('',#19710);
#5155=VERTEX_POINT('',#20161);
#5156=VERTEX_POINT('',#20236);
#5157=VERTEX_POINT('',#20314);
#5158=VERTEX_POINT('',#20316);
#5159=VERTEX_POINT('',#20767);
#5160=VERTEX_POINT('',#20842);
#5161=VERTEX_POINT('',#20920);
#5162=VERTEX_POINT('',#20922);
#5163=VERTEX_POINT('',#21373);
#5164=VERTEX_POINT('',#21448);
#5165=VERTEX_POINT('',#21526);
#5166=VERTEX_POINT('',#21528);
#5167=VERTEX_POINT('',#21979);
#5168=VERTEX_POINT('',#22054);
#5169=VERTEX_POINT('',#22132);
#5170=VERTEX_POINT('',#22134);
#5171=VERTEX_POINT('',#22585);
#5172=VERTEX_POINT('',#22660);
#5173=VERTEX_POINT('',#22738);
#5174=VERTEX_POINT('',#22740);
#5175=VERTEX_POINT('',#23191);
#5176=VERTEX_POINT('',#23266);
#5177=VERTEX_POINT('',#23344);
#5178=VERTEX_POINT('',#23346);
#5179=VERTEX_POINT('',#23797);
#5180=VERTEX_POINT('',#23872);
#5181=VERTEX_POINT('',#23950);
#5182=VERTEX_POINT('',#23952);
#5183=VERTEX_POINT('',#24403);
#5184=VERTEX_POINT('',#24478);
#5185=VERTEX_POINT('',#24556);
#5186=VERTEX_POINT('',#24558);
#5187=VERTEX_POINT('',#25009);
#5188=VERTEX_POINT('',#25084);
#5189=VERTEX_POINT('',#25162);
#5190=VERTEX_POINT('',#25164);
#5191=VERTEX_POINT('',#25615);
#5192=VERTEX_POINT('',#25690);
#5193=VERTEX_POINT('',#25768);
#5194=VERTEX_POINT('',#25770);
#5195=VERTEX_POINT('',#26221);
#5196=VERTEX_POINT('',#26296);
#5197=VERTEX_POINT('',#26374);
#5198=VERTEX_POINT('',#26376);
#5199=VERTEX_POINT('',#26827);
#5200=VERTEX_POINT('',#26902);
#5201=VERTEX_POINT('',#26980);
#5202=VERTEX_POINT('',#26982);
#5203=VERTEX_POINT('',#27433);
#5204=VERTEX_POINT('',#27508);
#5205=VERTEX_POINT('',#27586);
#5206=VERTEX_POINT('',#27588);
#5207=VERTEX_POINT('',#28039);
#5208=VERTEX_POINT('',#28114);
#5209=VERTEX_POINT('',#28192);
#5210=VERTEX_POINT('',#28194);
#5211=VERTEX_POINT('',#28645);
#5212=VERTEX_POINT('',#28720);
#5213=VERTEX_POINT('',#28798);
#5214=VERTEX_POINT('',#28800);
#5215=VERTEX_POINT('',#29251);
#5216=VERTEX_POINT('',#29326);
#5217=VERTEX_POINT('',#29404);
#5218=VERTEX_POINT('',#29406);
#5219=VERTEX_POINT('',#29857);
#5220=VERTEX_POINT('',#29932);
#5221=VERTEX_POINT('',#30010);
#5222=VERTEX_POINT('',#30012);
#5223=VERTEX_POINT('',#30463);
#5224=VERTEX_POINT('',#30538);
#5225=VERTEX_POINT('',#30616);
#5226=VERTEX_POINT('',#30618);
#5227=VERTEX_POINT('',#30937);
#5228=VERTEX_POINT('',#30939);
#5229=VERTEX_POINT('',#30941);
#5230=VERTEX_POINT('',#30943);
#5231=VERTEX_POINT('',#31018);
#5232=VERTEX_POINT('',#31020);
#5233=VERTEX_POINT('',#31095);
#5234=VERTEX_POINT('',#31097);
#5235=VERTEX_POINT('',#31102);
#5236=VERTEX_POINT('',#31104);
#5237=VERTEX_POINT('',#31106);
#5238=VERTEX_POINT('',#31108);
#5239=VERTEX_POINT('',#31183);
#5240=VERTEX_POINT('',#31185);
#5241=VERTEX_POINT('',#31261);
#5242=VERTEX_POINT('',#31263);
#5243=VERTEX_POINT('',#31619);
#5244=VERTEX_POINT('',#31621);
#5245=VERTEX_POINT('',#31625);
#5246=VERTEX_POINT('',#31627);
#5247=VERTEX_POINT('',#31633);
#5248=VERTEX_POINT('',#31634);
#5249=VERTEX_POINT('',#31636);
#5250=VERTEX_POINT('',#31638);
#5251=VERTEX_POINT('',#31642);
#5252=VERTEX_POINT('',#31644);
#5253=VERTEX_POINT('',#31648);
#5254=VERTEX_POINT('',#31649);
#5255=VERTEX_POINT('',#31651);
#5256=VERTEX_POINT('',#31653);
#5257=VERTEX_POINT('',#31657);
#5258=VERTEX_POINT('',#31659);
#5259=VERTEX_POINT('',#31663);
#5260=VERTEX_POINT('',#31664);
#5261=VERTEX_POINT('',#31666);
#5262=VERTEX_POINT('',#31668);
#5263=VERTEX_POINT('',#31672);
#5264=VERTEX_POINT('',#31674);
#5265=VERTEX_POINT('',#31678);
#5266=VERTEX_POINT('',#31679);
#5267=VERTEX_POINT('',#31681);
#5268=VERTEX_POINT('',#31683);
#5269=VERTEX_POINT('',#31687);
#5270=VERTEX_POINT('',#31689);
#5271=VERTEX_POINT('',#31693);
#5272=VERTEX_POINT('',#31694);
#5273=VERTEX_POINT('',#31696);
#5274=VERTEX_POINT('',#31698);
#5275=VERTEX_POINT('',#31702);
#5276=VERTEX_POINT('',#31704);
#5277=VERTEX_POINT('',#31708);
#5278=VERTEX_POINT('',#31709);
#5279=VERTEX_POINT('',#31711);
#5280=VERTEX_POINT('',#31713);
#5281=VERTEX_POINT('',#31717);
#5282=VERTEX_POINT('',#31719);
#5283=VERTEX_POINT('',#31723);
#5284=VERTEX_POINT('',#31724);
#5285=VERTEX_POINT('',#31726);
#5286=VERTEX_POINT('',#31728);
#5287=VERTEX_POINT('',#31732);
#5288=VERTEX_POINT('',#31734);
#5289=VERTEX_POINT('',#31738);
#5290=VERTEX_POINT('',#31739);
#5291=VERTEX_POINT('',#31741);
#5292=VERTEX_POINT('',#31743);
#5293=VERTEX_POINT('',#31747);
#5294=VERTEX_POINT('',#31749);
#5295=VERTEX_POINT('',#31753);
#5296=VERTEX_POINT('',#31754);
#5297=VERTEX_POINT('',#31756);
#5298=VERTEX_POINT('',#31758);
#5299=VERTEX_POINT('',#31762);
#5300=VERTEX_POINT('',#31764);
#5301=VERTEX_POINT('',#31768);
#5302=VERTEX_POINT('',#31769);
#5303=VERTEX_POINT('',#31771);
#5304=VERTEX_POINT('',#31773);
#5305=VERTEX_POINT('',#31777);
#5306=VERTEX_POINT('',#31779);
#5307=VERTEX_POINT('',#31783);
#5308=VERTEX_POINT('',#31784);
#5309=VERTEX_POINT('',#31786);
#5310=VERTEX_POINT('',#31788);
#5311=VERTEX_POINT('',#31792);
#5312=VERTEX_POINT('',#31794);
#5313=VERTEX_POINT('',#31798);
#5314=VERTEX_POINT('',#31799);
#5315=VERTEX_POINT('',#31801);
#5316=VERTEX_POINT('',#31803);
#5317=VERTEX_POINT('',#31807);
#5318=VERTEX_POINT('',#31809);
#5319=VERTEX_POINT('',#31813);
#5320=VERTEX_POINT('',#31814);
#5321=VERTEX_POINT('',#31816);
#5322=VERTEX_POINT('',#31818);
#5323=VERTEX_POINT('',#31822);
#5324=VERTEX_POINT('',#31824);
#5325=VERTEX_POINT('',#31828);
#5326=VERTEX_POINT('',#31829);
#5327=VERTEX_POINT('',#31831);
#5328=VERTEX_POINT('',#31833);
#5329=VERTEX_POINT('',#31837);
#5330=VERTEX_POINT('',#31839);
#5331=VERTEX_POINT('',#31843);
#5332=VERTEX_POINT('',#31844);
#5333=VERTEX_POINT('',#31846);
#5334=VERTEX_POINT('',#31848);
#5335=VERTEX_POINT('',#31852);
#5336=VERTEX_POINT('',#31854);
#5337=VERTEX_POINT('',#31858);
#5338=VERTEX_POINT('',#31859);
#5339=VERTEX_POINT('',#31861);
#5340=VERTEX_POINT('',#31863);
#5341=VERTEX_POINT('',#31867);
#5342=VERTEX_POINT('',#31869);
#5343=VERTEX_POINT('',#31873);
#5344=VERTEX_POINT('',#31874);
#5345=VERTEX_POINT('',#31876);
#5346=VERTEX_POINT('',#31878);
#5347=VERTEX_POINT('',#31882);
#5348=VERTEX_POINT('',#31884);
#5349=VERTEX_POINT('',#31888);
#5350=VERTEX_POINT('',#31889);
#5351=VERTEX_POINT('',#31891);
#5352=VERTEX_POINT('',#31893);
#5353=VERTEX_POINT('',#31897);
#5354=VERTEX_POINT('',#31899);
#5355=VERTEX_POINT('',#32052);
#5356=VERTEX_POINT('',#32127);
#5357=VERTEX_POINT('',#32205);
#5358=VERTEX_POINT('',#32207);
#5359=VERTEX_POINT('',#32658);
#5360=VERTEX_POINT('',#32733);
#5361=VERTEX_POINT('',#32811);
#5362=VERTEX_POINT('',#32813);
#5363=VERTEX_POINT('',#33264);
#5364=VERTEX_POINT('',#33339);
#5365=VERTEX_POINT('',#33417);
#5366=VERTEX_POINT('',#33419);
#5367=VERTEX_POINT('',#33870);
#5368=VERTEX_POINT('',#33945);
#5369=VERTEX_POINT('',#34023);
#5370=VERTEX_POINT('',#34025);
#5371=VERTEX_POINT('',#34476);
#5372=VERTEX_POINT('',#34551);
#5373=VERTEX_POINT('',#34629);
#5374=VERTEX_POINT('',#34631);
#5375=VERTEX_POINT('',#35082);
#5376=VERTEX_POINT('',#35157);
#5377=VERTEX_POINT('',#35235);
#5378=VERTEX_POINT('',#35237);
#5379=VERTEX_POINT('',#35688);
#5380=VERTEX_POINT('',#35763);
#5381=VERTEX_POINT('',#35841);
#5382=VERTEX_POINT('',#35843);
#5383=VERTEX_POINT('',#36294);
#5384=VERTEX_POINT('',#36369);
#5385=VERTEX_POINT('',#36447);
#5386=VERTEX_POINT('',#36449);
#5387=VERTEX_POINT('',#36900);
#5388=VERTEX_POINT('',#36975);
#5389=VERTEX_POINT('',#37053);
#5390=VERTEX_POINT('',#37055);
#5391=VERTEX_POINT('',#37364);
#5392=VERTEX_POINT('',#37366);
#5393=VERTEX_POINT('',#37368);
#5394=VERTEX_POINT('',#37370);
#5395=VERTEX_POINT('',#37445);
#5396=VERTEX_POINT('',#37447);
#5397=VERTEX_POINT('',#37522);
#5398=VERTEX_POINT('',#37524);
#5399=VERTEX_POINT('',#37529);
#5400=VERTEX_POINT('',#37531);
#5401=VERTEX_POINT('',#37533);
#5402=VERTEX_POINT('',#37535);
#5403=VERTEX_POINT('',#37610);
#5404=VERTEX_POINT('',#37612);
#5405=VERTEX_POINT('',#37688);
#5406=VERTEX_POINT('',#37690);
#5407=VERTEX_POINT('',#38026);
#5408=VERTEX_POINT('',#38028);
#5409=VERTEX_POINT('',#38032);
#5410=VERTEX_POINT('',#38033);
#5411=VERTEX_POINT('',#38036);
#5412=VERTEX_POINT('',#38038);
#5413=VERTEX_POINT('',#38042);
#5414=VERTEX_POINT('',#38043);
#5415=VERTEX_POINT('',#38046);
#5416=VERTEX_POINT('',#38050);
#5417=VERTEX_POINT('',#38056);
#5418=VERTEX_POINT('',#38060);
#5419=VERTEX_POINT('',#38064);
#5420=VERTEX_POINT('',#38070);
#5421=VERTEX_POINT('',#38071);
#5422=VERTEX_POINT('',#38074);
#5423=VERTEX_POINT('',#38075);
#5424=VERTEX_POINT('',#38078);
#5425=VERTEX_POINT('',#38079);
#5426=VERTEX_POINT('',#38082);
#5427=VERTEX_POINT('',#38083);
#5428=VERTEX_POINT('',#38086);
#5429=VERTEX_POINT('',#38087);
#5430=VERTEX_POINT('',#38090);
#5431=VERTEX_POINT('',#38091);
#5432=VERTEX_POINT('',#38094);
#5433=VERTEX_POINT('',#38095);
#5434=VERTEX_POINT('',#38098);
#5435=VERTEX_POINT('',#38100);
#5436=VERTEX_POINT('',#38102);
#5437=VERTEX_POINT('',#38106);
#5438=VERTEX_POINT('',#38108);
#5439=VERTEX_POINT('',#38112);
#5440=VERTEX_POINT('',#38114);
#5441=VERTEX_POINT('',#38118);
#5442=VERTEX_POINT('',#38119);
#5443=VERTEX_POINT('',#38122);
#5444=VERTEX_POINT('',#38126);
#5445=VERTEX_POINT('',#38128);
#5446=VERTEX_POINT('',#38132);
#5447=VERTEX_POINT('',#38136);
#5448=VERTEX_POINT('',#38140);
#5449=VERTEX_POINT('',#38146);
#5450=VERTEX_POINT('',#38150);
#5451=VERTEX_POINT('',#38152);
#5452=VERTEX_POINT('',#38156);
#5453=VERTEX_POINT('',#38158);
#5454=VERTEX_POINT('',#38162);
#5455=VERTEX_POINT('',#38163);
#5456=VERTEX_POINT('',#38165);
#5457=VERTEX_POINT('',#38178);
#5458=VERTEX_POINT('',#38180);
#5459=VERTEX_POINT('',#38183);
#5460=VERTEX_POINT('',#38184);
#5461=VERTEX_POINT('',#38191);
#5462=VERTEX_POINT('',#38211);
#5463=VERTEX_POINT('',#38237);
#5464=VERTEX_POINT('',#38238);
#5465=VERTEX_POINT('',#38245);
#5466=VERTEX_POINT('',#38265);
#5467=VERTEX_POINT('',#38292);
#5468=VERTEX_POINT('',#38293);
#5469=VERTEX_POINT('',#38295);
#5470=VERTEX_POINT('',#38297);
#5471=VERTEX_POINT('',#38299);
#5472=VERTEX_POINT('',#38307);
#5473=VERTEX_POINT('',#38309);
#5474=VERTEX_POINT('',#38318);
#5475=VERTEX_POINT('',#38320);
#5476=VERTEX_POINT('',#38327);
#5477=VERTEX_POINT('',#38335);
#5478=VERTEX_POINT('',#38337);
#5479=VERTEX_POINT('',#38340);
#5480=VERTEX_POINT('',#38342);
#5481=VERTEX_POINT('',#38345);
#5482=VERTEX_POINT('',#38346);
#5483=VERTEX_POINT('',#38353);
#5484=VERTEX_POINT('',#38373);
#5485=VERTEX_POINT('',#38399);
#5486=VERTEX_POINT('',#38400);
#5487=VERTEX_POINT('',#38407);
#5488=VERTEX_POINT('',#38427);
#5489=VERTEX_POINT('',#38454);
#5490=VERTEX_POINT('',#38455);
#5491=VERTEX_POINT('',#38457);
#5492=VERTEX_POINT('',#38459);
#5493=VERTEX_POINT('',#38461);
#5494=VERTEX_POINT('',#38469);
#5495=VERTEX_POINT('',#38471);
#5496=VERTEX_POINT('',#38480);
#5497=VERTEX_POINT('',#38482);
#5498=VERTEX_POINT('',#38489);
#5499=VERTEX_POINT('',#38497);
#5500=VERTEX_POINT('',#38499);
#5501=VERTEX_POINT('',#38502);
#5502=VERTEX_POINT('',#38504);
#5503=VERTEX_POINT('',#38507);
#5504=VERTEX_POINT('',#38508);
#5505=VERTEX_POINT('',#38515);
#5506=VERTEX_POINT('',#38535);
#5507=VERTEX_POINT('',#38561);
#5508=VERTEX_POINT('',#38562);
#5509=VERTEX_POINT('',#38569);
#5510=VERTEX_POINT('',#38589);
#5511=VERTEX_POINT('',#38616);
#5512=VERTEX_POINT('',#38617);
#5513=VERTEX_POINT('',#38619);
#5514=VERTEX_POINT('',#38621);
#5515=VERTEX_POINT('',#38623);
#5516=VERTEX_POINT('',#38631);
#5517=VERTEX_POINT('',#38633);
#5518=VERTEX_POINT('',#38642);
#5519=VERTEX_POINT('',#38644);
#5520=VERTEX_POINT('',#38651);
#5521=VERTEX_POINT('',#38659);
#5522=VERTEX_POINT('',#38661);
#5523=VERTEX_POINT('',#38664);
#5524=VERTEX_POINT('',#38666);
#5525=VERTEX_POINT('',#38669);
#5526=VERTEX_POINT('',#38670);
#5527=VERTEX_POINT('',#38677);
#5528=VERTEX_POINT('',#38697);
#5529=VERTEX_POINT('',#38723);
#5530=VERTEX_POINT('',#38724);
#5531=VERTEX_POINT('',#38731);
#5532=VERTEX_POINT('',#38751);
#5533=VERTEX_POINT('',#38778);
#5534=VERTEX_POINT('',#38779);
#5535=VERTEX_POINT('',#38781);
#5536=VERTEX_POINT('',#38783);
#5537=VERTEX_POINT('',#38785);
#5538=VERTEX_POINT('',#38793);
#5539=VERTEX_POINT('',#38795);
#5540=VERTEX_POINT('',#38804);
#5541=VERTEX_POINT('',#38806);
#5542=VERTEX_POINT('',#38813);
#5543=VERTEX_POINT('',#38821);
#5544=VERTEX_POINT('',#38823);
#5545=VERTEX_POINT('',#38826);
#5546=VERTEX_POINT('',#38828);
#5547=VERTEX_POINT('',#38831);
#5548=VERTEX_POINT('',#38832);
#5549=VERTEX_POINT('',#38839);
#5550=VERTEX_POINT('',#38859);
#5551=VERTEX_POINT('',#38885);
#5552=VERTEX_POINT('',#38886);
#5553=VERTEX_POINT('',#38893);
#5554=VERTEX_POINT('',#38913);
#5555=VERTEX_POINT('',#38940);
#5556=VERTEX_POINT('',#38941);
#5557=VERTEX_POINT('',#38943);
#5558=VERTEX_POINT('',#38945);
#5559=VERTEX_POINT('',#38947);
#5560=VERTEX_POINT('',#38955);
#5561=VERTEX_POINT('',#38957);
#5562=VERTEX_POINT('',#38966);
#5563=VERTEX_POINT('',#38968);
#5564=VERTEX_POINT('',#38975);
#5565=VERTEX_POINT('',#38983);
#5566=VERTEX_POINT('',#38985);
#5567=VERTEX_POINT('',#38988);
#5568=VERTEX_POINT('',#38990);
#5569=VERTEX_POINT('',#38993);
#5570=VERTEX_POINT('',#38994);
#5571=VERTEX_POINT('',#39014);
#5572=VERTEX_POINT('',#39021);
#5573=VERTEX_POINT('',#39047);
#5574=VERTEX_POINT('',#39048);
#5575=VERTEX_POINT('',#39055);
#5576=VERTEX_POINT('',#39075);
#5577=VERTEX_POINT('',#39102);
#5578=VERTEX_POINT('',#39103);
#5579=VERTEX_POINT('',#39105);
#5580=VERTEX_POINT('',#39112);
#5581=VERTEX_POINT('',#39114);
#5582=VERTEX_POINT('',#39122);
#5583=VERTEX_POINT('',#39124);
#5584=VERTEX_POINT('',#39126);
#5585=VERTEX_POINT('',#39134);
#5586=VERTEX_POINT('',#39136);
#5587=VERTEX_POINT('',#39145);
#5588=VERTEX_POINT('',#39147);
#5589=VERTEX_POINT('',#39150);
#5590=VERTEX_POINT('',#39151);
#5591=VERTEX_POINT('',#39153);
#5592=VERTEX_POINT('',#39155);
#5593=VERTEX_POINT('',#39157);
#5594=VERTEX_POINT('',#39165);
#5595=VERTEX_POINT('',#39167);
#5596=VERTEX_POINT('',#39176);
#5597=VERTEX_POINT('',#39178);
#5598=VERTEX_POINT('',#39185);
#5599=VERTEX_POINT('',#39193);
#5600=VERTEX_POINT('',#39195);
#5601=VERTEX_POINT('',#39198);
#5602=VERTEX_POINT('',#39200);
#5603=VERTEX_POINT('',#39203);
#5604=VERTEX_POINT('',#39204);
#5605=VERTEX_POINT('',#39211);
#5606=VERTEX_POINT('',#39231);
#5607=VERTEX_POINT('',#39257);
#5608=VERTEX_POINT('',#39258);
#5609=VERTEX_POINT('',#39265);
#5610=VERTEX_POINT('',#39285);
#5611=VERTEX_POINT('',#39439);
#5612=VERTEX_POINT('',#39441);
#5613=VERTEX_POINT('',#39445);
#5614=VERTEX_POINT('',#39446);
#5615=VERTEX_POINT('',#39449);
#5616=VERTEX_POINT('',#39451);
#5617=VERTEX_POINT('',#39455);
#5618=VERTEX_POINT('',#39456);
#5619=VERTEX_POINT('',#39459);
#5620=VERTEX_POINT('',#39463);
#5621=VERTEX_POINT('',#39469);
#5622=VERTEX_POINT('',#39473);
#5623=VERTEX_POINT('',#39477);
#5624=VERTEX_POINT('',#39483);
#5625=VERTEX_POINT('',#39484);
#5626=VERTEX_POINT('',#39487);
#5627=VERTEX_POINT('',#39488);
#5628=VERTEX_POINT('',#39491);
#5629=VERTEX_POINT('',#39492);
#5630=VERTEX_POINT('',#39495);
#5631=VERTEX_POINT('',#39496);
#5632=VERTEX_POINT('',#39499);
#5633=VERTEX_POINT('',#39500);
#5634=VERTEX_POINT('',#39503);
#5635=VERTEX_POINT('',#39504);
#5636=VERTEX_POINT('',#39507);
#5637=VERTEX_POINT('',#39508);
#5638=VERTEX_POINT('',#39511);
#5639=VERTEX_POINT('',#39513);
#5640=VERTEX_POINT('',#39515);
#5641=VERTEX_POINT('',#39519);
#5642=VERTEX_POINT('',#39521);
#5643=VERTEX_POINT('',#39525);
#5644=VERTEX_POINT('',#39527);
#5645=VERTEX_POINT('',#39531);
#5646=VERTEX_POINT('',#39532);
#5647=VERTEX_POINT('',#39535);
#5648=VERTEX_POINT('',#39539);
#5649=VERTEX_POINT('',#39541);
#5650=VERTEX_POINT('',#39545);
#5651=VERTEX_POINT('',#39549);
#5652=VERTEX_POINT('',#39553);
#5653=VERTEX_POINT('',#39559);
#5654=VERTEX_POINT('',#39563);
#5655=VERTEX_POINT('',#39565);
#5656=VERTEX_POINT('',#39569);
#5657=VERTEX_POINT('',#39571);
#5658=VERTEX_POINT('',#39575);
#5659=VERTEX_POINT('',#39576);
#5660=VERTEX_POINT('',#39578);
#5661=VERTEX_POINT('',#39591);
#5662=VERTEX_POINT('',#39593);
#5663=VERTEX_POINT('',#39596);
#5664=VERTEX_POINT('',#39597);
#5665=VERTEX_POINT('',#39604);
#5666=VERTEX_POINT('',#39624);
#5667=VERTEX_POINT('',#39650);
#5668=VERTEX_POINT('',#39651);
#5669=VERTEX_POINT('',#39658);
#5670=VERTEX_POINT('',#39678);
#5671=VERTEX_POINT('',#39705);
#5672=VERTEX_POINT('',#39706);
#5673=VERTEX_POINT('',#39708);
#5674=VERTEX_POINT('',#39710);
#5675=VERTEX_POINT('',#39712);
#5676=VERTEX_POINT('',#39720);
#5677=VERTEX_POINT('',#39722);
#5678=VERTEX_POINT('',#39731);
#5679=VERTEX_POINT('',#39733);
#5680=VERTEX_POINT('',#39740);
#5681=VERTEX_POINT('',#39748);
#5682=VERTEX_POINT('',#39750);
#5683=VERTEX_POINT('',#39753);
#5684=VERTEX_POINT('',#39755);
#5685=VERTEX_POINT('',#39758);
#5686=VERTEX_POINT('',#39759);
#5687=VERTEX_POINT('',#39766);
#5688=VERTEX_POINT('',#39786);
#5689=VERTEX_POINT('',#39812);
#5690=VERTEX_POINT('',#39813);
#5691=VERTEX_POINT('',#39820);
#5692=VERTEX_POINT('',#39840);
#5693=VERTEX_POINT('',#39867);
#5694=VERTEX_POINT('',#39868);
#5695=VERTEX_POINT('',#39870);
#5696=VERTEX_POINT('',#39872);
#5697=VERTEX_POINT('',#39874);
#5698=VERTEX_POINT('',#39882);
#5699=VERTEX_POINT('',#39884);
#5700=VERTEX_POINT('',#39893);
#5701=VERTEX_POINT('',#39895);
#5702=VERTEX_POINT('',#39902);
#5703=VERTEX_POINT('',#39910);
#5704=VERTEX_POINT('',#39912);
#5705=VERTEX_POINT('',#39915);
#5706=VERTEX_POINT('',#39917);
#5707=VERTEX_POINT('',#39920);
#5708=VERTEX_POINT('',#39921);
#5709=VERTEX_POINT('',#39928);
#5710=VERTEX_POINT('',#39948);
#5711=VERTEX_POINT('',#39974);
#5712=VERTEX_POINT('',#39975);
#5713=VERTEX_POINT('',#39982);
#5714=VERTEX_POINT('',#40002);
#5715=VERTEX_POINT('',#40029);
#5716=VERTEX_POINT('',#40030);
#5717=VERTEX_POINT('',#40032);
#5718=VERTEX_POINT('',#40034);
#5719=VERTEX_POINT('',#40036);
#5720=VERTEX_POINT('',#40044);
#5721=VERTEX_POINT('',#40046);
#5722=VERTEX_POINT('',#40055);
#5723=VERTEX_POINT('',#40057);
#5724=VERTEX_POINT('',#40064);
#5725=VERTEX_POINT('',#40072);
#5726=VERTEX_POINT('',#40074);
#5727=VERTEX_POINT('',#40077);
#5728=VERTEX_POINT('',#40079);
#5729=VERTEX_POINT('',#40082);
#5730=VERTEX_POINT('',#40083);
#5731=VERTEX_POINT('',#40090);
#5732=VERTEX_POINT('',#40110);
#5733=VERTEX_POINT('',#40136);
#5734=VERTEX_POINT('',#40137);
#5735=VERTEX_POINT('',#40144);
#5736=VERTEX_POINT('',#40164);
#5737=VERTEX_POINT('',#40191);
#5738=VERTEX_POINT('',#40192);
#5739=VERTEX_POINT('',#40194);
#5740=VERTEX_POINT('',#40196);
#5741=VERTEX_POINT('',#40198);
#5742=VERTEX_POINT('',#40206);
#5743=VERTEX_POINT('',#40208);
#5744=VERTEX_POINT('',#40217);
#5745=VERTEX_POINT('',#40219);
#5746=VERTEX_POINT('',#40226);
#5747=VERTEX_POINT('',#40234);
#5748=VERTEX_POINT('',#40236);
#5749=VERTEX_POINT('',#40239);
#5750=VERTEX_POINT('',#40241);
#5751=VERTEX_POINT('',#40244);
#5752=VERTEX_POINT('',#40245);
#5753=VERTEX_POINT('',#40252);
#5754=VERTEX_POINT('',#40272);
#5755=VERTEX_POINT('',#40298);
#5756=VERTEX_POINT('',#40299);
#5757=VERTEX_POINT('',#40306);
#5758=VERTEX_POINT('',#40326);
#5759=VERTEX_POINT('',#40353);
#5760=VERTEX_POINT('',#40354);
#5761=VERTEX_POINT('',#40356);
#5762=VERTEX_POINT('',#40358);
#5763=VERTEX_POINT('',#40360);
#5764=VERTEX_POINT('',#40368);
#5765=VERTEX_POINT('',#40370);
#5766=VERTEX_POINT('',#40379);
#5767=VERTEX_POINT('',#40381);
#5768=VERTEX_POINT('',#40388);
#5769=VERTEX_POINT('',#40396);
#5770=VERTEX_POINT('',#40398);
#5771=VERTEX_POINT('',#40401);
#5772=VERTEX_POINT('',#40403);
#5773=VERTEX_POINT('',#40406);
#5774=VERTEX_POINT('',#40407);
#5775=VERTEX_POINT('',#40427);
#5776=VERTEX_POINT('',#40434);
#5777=VERTEX_POINT('',#40460);
#5778=VERTEX_POINT('',#40461);
#5779=VERTEX_POINT('',#40468);
#5780=VERTEX_POINT('',#40488);
#5781=VERTEX_POINT('',#40515);
#5782=VERTEX_POINT('',#40516);
#5783=VERTEX_POINT('',#40518);
#5784=VERTEX_POINT('',#40525);
#5785=VERTEX_POINT('',#40527);
#5786=VERTEX_POINT('',#40535);
#5787=VERTEX_POINT('',#40537);
#5788=VERTEX_POINT('',#40539);
#5789=VERTEX_POINT('',#40547);
#5790=VERTEX_POINT('',#40549);
#5791=VERTEX_POINT('',#40558);
#5792=VERTEX_POINT('',#40560);
#5793=VERTEX_POINT('',#40563);
#5794=VERTEX_POINT('',#40564);
#5795=VERTEX_POINT('',#40566);
#5796=VERTEX_POINT('',#40568);
#5797=VERTEX_POINT('',#40570);
#5798=VERTEX_POINT('',#40578);
#5799=VERTEX_POINT('',#40580);
#5800=VERTEX_POINT('',#40589);
#5801=VERTEX_POINT('',#40591);
#5802=VERTEX_POINT('',#40598);
#5803=VERTEX_POINT('',#40606);
#5804=VERTEX_POINT('',#40608);
#5805=VERTEX_POINT('',#40611);
#5806=VERTEX_POINT('',#40613);
#5807=VERTEX_POINT('',#40616);
#5808=VERTEX_POINT('',#40617);
#5809=VERTEX_POINT('',#40624);
#5810=VERTEX_POINT('',#40644);
#5811=VERTEX_POINT('',#40670);
#5812=VERTEX_POINT('',#40671);
#5813=VERTEX_POINT('',#40678);
#5814=VERTEX_POINT('',#40698);
#5815=VERTEX_POINT('',#40852);
#5816=VERTEX_POINT('',#40854);
#5817=VERTEX_POINT('',#40858);
#5818=VERTEX_POINT('',#40859);
#5819=VERTEX_POINT('',#40861);
#5820=VERTEX_POINT('',#40863);
#5821=VERTEX_POINT('',#40868);
#5822=VERTEX_POINT('',#40869);
#5823=VERTEX_POINT('',#40871);
#5824=VERTEX_POINT('',#40876);
#5825=VERTEX_POINT('',#40882);
#5826=VERTEX_POINT('',#40886);
#5827=VERTEX_POINT('',#40890);
#5828=VERTEX_POINT('',#40896);
#5829=VERTEX_POINT('',#40897);
#5830=VERTEX_POINT('',#40900);
#5831=VERTEX_POINT('',#40901);
#5832=VERTEX_POINT('',#40904);
#5833=VERTEX_POINT('',#40905);
#5834=VERTEX_POINT('',#40908);
#5835=VERTEX_POINT('',#40909);
#5836=VERTEX_POINT('',#40912);
#5837=VERTEX_POINT('',#40913);
#5838=VERTEX_POINT('',#40916);
#5839=VERTEX_POINT('',#40917);
#5840=VERTEX_POINT('',#40920);
#5841=VERTEX_POINT('',#40921);
#5842=VERTEX_POINT('',#40924);
#5843=VERTEX_POINT('',#40926);
#5844=VERTEX_POINT('',#40928);
#5845=VERTEX_POINT('',#40932);
#5846=VERTEX_POINT('',#40934);
#5847=VERTEX_POINT('',#40938);
#5848=VERTEX_POINT('',#40940);
#5849=VERTEX_POINT('',#40944);
#5850=VERTEX_POINT('',#40945);
#5851=VERTEX_POINT('',#40947);
#5852=VERTEX_POINT('',#40952);
#5853=VERTEX_POINT('',#40954);
#5854=VERTEX_POINT('',#40958);
#5855=VERTEX_POINT('',#40962);
#5856=VERTEX_POINT('',#40966);
#5857=VERTEX_POINT('',#40972);
#5858=VERTEX_POINT('',#40976);
#5859=VERTEX_POINT('',#40978);
#5860=VERTEX_POINT('',#40982);
#5861=VERTEX_POINT('',#40984);
#5862=VERTEX_POINT('',#40988);
#5863=VERTEX_POINT('',#40989);
#5864=VERTEX_POINT('',#40992);
#5865=VERTEX_POINT('',#41004);
#5866=VERTEX_POINT('',#41006);
#5867=VERTEX_POINT('',#41009);
#5868=VERTEX_POINT('',#41010);
#5869=VERTEX_POINT('',#41017);
#5870=VERTEX_POINT('',#41037);
#5871=VERTEX_POINT('',#41063);
#5872=VERTEX_POINT('',#41064);
#5873=VERTEX_POINT('',#41071);
#5874=VERTEX_POINT('',#41091);
#5875=VERTEX_POINT('',#41118);
#5876=VERTEX_POINT('',#41119);
#5877=VERTEX_POINT('',#41121);
#5878=VERTEX_POINT('',#41128);
#5879=VERTEX_POINT('',#41130);
#5880=VERTEX_POINT('',#41138);
#5881=VERTEX_POINT('',#41140);
#5882=VERTEX_POINT('',#41142);
#5883=VERTEX_POINT('',#41150);
#5884=VERTEX_POINT('',#41152);
#5885=VERTEX_POINT('',#41161);
#5886=VERTEX_POINT('',#41163);
#5887=VERTEX_POINT('',#41166);
#5888=VERTEX_POINT('',#41168);
#5889=VERTEX_POINT('',#41171);
#5890=VERTEX_POINT('',#41172);
#5891=VERTEX_POINT('',#41179);
#5892=VERTEX_POINT('',#41199);
#5893=VERTEX_POINT('',#41225);
#5894=VERTEX_POINT('',#41226);
#5895=VERTEX_POINT('',#41233);
#5896=VERTEX_POINT('',#41253);
#5897=VERTEX_POINT('',#41280);
#5898=VERTEX_POINT('',#41281);
#5899=VERTEX_POINT('',#41283);
#5900=VERTEX_POINT('',#41290);
#5901=VERTEX_POINT('',#41292);
#5902=VERTEX_POINT('',#41300);
#5903=VERTEX_POINT('',#41302);
#5904=VERTEX_POINT('',#41304);
#5905=VERTEX_POINT('',#41312);
#5906=VERTEX_POINT('',#41314);
#5907=VERTEX_POINT('',#41323);
#5908=VERTEX_POINT('',#41325);
#5909=VERTEX_POINT('',#41328);
#5910=VERTEX_POINT('',#41330);
#5911=VERTEX_POINT('',#41333);
#5912=VERTEX_POINT('',#41334);
#5913=VERTEX_POINT('',#41341);
#5914=VERTEX_POINT('',#41361);
#5915=VERTEX_POINT('',#41387);
#5916=VERTEX_POINT('',#41388);
#5917=VERTEX_POINT('',#41395);
#5918=VERTEX_POINT('',#41415);
#5919=VERTEX_POINT('',#41442);
#5920=VERTEX_POINT('',#41443);
#5921=VERTEX_POINT('',#41445);
#5922=VERTEX_POINT('',#41452);
#5923=VERTEX_POINT('',#41454);
#5924=VERTEX_POINT('',#41462);
#5925=VERTEX_POINT('',#41464);
#5926=VERTEX_POINT('',#41466);
#5927=VERTEX_POINT('',#41474);
#5928=VERTEX_POINT('',#41476);
#5929=VERTEX_POINT('',#41485);
#5930=VERTEX_POINT('',#41487);
#5931=VERTEX_POINT('',#41490);
#5932=VERTEX_POINT('',#41492);
#5933=VERTEX_POINT('',#41495);
#5934=VERTEX_POINT('',#41496);
#5935=VERTEX_POINT('',#41503);
#5936=VERTEX_POINT('',#41523);
#5937=VERTEX_POINT('',#41549);
#5938=VERTEX_POINT('',#41550);
#5939=VERTEX_POINT('',#41557);
#5940=VERTEX_POINT('',#41577);
#5941=VERTEX_POINT('',#41604);
#5942=VERTEX_POINT('',#41605);
#5943=VERTEX_POINT('',#41607);
#5944=VERTEX_POINT('',#41614);
#5945=VERTEX_POINT('',#41616);
#5946=VERTEX_POINT('',#41624);
#5947=VERTEX_POINT('',#41626);
#5948=VERTEX_POINT('',#41628);
#5949=VERTEX_POINT('',#41636);
#5950=VERTEX_POINT('',#41638);
#5951=VERTEX_POINT('',#41647);
#5952=VERTEX_POINT('',#41649);
#5953=VERTEX_POINT('',#41652);
#5954=VERTEX_POINT('',#41654);
#5955=VERTEX_POINT('',#41657);
#5956=VERTEX_POINT('',#41658);
#5957=VERTEX_POINT('',#41665);
#5958=VERTEX_POINT('',#41685);
#5959=VERTEX_POINT('',#41711);
#5960=VERTEX_POINT('',#41712);
#5961=VERTEX_POINT('',#41719);
#5962=VERTEX_POINT('',#41739);
#5963=VERTEX_POINT('',#41766);
#5964=VERTEX_POINT('',#41767);
#5965=VERTEX_POINT('',#41769);
#5966=VERTEX_POINT('',#41776);
#5967=VERTEX_POINT('',#41778);
#5968=VERTEX_POINT('',#41786);
#5969=VERTEX_POINT('',#41788);
#5970=VERTEX_POINT('',#41790);
#5971=VERTEX_POINT('',#41798);
#5972=VERTEX_POINT('',#41800);
#5973=VERTEX_POINT('',#41809);
#5974=VERTEX_POINT('',#41811);
#5975=VERTEX_POINT('',#41814);
#5976=VERTEX_POINT('',#41816);
#5977=VERTEX_POINT('',#41819);
#5978=VERTEX_POINT('',#41820);
#5979=VERTEX_POINT('',#41840);
#5980=VERTEX_POINT('',#41847);
#5981=VERTEX_POINT('',#41873);
#5982=VERTEX_POINT('',#41874);
#5983=VERTEX_POINT('',#41881);
#5984=VERTEX_POINT('',#41901);
#5985=VERTEX_POINT('',#41928);
#5986=VERTEX_POINT('',#41929);
#5987=VERTEX_POINT('',#41931);
#5988=VERTEX_POINT('',#41933);
#5989=VERTEX_POINT('',#41935);
#5990=VERTEX_POINT('',#41943);
#5991=VERTEX_POINT('',#41945);
#5992=VERTEX_POINT('',#41954);
#5993=VERTEX_POINT('',#41956);
#5994=VERTEX_POINT('',#41963);
#5995=VERTEX_POINT('',#41971);
#5996=VERTEX_POINT('',#41973);
#5997=VERTEX_POINT('',#41976);
#5998=VERTEX_POINT('',#41977);
#5999=VERTEX_POINT('',#41979);
#6000=VERTEX_POINT('',#41986);
#6001=VERTEX_POINT('',#41988);
#6002=VERTEX_POINT('',#41996);
#6003=VERTEX_POINT('',#41998);
#6004=VERTEX_POINT('',#42000);
#6005=VERTEX_POINT('',#42008);
#6006=VERTEX_POINT('',#42010);
#6007=VERTEX_POINT('',#42019);
#6008=VERTEX_POINT('',#42021);
#6009=VERTEX_POINT('',#42024);
#6010=VERTEX_POINT('',#42026);
#6011=VERTEX_POINT('',#42029);
#6012=VERTEX_POINT('',#42030);
#6013=VERTEX_POINT('',#42037);
#6014=VERTEX_POINT('',#42057);
#6015=VERTEX_POINT('',#42083);
#6016=VERTEX_POINT('',#42084);
#6017=VERTEX_POINT('',#42091);
#6018=VERTEX_POINT('',#42111);
#6019=VERTEX_POINT('',#42265);
#6020=VERTEX_POINT('',#42267);
#6021=VERTEX_POINT('',#42271);
#6022=VERTEX_POINT('',#42272);
#6023=VERTEX_POINT('',#42274);
#6024=VERTEX_POINT('',#42276);
#6025=VERTEX_POINT('',#42281);
#6026=VERTEX_POINT('',#42282);
#6027=VERTEX_POINT('',#42284);
#6028=VERTEX_POINT('',#42289);
#6029=VERTEX_POINT('',#42295);
#6030=VERTEX_POINT('',#42299);
#6031=VERTEX_POINT('',#42303);
#6032=VERTEX_POINT('',#42309);
#6033=VERTEX_POINT('',#42310);
#6034=VERTEX_POINT('',#42313);
#6035=VERTEX_POINT('',#42314);
#6036=VERTEX_POINT('',#42317);
#6037=VERTEX_POINT('',#42318);
#6038=VERTEX_POINT('',#42321);
#6039=VERTEX_POINT('',#42322);
#6040=VERTEX_POINT('',#42325);
#6041=VERTEX_POINT('',#42326);
#6042=VERTEX_POINT('',#42329);
#6043=VERTEX_POINT('',#42330);
#6044=VERTEX_POINT('',#42333);
#6045=VERTEX_POINT('',#42334);
#6046=VERTEX_POINT('',#42337);
#6047=VERTEX_POINT('',#42339);
#6048=VERTEX_POINT('',#42341);
#6049=VERTEX_POINT('',#42345);
#6050=VERTEX_POINT('',#42347);
#6051=VERTEX_POINT('',#42351);
#6052=VERTEX_POINT('',#42353);
#6053=VERTEX_POINT('',#42357);
#6054=VERTEX_POINT('',#42358);
#6055=VERTEX_POINT('',#42360);
#6056=VERTEX_POINT('',#42365);
#6057=VERTEX_POINT('',#42367);
#6058=VERTEX_POINT('',#42371);
#6059=VERTEX_POINT('',#42375);
#6060=VERTEX_POINT('',#42379);
#6061=VERTEX_POINT('',#42385);
#6062=VERTEX_POINT('',#42389);
#6063=VERTEX_POINT('',#42391);
#6064=VERTEX_POINT('',#42395);
#6065=VERTEX_POINT('',#42397);
#6066=VERTEX_POINT('',#42401);
#6067=VERTEX_POINT('',#42402);
#6068=VERTEX_POINT('',#42405);
#6069=VERTEX_POINT('',#42417);
#6070=VERTEX_POINT('',#42419);
#6071=VERTEX_POINT('',#42422);
#6072=VERTEX_POINT('',#42423);
#6073=VERTEX_POINT('',#42430);
#6074=VERTEX_POINT('',#42450);
#6075=VERTEX_POINT('',#42476);
#6076=VERTEX_POINT('',#42477);
#6077=VERTEX_POINT('',#42484);
#6078=VERTEX_POINT('',#42504);
#6079=VERTEX_POINT('',#42531);
#6080=VERTEX_POINT('',#42532);
#6081=VERTEX_POINT('',#42534);
#6082=VERTEX_POINT('',#42541);
#6083=VERTEX_POINT('',#42543);
#6084=VERTEX_POINT('',#42551);
#6085=VERTEX_POINT('',#42553);
#6086=VERTEX_POINT('',#42555);
#6087=VERTEX_POINT('',#42563);
#6088=VERTEX_POINT('',#42565);
#6089=VERTEX_POINT('',#42574);
#6090=VERTEX_POINT('',#42576);
#6091=VERTEX_POINT('',#42579);
#6092=VERTEX_POINT('',#42581);
#6093=VERTEX_POINT('',#42584);
#6094=VERTEX_POINT('',#42585);
#6095=VERTEX_POINT('',#42592);
#6096=VERTEX_POINT('',#42612);
#6097=VERTEX_POINT('',#42638);
#6098=VERTEX_POINT('',#42639);
#6099=VERTEX_POINT('',#42646);
#6100=VERTEX_POINT('',#42666);
#6101=VERTEX_POINT('',#42693);
#6102=VERTEX_POINT('',#42694);
#6103=VERTEX_POINT('',#42696);
#6104=VERTEX_POINT('',#42703);
#6105=VERTEX_POINT('',#42705);
#6106=VERTEX_POINT('',#42713);
#6107=VERTEX_POINT('',#42715);
#6108=VERTEX_POINT('',#42717);
#6109=VERTEX_POINT('',#42725);
#6110=VERTEX_POINT('',#42727);
#6111=VERTEX_POINT('',#42736);
#6112=VERTEX_POINT('',#42738);
#6113=VERTEX_POINT('',#42741);
#6114=VERTEX_POINT('',#42743);
#6115=VERTEX_POINT('',#42746);
#6116=VERTEX_POINT('',#42747);
#6117=VERTEX_POINT('',#42754);
#6118=VERTEX_POINT('',#42774);
#6119=VERTEX_POINT('',#42800);
#6120=VERTEX_POINT('',#42801);
#6121=VERTEX_POINT('',#42808);
#6122=VERTEX_POINT('',#42828);
#6123=VERTEX_POINT('',#42855);
#6124=VERTEX_POINT('',#42856);
#6125=VERTEX_POINT('',#42858);
#6126=VERTEX_POINT('',#42865);
#6127=VERTEX_POINT('',#42867);
#6128=VERTEX_POINT('',#42875);
#6129=VERTEX_POINT('',#42877);
#6130=VERTEX_POINT('',#42879);
#6131=VERTEX_POINT('',#42887);
#6132=VERTEX_POINT('',#42889);
#6133=VERTEX_POINT('',#42898);
#6134=VERTEX_POINT('',#42900);
#6135=VERTEX_POINT('',#42903);
#6136=VERTEX_POINT('',#42905);
#6137=VERTEX_POINT('',#42908);
#6138=VERTEX_POINT('',#42909);
#6139=VERTEX_POINT('',#42916);
#6140=VERTEX_POINT('',#42936);
#6141=VERTEX_POINT('',#42962);
#6142=VERTEX_POINT('',#42963);
#6143=VERTEX_POINT('',#42970);
#6144=VERTEX_POINT('',#42990);
#6145=VERTEX_POINT('',#43017);
#6146=VERTEX_POINT('',#43018);
#6147=VERTEX_POINT('',#43020);
#6148=VERTEX_POINT('',#43027);
#6149=VERTEX_POINT('',#43029);
#6150=VERTEX_POINT('',#43037);
#6151=VERTEX_POINT('',#43039);
#6152=VERTEX_POINT('',#43041);
#6153=VERTEX_POINT('',#43049);
#6154=VERTEX_POINT('',#43051);
#6155=VERTEX_POINT('',#43060);
#6156=VERTEX_POINT('',#43062);
#6157=VERTEX_POINT('',#43065);
#6158=VERTEX_POINT('',#43067);
#6159=VERTEX_POINT('',#43070);
#6160=VERTEX_POINT('',#43071);
#6161=VERTEX_POINT('',#43078);
#6162=VERTEX_POINT('',#43098);
#6163=VERTEX_POINT('',#43124);
#6164=VERTEX_POINT('',#43125);
#6165=VERTEX_POINT('',#43132);
#6166=VERTEX_POINT('',#43152);
#6167=VERTEX_POINT('',#43179);
#6168=VERTEX_POINT('',#43180);
#6169=VERTEX_POINT('',#43182);
#6170=VERTEX_POINT('',#43189);
#6171=VERTEX_POINT('',#43191);
#6172=VERTEX_POINT('',#43199);
#6173=VERTEX_POINT('',#43201);
#6174=VERTEX_POINT('',#43203);
#6175=VERTEX_POINT('',#43211);
#6176=VERTEX_POINT('',#43213);
#6177=VERTEX_POINT('',#43222);
#6178=VERTEX_POINT('',#43224);
#6179=VERTEX_POINT('',#43227);
#6180=VERTEX_POINT('',#43229);
#6181=VERTEX_POINT('',#43232);
#6182=VERTEX_POINT('',#43233);
#6183=VERTEX_POINT('',#43253);
#6184=VERTEX_POINT('',#43260);
#6185=VERTEX_POINT('',#43286);
#6186=VERTEX_POINT('',#43287);
#6187=VERTEX_POINT('',#43294);
#6188=VERTEX_POINT('',#43314);
#6189=VERTEX_POINT('',#43341);
#6190=VERTEX_POINT('',#43342);
#6191=VERTEX_POINT('',#43344);
#6192=VERTEX_POINT('',#43346);
#6193=VERTEX_POINT('',#43348);
#6194=VERTEX_POINT('',#43356);
#6195=VERTEX_POINT('',#43358);
#6196=VERTEX_POINT('',#43367);
#6197=VERTEX_POINT('',#43369);
#6198=VERTEX_POINT('',#43376);
#6199=VERTEX_POINT('',#43384);
#6200=VERTEX_POINT('',#43386);
#6201=VERTEX_POINT('',#43389);
#6202=VERTEX_POINT('',#43390);
#6203=VERTEX_POINT('',#43392);
#6204=VERTEX_POINT('',#43399);
#6205=VERTEX_POINT('',#43401);
#6206=VERTEX_POINT('',#43409);
#6207=VERTEX_POINT('',#43411);
#6208=VERTEX_POINT('',#43413);
#6209=VERTEX_POINT('',#43421);
#6210=VERTEX_POINT('',#43423);
#6211=VERTEX_POINT('',#43432);
#6212=VERTEX_POINT('',#43434);
#6213=VERTEX_POINT('',#43437);
#6214=VERTEX_POINT('',#43439);
#6215=VERTEX_POINT('',#43442);
#6216=VERTEX_POINT('',#43443);
#6217=VERTEX_POINT('',#43450);
#6218=VERTEX_POINT('',#43470);
#6219=VERTEX_POINT('',#43496);
#6220=VERTEX_POINT('',#43497);
#6221=VERTEX_POINT('',#43504);
#6222=VERTEX_POINT('',#43524);
#6223=VERTEX_POINT('',#43678);
#6224=VERTEX_POINT('',#43680);
#6225=VERTEX_POINT('',#43684);
#6226=VERTEX_POINT('',#43685);
#6227=VERTEX_POINT('',#43687);
#6228=VERTEX_POINT('',#43689);
#6229=VERTEX_POINT('',#43692);
#6230=VERTEX_POINT('',#43695);
#6231=VERTEX_POINT('',#43699);
#6232=VERTEX_POINT('',#43700);
#6233=VERTEX_POINT('',#43702);
#6234=VERTEX_POINT('',#43704);
#6235=VERTEX_POINT('',#43717);
#6236=VERTEX_POINT('',#43719);
#6237=VERTEX_POINT('',#43723);
#6238=VERTEX_POINT('',#43725);
#6239=VERTEX_POINT('',#43729);
#6240=VERTEX_POINT('',#43730);
#6241=VERTEX_POINT('',#43732);
#6242=VERTEX_POINT('',#43734);
#6243=VERTEX_POINT('',#43738);
#6244=VERTEX_POINT('',#43740);
#6245=VERTEX_POINT('',#43744);
#6246=VERTEX_POINT('',#43748);
#6247=EDGE_CURVE('',#4919,#4919,#3899,.T.);
#6248=EDGE_CURVE('',#4919,#4920,#3003,.T.);
#6249=EDGE_CURVE('',#4920,#4920,#3900,.F.);
#6250=EDGE_CURVE('',#4921,#4921,#3901,.T.);
#6251=EDGE_CURVE('',#4921,#4922,#3004,.T.);
#6252=EDGE_CURVE('',#4922,#4922,#3902,.T.);
#6253=EDGE_CURVE('',#4923,#4924,#3903,.T.);
#6254=EDGE_CURVE('',#4924,#4925,#3005,.T.);
#6255=EDGE_CURVE('',#4925,#4926,#3904,.T.);
#6256=EDGE_CURVE('',#4926,#4923,#3006,.T.);
#6257=EDGE_CURVE('',#4927,#4924,#3007,.T.);
#6258=EDGE_CURVE('',#4928,#4927,#3008,.T.);
#6259=EDGE_CURVE('',#4925,#4928,#3009,.T.);
#6260=EDGE_CURVE('',#4929,#4930,#3905,.T.);
#6261=EDGE_CURVE('',#4930,#4931,#3010,.T.);
#6262=EDGE_CURVE('',#4931,#4932,#3906,.T.);
#6263=EDGE_CURVE('',#4932,#4929,#3011,.T.);
#6264=EDGE_CURVE('',#4930,#4933,#3012,.T.);
#6265=EDGE_CURVE('',#4933,#4934,#3013,.T.);
#6266=EDGE_CURVE('',#4931,#4934,#3014,.T.);
#6267=EDGE_CURVE('',#4935,#4936,#3907,.T.);
#6268=EDGE_CURVE('',#4936,#4937,#3015,.T.);
#6269=EDGE_CURVE('',#4937,#4938,#3908,.T.);
#6270=EDGE_CURVE('',#4938,#4935,#3016,.T.);
#6271=EDGE_CURVE('',#4939,#4936,#3017,.T.);
#6272=EDGE_CURVE('',#4940,#4939,#3018,.T.);
#6273=EDGE_CURVE('',#4937,#4940,#3019,.T.);
#6274=EDGE_CURVE('',#4941,#4942,#3909,.T.);
#6275=EDGE_CURVE('',#4942,#4943,#3020,.T.);
#6276=EDGE_CURVE('',#4943,#4944,#3910,.T.);
#6277=EDGE_CURVE('',#4944,#4941,#3021,.T.);
#6278=EDGE_CURVE('',#4942,#4945,#3022,.T.);
#6279=EDGE_CURVE('',#4945,#4946,#3023,.T.);
#6280=EDGE_CURVE('',#4943,#4946,#3024,.T.);
#6281=EDGE_CURVE('',#4947,#4948,#3911,.T.);
#6282=EDGE_CURVE('',#4948,#4949,#3025,.T.);
#6283=EDGE_CURVE('',#4949,#4950,#3912,.T.);
#6284=EDGE_CURVE('',#4950,#4947,#3026,.T.);
#6285=EDGE_CURVE('',#4951,#4948,#3027,.T.);
#6286=EDGE_CURVE('',#4952,#4951,#3028,.T.);
#6287=EDGE_CURVE('',#4949,#4952,#3029,.T.);
#6288=EDGE_CURVE('',#4953,#4954,#3913,.T.);
#6289=EDGE_CURVE('',#4954,#4955,#3030,.T.);
#6290=EDGE_CURVE('',#4955,#4956,#3914,.T.);
#6291=EDGE_CURVE('',#4956,#4953,#3031,.T.);
#6292=EDGE_CURVE('',#4954,#4957,#3032,.T.);
#6293=EDGE_CURVE('',#4957,#4958,#3033,.T.);
#6294=EDGE_CURVE('',#4955,#4958,#3034,.T.);
#6295=EDGE_CURVE('',#4959,#4960,#3915,.T.);
#6296=EDGE_CURVE('',#4960,#4961,#3035,.T.);
#6297=EDGE_CURVE('',#4961,#4962,#3916,.T.);
#6298=EDGE_CURVE('',#4962,#4959,#3036,.T.);
#6299=EDGE_CURVE('',#4963,#4960,#3037,.T.);
#6300=EDGE_CURVE('',#4964,#4963,#3038,.T.);
#6301=EDGE_CURVE('',#4961,#4964,#3039,.T.);
#6302=EDGE_CURVE('',#4965,#4966,#3917,.T.);
#6303=EDGE_CURVE('',#4966,#4967,#3040,.T.);
#6304=EDGE_CURVE('',#4967,#4968,#3918,.T.);
#6305=EDGE_CURVE('',#4968,#4965,#3041,.T.);
#6306=EDGE_CURVE('',#4966,#4969,#3042,.T.);
#6307=EDGE_CURVE('',#4969,#4970,#3043,.T.);
#6308=EDGE_CURVE('',#4967,#4970,#3044,.T.);
#6309=EDGE_CURVE('',#4971,#4972,#3919,.T.);
#6310=EDGE_CURVE('',#4972,#4973,#3045,.T.);
#6311=EDGE_CURVE('',#4973,#4974,#3920,.T.);
#6312=EDGE_CURVE('',#4974,#4971,#3046,.T.);
#6313=EDGE_CURVE('',#4975,#4972,#3047,.T.);
#6314=EDGE_CURVE('',#4976,#4975,#3048,.T.);
#6315=EDGE_CURVE('',#4973,#4976,#3049,.T.);
#6316=EDGE_CURVE('',#4977,#4978,#3921,.T.);
#6317=EDGE_CURVE('',#4978,#4979,#3050,.T.);
#6318=EDGE_CURVE('',#4979,#4980,#3922,.T.);
#6319=EDGE_CURVE('',#4980,#4977,#3051,.T.);
#6320=EDGE_CURVE('',#4978,#4981,#3052,.T.);
#6321=EDGE_CURVE('',#4981,#4982,#3053,.T.);
#6322=EDGE_CURVE('',#4979,#4982,#3054,.T.);
#6323=EDGE_CURVE('',#4983,#4984,#3923,.T.);
#6324=EDGE_CURVE('',#4984,#4985,#3055,.T.);
#6325=EDGE_CURVE('',#4985,#4986,#3924,.T.);
#6326=EDGE_CURVE('',#4986,#4983,#3056,.T.);
#6327=EDGE_CURVE('',#4987,#4984,#3057,.T.);
#6328=EDGE_CURVE('',#4988,#4987,#3058,.T.);
#6329=EDGE_CURVE('',#4985,#4988,#3059,.T.);
#6330=EDGE_CURVE('',#4989,#4990,#3925,.T.);
#6331=EDGE_CURVE('',#4990,#4991,#3060,.T.);
#6332=EDGE_CURVE('',#4991,#4992,#3926,.T.);
#6333=EDGE_CURVE('',#4992,#4989,#3061,.T.);
#6334=EDGE_CURVE('',#4990,#4993,#3062,.T.);
#6335=EDGE_CURVE('',#4993,#4994,#3063,.T.);
#6336=EDGE_CURVE('',#4991,#4994,#3064,.T.);
#6337=EDGE_CURVE('',#4995,#4996,#3927,.T.);
#6338=EDGE_CURVE('',#4996,#4997,#3065,.T.);
#6339=EDGE_CURVE('',#4997,#4998,#3928,.T.);
#6340=EDGE_CURVE('',#4998,#4995,#3066,.T.);
#6341=EDGE_CURVE('',#4999,#4996,#3067,.T.);
#6342=EDGE_CURVE('',#5000,#4999,#3068,.T.);
#6343=EDGE_CURVE('',#4997,#5000,#3069,.T.);
#6344=EDGE_CURVE('',#5001,#5002,#3929,.T.);
#6345=EDGE_CURVE('',#5002,#5003,#3070,.T.);
#6346=EDGE_CURVE('',#5003,#5004,#3930,.T.);
#6347=EDGE_CURVE('',#5004,#5001,#3071,.T.);
#6348=EDGE_CURVE('',#5002,#5005,#3072,.T.);
#6349=EDGE_CURVE('',#5005,#5006,#3073,.T.);
#6350=EDGE_CURVE('',#5003,#5006,#3074,.T.);
#6351=EDGE_CURVE('',#5007,#5008,#3931,.T.);
#6352=EDGE_CURVE('',#5008,#5009,#3075,.T.);
#6353=EDGE_CURVE('',#5009,#5010,#3932,.T.);
#6354=EDGE_CURVE('',#5010,#5007,#3076,.T.);
#6355=EDGE_CURVE('',#5011,#5008,#3077,.T.);
#6356=EDGE_CURVE('',#5012,#5011,#3078,.T.);
#6357=EDGE_CURVE('',#5009,#5012,#3079,.T.);
#6358=EDGE_CURVE('',#5013,#5014,#3933,.T.);
#6359=EDGE_CURVE('',#5014,#5015,#3080,.T.);
#6360=EDGE_CURVE('',#5015,#5016,#3934,.T.);
#6361=EDGE_CURVE('',#5016,#5013,#3081,.T.);
#6362=EDGE_CURVE('',#5014,#5017,#3082,.T.);
#6363=EDGE_CURVE('',#5017,#5018,#3083,.T.);
#6364=EDGE_CURVE('',#5015,#5018,#3084,.T.);
#6365=EDGE_CURVE('',#5019,#5020,#3935,.T.);
#6366=EDGE_CURVE('',#5020,#5021,#3085,.T.);
#6367=EDGE_CURVE('',#5021,#5022,#3936,.T.);
#6368=EDGE_CURVE('',#5022,#5019,#3086,.T.);
#6369=EDGE_CURVE('',#5023,#5020,#3087,.T.);
#6370=EDGE_CURVE('',#5024,#5023,#3088,.T.);
#6371=EDGE_CURVE('',#5021,#5024,#3089,.T.);
#6372=EDGE_CURVE('',#5025,#5026,#3937,.T.);
#6373=EDGE_CURVE('',#5026,#5027,#3090,.T.);
#6374=EDGE_CURVE('',#5027,#5028,#3938,.T.);
#6375=EDGE_CURVE('',#5028,#5025,#3091,.T.);
#6376=EDGE_CURVE('',#5026,#5029,#3092,.T.);
#6377=EDGE_CURVE('',#5029,#5030,#3093,.T.);
#6378=EDGE_CURVE('',#5027,#5030,#3094,.T.);
#6379=EDGE_CURVE('',#5031,#5032,#3939,.T.);
#6380=EDGE_CURVE('',#5032,#5033,#3095,.T.);
#6381=EDGE_CURVE('',#5033,#5034,#3940,.T.);
#6382=EDGE_CURVE('',#5034,#5031,#3096,.T.);
#6383=EDGE_CURVE('',#5035,#5032,#3097,.T.);
#6384=EDGE_CURVE('',#5036,#5035,#3098,.T.);
#6385=EDGE_CURVE('',#5033,#5036,#3099,.T.);
#6386=EDGE_CURVE('',#5037,#5038,#3941,.T.);
#6387=EDGE_CURVE('',#5038,#5039,#3100,.T.);
#6388=EDGE_CURVE('',#5039,#5040,#3942,.T.);
#6389=EDGE_CURVE('',#5040,#5037,#3101,.T.);
#6390=EDGE_CURVE('',#5038,#5041,#3102,.T.);
#6391=EDGE_CURVE('',#5041,#5042,#3103,.T.);
#6392=EDGE_CURVE('',#5039,#5042,#3104,.T.);
#6393=EDGE_CURVE('',#5043,#5044,#3943,.T.);
#6394=EDGE_CURVE('',#5044,#5045,#3105,.T.);
#6395=EDGE_CURVE('',#5045,#5046,#3944,.T.);
#6396=EDGE_CURVE('',#5046,#5043,#3106,.T.);
#6397=EDGE_CURVE('',#5047,#5044,#3107,.T.);
#6398=EDGE_CURVE('',#5048,#5047,#3108,.T.);
#6399=EDGE_CURVE('',#5045,#5048,#3109,.T.);
#6400=EDGE_CURVE('',#5049,#5050,#3945,.T.);
#6401=EDGE_CURVE('',#5050,#5051,#3110,.T.);
#6402=EDGE_CURVE('',#5051,#5052,#3946,.T.);
#6403=EDGE_CURVE('',#5052,#5049,#3111,.T.);
#6404=EDGE_CURVE('',#5050,#5053,#3112,.T.);
#6405=EDGE_CURVE('',#5053,#5054,#3113,.T.);
#6406=EDGE_CURVE('',#5051,#5054,#3114,.T.);
#6407=EDGE_CURVE('',#5055,#5056,#3947,.T.);
#6408=EDGE_CURVE('',#5056,#5057,#3115,.T.);
#6409=EDGE_CURVE('',#5057,#5058,#3948,.T.);
#6410=EDGE_CURVE('',#5058,#5055,#3116,.T.);
#6411=EDGE_CURVE('',#5059,#5056,#3117,.T.);
#6412=EDGE_CURVE('',#5060,#5059,#3118,.T.);
#6413=EDGE_CURVE('',#5057,#5060,#3119,.T.);
#6414=EDGE_CURVE('',#5061,#5062,#3949,.T.);
#6415=EDGE_CURVE('',#5062,#5063,#3120,.T.);
#6416=EDGE_CURVE('',#5063,#5064,#3950,.T.);
#6417=EDGE_CURVE('',#5064,#5061,#3121,.T.);
#6418=EDGE_CURVE('',#5062,#5065,#3122,.T.);
#6419=EDGE_CURVE('',#5065,#5066,#3123,.T.);
#6420=EDGE_CURVE('',#5063,#5066,#3124,.T.);
#6421=EDGE_CURVE('',#5067,#5068,#3951,.T.);
#6422=EDGE_CURVE('',#5068,#5069,#3125,.T.);
#6423=EDGE_CURVE('',#5069,#5070,#3952,.T.);
#6424=EDGE_CURVE('',#5070,#5067,#3126,.T.);
#6425=EDGE_CURVE('',#5071,#5068,#3127,.T.);
#6426=EDGE_CURVE('',#5072,#5071,#3128,.T.);
#6427=EDGE_CURVE('',#5069,#5072,#3129,.T.);
#6428=EDGE_CURVE('',#5073,#5074,#3953,.T.);
#6429=EDGE_CURVE('',#5074,#5075,#3130,.T.);
#6430=EDGE_CURVE('',#5075,#5076,#3954,.T.);
#6431=EDGE_CURVE('',#5076,#5073,#3131,.T.);
#6432=EDGE_CURVE('',#5074,#5077,#3132,.T.);
#6433=EDGE_CURVE('',#5077,#5078,#3133,.T.);
#6434=EDGE_CURVE('',#5075,#5078,#3134,.T.);
#6435=EDGE_CURVE('',#5079,#5080,#3955,.T.);
#6436=EDGE_CURVE('',#5080,#5081,#3135,.T.);
#6437=EDGE_CURVE('',#5081,#5082,#3956,.T.);
#6438=EDGE_CURVE('',#5082,#5079,#3136,.T.);
#6439=EDGE_CURVE('',#5083,#5080,#3137,.T.);
#6440=EDGE_CURVE('',#5084,#5083,#3138,.T.);
#6441=EDGE_CURVE('',#5081,#5084,#3139,.T.);
#6442=EDGE_CURVE('',#5085,#5086,#3957,.T.);
#6443=EDGE_CURVE('',#5086,#5087,#3140,.T.);
#6444=EDGE_CURVE('',#5087,#5088,#3958,.T.);
#6445=EDGE_CURVE('',#5088,#5085,#3141,.T.);
#6446=EDGE_CURVE('',#5086,#5089,#3142,.T.);
#6447=EDGE_CURVE('',#5089,#5090,#3143,.T.);
#6448=EDGE_CURVE('',#5087,#5090,#3144,.T.);
#6449=EDGE_CURVE('',#5091,#5092,#3959,.T.);
#6450=EDGE_CURVE('',#5092,#5093,#3145,.T.);
#6451=EDGE_CURVE('',#5093,#5094,#3960,.T.);
#6452=EDGE_CURVE('',#5094,#5091,#3146,.T.);
#6453=EDGE_CURVE('',#5095,#5092,#3147,.T.);
#6454=EDGE_CURVE('',#5096,#5095,#3148,.T.);
#6455=EDGE_CURVE('',#5093,#5096,#3149,.T.);
#6456=EDGE_CURVE('',#5097,#5098,#3961,.T.);
#6457=EDGE_CURVE('',#5098,#5099,#3150,.T.);
#6458=EDGE_CURVE('',#5099,#5100,#3962,.T.);
#6459=EDGE_CURVE('',#5100,#5097,#3151,.T.);
#6460=EDGE_CURVE('',#5098,#5101,#3152,.T.);
#6461=EDGE_CURVE('',#5101,#5102,#3153,.T.);
#6462=EDGE_CURVE('',#5099,#5102,#3154,.T.);
#6463=EDGE_CURVE('',#5103,#5104,#3963,.T.);
#6464=EDGE_CURVE('',#5104,#5105,#3155,.T.);
#6465=EDGE_CURVE('',#5105,#5106,#3964,.T.);
#6466=EDGE_CURVE('',#5106,#5103,#3156,.T.);
#6467=EDGE_CURVE('',#5107,#5104,#3157,.T.);
#6468=EDGE_CURVE('',#5108,#5107,#3158,.T.);
#6469=EDGE_CURVE('',#5105,#5108,#3159,.T.);
#6470=EDGE_CURVE('',#5109,#5110,#3965,.T.);
#6471=EDGE_CURVE('',#5110,#5111,#3160,.T.);
#6472=EDGE_CURVE('',#5111,#5112,#3966,.T.);
#6473=EDGE_CURVE('',#5112,#5109,#3161,.T.);
#6474=EDGE_CURVE('',#5110,#5113,#3162,.T.);
#6475=EDGE_CURVE('',#5113,#5114,#3163,.T.);
#6476=EDGE_CURVE('',#5111,#5114,#3164,.T.);
#6477=EDGE_CURVE('',#5115,#5116,#3967,.T.);
#6478=EDGE_CURVE('',#5116,#5117,#3165,.T.);
#6479=EDGE_CURVE('',#5117,#5118,#3968,.T.);
#6480=EDGE_CURVE('',#5118,#5115,#3166,.T.);
#6481=EDGE_CURVE('',#5119,#5116,#3167,.T.);
#6482=EDGE_CURVE('',#5120,#5119,#3168,.T.);
#6483=EDGE_CURVE('',#5117,#5120,#3169,.T.);
#6484=EDGE_CURVE('',#5121,#5122,#3969,.T.);
#6485=EDGE_CURVE('',#5122,#5123,#3170,.T.);
#6486=EDGE_CURVE('',#5123,#5124,#3970,.T.);
#6487=EDGE_CURVE('',#5124,#5121,#3171,.T.);
#6488=EDGE_CURVE('',#5122,#5125,#3172,.T.);
#6489=EDGE_CURVE('',#5125,#5126,#3173,.T.);
#6490=EDGE_CURVE('',#5123,#5126,#3174,.T.);
#6491=EDGE_CURVE('',#5127,#5128,#3971,.T.);
#6492=EDGE_CURVE('',#5128,#5129,#3175,.T.);
#6493=EDGE_CURVE('',#5129,#5130,#3972,.T.);
#6494=EDGE_CURVE('',#5130,#5127,#3176,.T.);
#6495=EDGE_CURVE('',#5131,#5128,#3177,.T.);
#6496=EDGE_CURVE('',#5132,#5131,#3178,.T.);
#6497=EDGE_CURVE('',#5129,#5132,#3179,.T.);
#6498=EDGE_CURVE('',#5133,#5134,#3973,.T.);
#6499=EDGE_CURVE('',#5134,#5135,#3180,.T.);
#6500=EDGE_CURVE('',#5135,#5136,#3974,.T.);
#6501=EDGE_CURVE('',#5136,#5133,#3181,.T.);
#6502=EDGE_CURVE('',#5134,#5137,#3182,.T.);
#6503=EDGE_CURVE('',#5137,#5138,#3183,.T.);
#6504=EDGE_CURVE('',#5135,#5138,#3184,.T.);
#6505=EDGE_CURVE('',#5139,#5140,#3975,.T.);
#6506=EDGE_CURVE('',#5140,#5141,#3185,.T.);
#6507=EDGE_CURVE('',#5141,#5142,#3976,.T.);
#6508=EDGE_CURVE('',#5142,#5139,#3186,.T.);
#6509=EDGE_CURVE('',#5143,#5140,#3187,.T.);
#6510=EDGE_CURVE('',#5144,#5143,#3188,.T.);
#6511=EDGE_CURVE('',#5141,#5144,#3189,.T.);
#6512=EDGE_CURVE('',#5145,#5146,#3977,.T.);
#6513=EDGE_CURVE('',#5146,#5147,#3190,.T.);
#6514=EDGE_CURVE('',#5147,#5148,#3978,.T.);
#6515=EDGE_CURVE('',#5148,#5145,#3191,.T.);
#6516=EDGE_CURVE('',#5146,#5149,#3192,.T.);
#6517=EDGE_CURVE('',#5149,#5150,#3193,.T.);
#6518=EDGE_CURVE('',#5147,#5150,#3194,.T.);
#6519=EDGE_CURVE('',#4928,#5151,#491,.T.);
#6520=EDGE_CURVE('',#5152,#4927,#492,.T.);
#6521=EDGE_CURVE('',#5151,#5152,#3195,.T.);
#6522=EDGE_CURVE('',#5153,#5151,#3979,.T.);
#6523=EDGE_CURVE('',#5154,#5152,#3980,.T.);
#6524=EDGE_CURVE('',#5153,#5154,#3196,.T.);
#6525=EDGE_CURVE('',#4933,#5153,#493,.T.);
#6526=EDGE_CURVE('',#4934,#5154,#494,.T.);
#6527=EDGE_CURVE('',#4940,#5155,#495,.T.);
#6528=EDGE_CURVE('',#5156,#4939,#496,.T.);
#6529=EDGE_CURVE('',#5155,#5156,#3197,.T.);
#6530=EDGE_CURVE('',#5157,#5155,#3981,.T.);
#6531=EDGE_CURVE('',#5158,#5156,#3982,.T.);
#6532=EDGE_CURVE('',#5157,#5158,#3198,.T.);
#6533=EDGE_CURVE('',#4945,#5157,#497,.T.);
#6534=EDGE_CURVE('',#4946,#5158,#498,.T.);
#6535=EDGE_CURVE('',#4952,#5159,#499,.T.);
#6536=EDGE_CURVE('',#5160,#4951,#500,.T.);
#6537=EDGE_CURVE('',#5159,#5160,#3199,.T.);
#6538=EDGE_CURVE('',#5161,#5159,#3983,.T.);
#6539=EDGE_CURVE('',#5162,#5160,#3984,.T.);
#6540=EDGE_CURVE('',#5161,#5162,#3200,.T.);
#6541=EDGE_CURVE('',#4957,#5161,#501,.T.);
#6542=EDGE_CURVE('',#4958,#5162,#502,.T.);
#6543=EDGE_CURVE('',#4964,#5163,#503,.T.);
#6544=EDGE_CURVE('',#5164,#4963,#504,.T.);
#6545=EDGE_CURVE('',#5163,#5164,#3201,.T.);
#6546=EDGE_CURVE('',#5165,#5163,#3985,.T.);
#6547=EDGE_CURVE('',#5166,#5164,#3986,.T.);
#6548=EDGE_CURVE('',#5165,#5166,#3202,.T.);
#6549=EDGE_CURVE('',#4969,#5165,#505,.T.);
#6550=EDGE_CURVE('',#4970,#5166,#506,.T.);
#6551=EDGE_CURVE('',#4976,#5167,#507,.T.);
#6552=EDGE_CURVE('',#5168,#4975,#508,.T.);
#6553=EDGE_CURVE('',#5167,#5168,#3203,.T.);
#6554=EDGE_CURVE('',#5169,#5167,#3987,.T.);
#6555=EDGE_CURVE('',#5170,#5168,#3988,.T.);
#6556=EDGE_CURVE('',#5169,#5170,#3204,.T.);
#6557=EDGE_CURVE('',#4981,#5169,#509,.T.);
#6558=EDGE_CURVE('',#4982,#5170,#510,.T.);
#6559=EDGE_CURVE('',#4988,#5171,#511,.T.);
#6560=EDGE_CURVE('',#5172,#4987,#512,.T.);
#6561=EDGE_CURVE('',#5171,#5172,#3205,.T.);
#6562=EDGE_CURVE('',#5173,#5171,#3989,.T.);
#6563=EDGE_CURVE('',#5174,#5172,#3990,.T.);
#6564=EDGE_CURVE('',#5173,#5174,#3206,.T.);
#6565=EDGE_CURVE('',#4993,#5173,#513,.T.);
#6566=EDGE_CURVE('',#4994,#5174,#514,.T.);
#6567=EDGE_CURVE('',#5000,#5175,#515,.T.);
#6568=EDGE_CURVE('',#5176,#4999,#516,.T.);
#6569=EDGE_CURVE('',#5175,#5176,#3207,.T.);
#6570=EDGE_CURVE('',#5177,#5175,#3991,.T.);
#6571=EDGE_CURVE('',#5178,#5176,#3992,.T.);
#6572=EDGE_CURVE('',#5177,#5178,#3208,.T.);
#6573=EDGE_CURVE('',#5005,#5177,#517,.T.);
#6574=EDGE_CURVE('',#5006,#5178,#518,.T.);
#6575=EDGE_CURVE('',#5012,#5179,#519,.T.);
#6576=EDGE_CURVE('',#5180,#5011,#520,.T.);
#6577=EDGE_CURVE('',#5179,#5180,#3209,.T.);
#6578=EDGE_CURVE('',#5181,#5179,#3993,.T.);
#6579=EDGE_CURVE('',#5182,#5180,#3994,.T.);
#6580=EDGE_CURVE('',#5181,#5182,#3210,.T.);
#6581=EDGE_CURVE('',#5017,#5181,#521,.T.);
#6582=EDGE_CURVE('',#5018,#5182,#522,.T.);
#6583=EDGE_CURVE('',#5024,#5183,#523,.T.);
#6584=EDGE_CURVE('',#5184,#5023,#524,.T.);
#6585=EDGE_CURVE('',#5183,#5184,#3211,.T.);
#6586=EDGE_CURVE('',#5185,#5183,#3995,.T.);
#6587=EDGE_CURVE('',#5186,#5184,#3996,.T.);
#6588=EDGE_CURVE('',#5185,#5186,#3212,.T.);
#6589=EDGE_CURVE('',#5029,#5185,#525,.T.);
#6590=EDGE_CURVE('',#5030,#5186,#526,.T.);
#6591=EDGE_CURVE('',#5036,#5187,#527,.T.);
#6592=EDGE_CURVE('',#5188,#5035,#528,.T.);
#6593=EDGE_CURVE('',#5187,#5188,#3213,.T.);
#6594=EDGE_CURVE('',#5189,#5187,#3997,.T.);
#6595=EDGE_CURVE('',#5190,#5188,#3998,.T.);
#6596=EDGE_CURVE('',#5189,#5190,#3214,.T.);
#6597=EDGE_CURVE('',#5041,#5189,#529,.T.);
#6598=EDGE_CURVE('',#5042,#5190,#530,.T.);
#6599=EDGE_CURVE('',#5048,#5191,#531,.T.);
#6600=EDGE_CURVE('',#5192,#5047,#532,.T.);
#6601=EDGE_CURVE('',#5191,#5192,#3215,.T.);
#6602=EDGE_CURVE('',#5193,#5191,#3999,.T.);
#6603=EDGE_CURVE('',#5194,#5192,#4000,.T.);
#6604=EDGE_CURVE('',#5193,#5194,#3216,.T.);
#6605=EDGE_CURVE('',#5053,#5193,#533,.T.);
#6606=EDGE_CURVE('',#5054,#5194,#534,.T.);
#6607=EDGE_CURVE('',#5060,#5195,#535,.T.);
#6608=EDGE_CURVE('',#5196,#5059,#536,.T.);
#6609=EDGE_CURVE('',#5195,#5196,#3217,.T.);
#6610=EDGE_CURVE('',#5197,#5195,#4001,.T.);
#6611=EDGE_CURVE('',#5198,#5196,#4002,.T.);
#6612=EDGE_CURVE('',#5197,#5198,#3218,.T.);
#6613=EDGE_CURVE('',#5065,#5197,#537,.T.);
#6614=EDGE_CURVE('',#5066,#5198,#538,.T.);
#6615=EDGE_CURVE('',#5072,#5199,#539,.T.);
#6616=EDGE_CURVE('',#5200,#5071,#540,.T.);
#6617=EDGE_CURVE('',#5199,#5200,#3219,.T.);
#6618=EDGE_CURVE('',#5201,#5199,#4003,.T.);
#6619=EDGE_CURVE('',#5202,#5200,#4004,.T.);
#6620=EDGE_CURVE('',#5201,#5202,#3220,.T.);
#6621=EDGE_CURVE('',#5077,#5201,#541,.T.);
#6622=EDGE_CURVE('',#5078,#5202,#542,.T.);
#6623=EDGE_CURVE('',#5084,#5203,#543,.T.);
#6624=EDGE_CURVE('',#5204,#5083,#544,.T.);
#6625=EDGE_CURVE('',#5203,#5204,#3221,.T.);
#6626=EDGE_CURVE('',#5205,#5203,#4005,.T.);
#6627=EDGE_CURVE('',#5206,#5204,#4006,.T.);
#6628=EDGE_CURVE('',#5205,#5206,#3222,.T.);
#6629=EDGE_CURVE('',#5089,#5205,#545,.T.);
#6630=EDGE_CURVE('',#5090,#5206,#546,.T.);
#6631=EDGE_CURVE('',#5096,#5207,#547,.T.);
#6632=EDGE_CURVE('',#5208,#5095,#548,.T.);
#6633=EDGE_CURVE('',#5207,#5208,#3223,.T.);
#6634=EDGE_CURVE('',#5209,#5207,#4007,.T.);
#6635=EDGE_CURVE('',#5210,#5208,#4008,.T.);
#6636=EDGE_CURVE('',#5209,#5210,#3224,.T.);
#6637=EDGE_CURVE('',#5101,#5209,#549,.T.);
#6638=EDGE_CURVE('',#5102,#5210,#550,.T.);
#6639=EDGE_CURVE('',#5108,#5211,#551,.T.);
#6640=EDGE_CURVE('',#5212,#5107,#552,.T.);
#6641=EDGE_CURVE('',#5211,#5212,#3225,.T.);
#6642=EDGE_CURVE('',#5213,#5211,#4009,.T.);
#6643=EDGE_CURVE('',#5214,#5212,#4010,.T.);
#6644=EDGE_CURVE('',#5213,#5214,#3226,.T.);
#6645=EDGE_CURVE('',#5113,#5213,#553,.T.);
#6646=EDGE_CURVE('',#5114,#5214,#554,.T.);
#6647=EDGE_CURVE('',#5120,#5215,#555,.T.);
#6648=EDGE_CURVE('',#5216,#5119,#556,.T.);
#6649=EDGE_CURVE('',#5215,#5216,#3227,.T.);
#6650=EDGE_CURVE('',#5217,#5215,#4011,.T.);
#6651=EDGE_CURVE('',#5218,#5216,#4012,.T.);
#6652=EDGE_CURVE('',#5217,#5218,#3228,.T.);
#6653=EDGE_CURVE('',#5125,#5217,#557,.T.);
#6654=EDGE_CURVE('',#5126,#5218,#558,.T.);
#6655=EDGE_CURVE('',#5132,#5219,#559,.T.);
#6656=EDGE_CURVE('',#5220,#5131,#560,.T.);
#6657=EDGE_CURVE('',#5219,#5220,#3229,.T.);
#6658=EDGE_CURVE('',#5221,#5219,#4013,.T.);
#6659=EDGE_CURVE('',#5222,#5220,#4014,.T.);
#6660=EDGE_CURVE('',#5221,#5222,#3230,.T.);
#6661=EDGE_CURVE('',#5137,#5221,#561,.T.);
#6662=EDGE_CURVE('',#5138,#5222,#562,.T.);
#6663=EDGE_CURVE('',#5144,#5223,#563,.T.);
#6664=EDGE_CURVE('',#5224,#5143,#564,.T.);
#6665=EDGE_CURVE('',#5223,#5224,#3231,.T.);
#6666=EDGE_CURVE('',#5225,#5223,#4015,.T.);
#6667=EDGE_CURVE('',#5226,#5224,#4016,.T.);
#6668=EDGE_CURVE('',#5225,#5226,#3232,.T.);
#6669=EDGE_CURVE('',#5149,#5225,#565,.T.);
#6670=EDGE_CURVE('',#5150,#5226,#566,.T.);
#6671=EDGE_CURVE('',#4950,#4941,#4017,.T.);
#6672=EDGE_CURVE('',#4962,#4953,#4018,.T.);
#6673=EDGE_CURVE('',#4974,#4965,#4019,.T.);
#6674=EDGE_CURVE('',#4986,#4977,#4020,.T.);
#6675=EDGE_CURVE('',#4998,#4989,#4021,.T.);
#6676=EDGE_CURVE('',#5010,#5001,#4022,.T.);
#6677=EDGE_CURVE('',#5022,#5013,#4023,.T.);
#6678=EDGE_CURVE('',#5034,#5025,#4024,.T.);
#6679=EDGE_CURVE('',#5046,#5037,#4025,.T.);
#6680=EDGE_CURVE('',#5058,#5049,#4026,.T.);
#6681=EDGE_CURVE('',#5070,#5061,#4027,.T.);
#6682=EDGE_CURVE('',#5082,#5073,#4028,.T.);
#6683=EDGE_CURVE('',#5094,#5085,#4029,.T.);
#6684=EDGE_CURVE('',#5106,#5097,#4030,.T.);
#6685=EDGE_CURVE('',#5118,#5109,#4031,.T.);
#6686=EDGE_CURVE('',#5130,#5121,#4032,.T.);
#6687=EDGE_CURVE('',#5142,#5133,#4033,.T.);
#6688=EDGE_CURVE('',#5227,#5145,#4034,.T.);
#6689=EDGE_CURVE('',#5228,#5227,#4035,.T.);
#6690=EDGE_CURVE('',#5228,#5229,#3233,.T.);
#6691=EDGE_CURVE('',#5229,#5230,#567,.T.);
#6692=EDGE_CURVE('',#5231,#5230,#4036,.T.);
#6693=EDGE_CURVE('',#5232,#5231,#568,.T.);
#6694=EDGE_CURVE('',#5233,#5232,#3234,.T.);
#6695=EDGE_CURVE('',#5234,#5233,#4037,.T.);
#6696=EDGE_CURVE('',#4926,#5234,#4038,.T.);
#6697=EDGE_CURVE('',#4938,#4929,#4039,.T.);
#6698=EDGE_CURVE('',#4923,#5235,#4040,.T.);
#6699=EDGE_CURVE('',#5236,#5235,#4041,.T.);
#6700=EDGE_CURVE('',#5236,#5237,#3235,.T.);
#6701=EDGE_CURVE('',#5237,#5238,#569,.T.);
#6702=EDGE_CURVE('',#5238,#5239,#4042,.T.);
#6703=EDGE_CURVE('',#5239,#5240,#570,.T.);
#6704=EDGE_CURVE('',#5240,#5241,#3236,.T.);
#6705=EDGE_CURVE('',#5242,#5241,#4043,.T.);
#6706=EDGE_CURVE('',#5242,#5148,#4044,.T.);
#6707=EDGE_CURVE('',#5139,#5136,#4045,.T.);
#6708=EDGE_CURVE('',#5127,#5124,#4046,.T.);
#6709=EDGE_CURVE('',#5115,#5112,#4047,.T.);
#6710=EDGE_CURVE('',#5103,#5100,#4048,.T.);
#6711=EDGE_CURVE('',#5091,#5088,#4049,.T.);
#6712=EDGE_CURVE('',#5079,#5076,#4050,.T.);
#6713=EDGE_CURVE('',#5067,#5064,#4051,.T.);
#6714=EDGE_CURVE('',#5055,#5052,#4052,.T.);
#6715=EDGE_CURVE('',#5043,#5040,#4053,.T.);
#6716=EDGE_CURVE('',#5031,#5028,#4054,.T.);
#6717=EDGE_CURVE('',#5019,#5016,#4055,.T.);
#6718=EDGE_CURVE('',#5007,#5004,#4056,.T.);
#6719=EDGE_CURVE('',#4995,#4992,#4057,.T.);
#6720=EDGE_CURVE('',#4983,#4980,#4058,.T.);
#6721=EDGE_CURVE('',#4971,#4968,#4059,.T.);
#6722=EDGE_CURVE('',#4959,#4956,#4060,.T.);
#6723=EDGE_CURVE('',#4947,#4944,#4061,.T.);
#6724=EDGE_CURVE('',#4935,#4932,#4062,.T.);
#6725=EDGE_CURVE('',#5227,#5242,#3237,.T.);
#6726=EDGE_CURVE('',#5241,#5228,#3238,.T.);
#6727=EDGE_CURVE('',#5229,#5240,#3239,.T.);
#6728=EDGE_CURVE('',#5233,#5236,#3240,.T.);
#6729=EDGE_CURVE('',#5235,#5234,#3241,.T.);
#6730=EDGE_CURVE('',#5232,#5237,#3242,.T.);
#6731=EDGE_CURVE('',#5230,#5239,#3243,.T.);
#6732=EDGE_CURVE('',#5231,#5238,#3244,.T.);
#6733=EDGE_CURVE('',#5243,#5243,#4063,.T.);
#6734=EDGE_CURVE('',#5243,#5244,#3245,.T.);
#6735=EDGE_CURVE('',#5244,#5244,#4064,.F.);
#6736=EDGE_CURVE('',#5245,#5245,#4065,.T.);
#6737=EDGE_CURVE('',#5245,#5246,#3246,.T.);
#6738=EDGE_CURVE('',#5246,#5246,#4066,.T.);
#6739=EDGE_CURVE('',#5247,#5248,#4067,.T.);
#6740=EDGE_CURVE('',#5248,#5249,#3247,.T.);
#6741=EDGE_CURVE('',#5249,#5250,#4068,.T.);
#6742=EDGE_CURVE('',#5250,#5247,#3248,.T.);
#6743=EDGE_CURVE('',#5251,#5248,#3249,.T.);
#6744=EDGE_CURVE('',#5252,#5251,#3250,.T.);
#6745=EDGE_CURVE('',#5249,#5252,#3251,.T.);
#6746=EDGE_CURVE('',#5253,#5254,#4069,.T.);
#6747=EDGE_CURVE('',#5254,#5255,#3252,.T.);
#6748=EDGE_CURVE('',#5255,#5256,#4070,.T.);
#6749=EDGE_CURVE('',#5256,#5253,#3253,.T.);
#6750=EDGE_CURVE('',#5254,#5257,#3254,.T.);
#6751=EDGE_CURVE('',#5257,#5258,#3255,.T.);
#6752=EDGE_CURVE('',#5255,#5258,#3256,.T.);
#6753=EDGE_CURVE('',#5259,#5260,#4071,.T.);
#6754=EDGE_CURVE('',#5260,#5261,#3257,.T.);
#6755=EDGE_CURVE('',#5261,#5262,#4072,.T.);
#6756=EDGE_CURVE('',#5262,#5259,#3258,.T.);
#6757=EDGE_CURVE('',#5263,#5260,#3259,.T.);
#6758=EDGE_CURVE('',#5264,#5263,#3260,.T.);
#6759=EDGE_CURVE('',#5261,#5264,#3261,.T.);
#6760=EDGE_CURVE('',#5265,#5266,#4073,.T.);
#6761=EDGE_CURVE('',#5266,#5267,#3262,.T.);
#6762=EDGE_CURVE('',#5267,#5268,#4074,.T.);
#6763=EDGE_CURVE('',#5268,#5265,#3263,.T.);
#6764=EDGE_CURVE('',#5266,#5269,#3264,.T.);
#6765=EDGE_CURVE('',#5269,#5270,#3265,.T.);
#6766=EDGE_CURVE('',#5267,#5270,#3266,.T.);
#6767=EDGE_CURVE('',#5271,#5272,#4075,.T.);
#6768=EDGE_CURVE('',#5272,#5273,#3267,.T.);
#6769=EDGE_CURVE('',#5273,#5274,#4076,.T.);
#6770=EDGE_CURVE('',#5274,#5271,#3268,.T.);
#6771=EDGE_CURVE('',#5275,#5272,#3269,.T.);
#6772=EDGE_CURVE('',#5276,#5275,#3270,.T.);
#6773=EDGE_CURVE('',#5273,#5276,#3271,.T.);
#6774=EDGE_CURVE('',#5277,#5278,#4077,.T.);
#6775=EDGE_CURVE('',#5278,#5279,#3272,.T.);
#6776=EDGE_CURVE('',#5279,#5280,#4078,.T.);
#6777=EDGE_CURVE('',#5280,#5277,#3273,.T.);
#6778=EDGE_CURVE('',#5278,#5281,#3274,.T.);
#6779=EDGE_CURVE('',#5281,#5282,#3275,.T.);
#6780=EDGE_CURVE('',#5279,#5282,#3276,.T.);
#6781=EDGE_CURVE('',#5283,#5284,#4079,.T.);
#6782=EDGE_CURVE('',#5284,#5285,#3277,.T.);
#6783=EDGE_CURVE('',#5285,#5286,#4080,.T.);
#6784=EDGE_CURVE('',#5286,#5283,#3278,.T.);
#6785=EDGE_CURVE('',#5287,#5284,#3279,.T.);
#6786=EDGE_CURVE('',#5288,#5287,#3280,.T.);
#6787=EDGE_CURVE('',#5285,#5288,#3281,.T.);
#6788=EDGE_CURVE('',#5289,#5290,#4081,.T.);
#6789=EDGE_CURVE('',#5290,#5291,#3282,.T.);
#6790=EDGE_CURVE('',#5291,#5292,#4082,.T.);
#6791=EDGE_CURVE('',#5292,#5289,#3283,.T.);
#6792=EDGE_CURVE('',#5290,#5293,#3284,.T.);
#6793=EDGE_CURVE('',#5293,#5294,#3285,.T.);
#6794=EDGE_CURVE('',#5291,#5294,#3286,.T.);
#6795=EDGE_CURVE('',#5295,#5296,#4083,.T.);
#6796=EDGE_CURVE('',#5296,#5297,#3287,.T.);
#6797=EDGE_CURVE('',#5297,#5298,#4084,.T.);
#6798=EDGE_CURVE('',#5298,#5295,#3288,.T.);
#6799=EDGE_CURVE('',#5299,#5296,#3289,.T.);
#6800=EDGE_CURVE('',#5300,#5299,#3290,.T.);
#6801=EDGE_CURVE('',#5297,#5300,#3291,.T.);
#6802=EDGE_CURVE('',#5301,#5302,#4085,.T.);
#6803=EDGE_CURVE('',#5302,#5303,#3292,.T.);
#6804=EDGE_CURVE('',#5303,#5304,#4086,.T.);
#6805=EDGE_CURVE('',#5304,#5301,#3293,.T.);
#6806=EDGE_CURVE('',#5302,#5305,#3294,.T.);
#6807=EDGE_CURVE('',#5305,#5306,#3295,.T.);
#6808=EDGE_CURVE('',#5303,#5306,#3296,.T.);
#6809=EDGE_CURVE('',#5307,#5308,#4087,.T.);
#6810=EDGE_CURVE('',#5308,#5309,#3297,.T.);
#6811=EDGE_CURVE('',#5309,#5310,#4088,.T.);
#6812=EDGE_CURVE('',#5310,#5307,#3298,.T.);
#6813=EDGE_CURVE('',#5311,#5308,#3299,.T.);
#6814=EDGE_CURVE('',#5312,#5311,#3300,.T.);
#6815=EDGE_CURVE('',#5309,#5312,#3301,.T.);
#6816=EDGE_CURVE('',#5313,#5314,#4089,.T.);
#6817=EDGE_CURVE('',#5314,#5315,#3302,.T.);
#6818=EDGE_CURVE('',#5315,#5316,#4090,.T.);
#6819=EDGE_CURVE('',#5316,#5313,#3303,.T.);
#6820=EDGE_CURVE('',#5314,#5317,#3304,.T.);
#6821=EDGE_CURVE('',#5317,#5318,#3305,.T.);
#6822=EDGE_CURVE('',#5315,#5318,#3306,.T.);
#6823=EDGE_CURVE('',#5319,#5320,#4091,.T.);
#6824=EDGE_CURVE('',#5320,#5321,#3307,.T.);
#6825=EDGE_CURVE('',#5321,#5322,#4092,.T.);
#6826=EDGE_CURVE('',#5322,#5319,#3308,.T.);
#6827=EDGE_CURVE('',#5323,#5320,#3309,.T.);
#6828=EDGE_CURVE('',#5324,#5323,#3310,.T.);
#6829=EDGE_CURVE('',#5321,#5324,#3311,.T.);
#6830=EDGE_CURVE('',#5325,#5326,#4093,.T.);
#6831=EDGE_CURVE('',#5326,#5327,#3312,.T.);
#6832=EDGE_CURVE('',#5327,#5328,#4094,.T.);
#6833=EDGE_CURVE('',#5328,#5325,#3313,.T.);
#6834=EDGE_CURVE('',#5326,#5329,#3314,.T.);
#6835=EDGE_CURVE('',#5329,#5330,#3315,.T.);
#6836=EDGE_CURVE('',#5327,#5330,#3316,.T.);
#6837=EDGE_CURVE('',#5331,#5332,#4095,.T.);
#6838=EDGE_CURVE('',#5332,#5333,#3317,.T.);
#6839=EDGE_CURVE('',#5333,#5334,#4096,.T.);
#6840=EDGE_CURVE('',#5334,#5331,#3318,.T.);
#6841=EDGE_CURVE('',#5335,#5332,#3319,.T.);
#6842=EDGE_CURVE('',#5336,#5335,#3320,.T.);
#6843=EDGE_CURVE('',#5333,#5336,#3321,.T.);
#6844=EDGE_CURVE('',#5337,#5338,#4097,.T.);
#6845=EDGE_CURVE('',#5338,#5339,#3322,.T.);
#6846=EDGE_CURVE('',#5339,#5340,#4098,.T.);
#6847=EDGE_CURVE('',#5340,#5337,#3323,.T.);
#6848=EDGE_CURVE('',#5338,#5341,#3324,.T.);
#6849=EDGE_CURVE('',#5341,#5342,#3325,.T.);
#6850=EDGE_CURVE('',#5339,#5342,#3326,.T.);
#6851=EDGE_CURVE('',#5343,#5344,#4099,.T.);
#6852=EDGE_CURVE('',#5344,#5345,#3327,.T.);
#6853=EDGE_CURVE('',#5345,#5346,#4100,.T.);
#6854=EDGE_CURVE('',#5346,#5343,#3328,.T.);
#6855=EDGE_CURVE('',#5347,#5344,#3329,.T.);
#6856=EDGE_CURVE('',#5348,#5347,#3330,.T.);
#6857=EDGE_CURVE('',#5345,#5348,#3331,.T.);
#6858=EDGE_CURVE('',#5349,#5350,#4101,.T.);
#6859=EDGE_CURVE('',#5350,#5351,#3332,.T.);
#6860=EDGE_CURVE('',#5351,#5352,#4102,.T.);
#6861=EDGE_CURVE('',#5352,#5349,#3333,.T.);
#6862=EDGE_CURVE('',#5350,#5353,#3334,.T.);
#6863=EDGE_CURVE('',#5353,#5354,#3335,.T.);
#6864=EDGE_CURVE('',#5351,#5354,#3336,.T.);
#6865=EDGE_CURVE('',#5252,#5355,#571,.T.);
#6866=EDGE_CURVE('',#5356,#5251,#572,.T.);
#6867=EDGE_CURVE('',#5355,#5356,#3337,.T.);
#6868=EDGE_CURVE('',#5357,#5355,#4103,.T.);
#6869=EDGE_CURVE('',#5358,#5356,#4104,.T.);
#6870=EDGE_CURVE('',#5357,#5358,#3338,.T.);
#6871=EDGE_CURVE('',#5257,#5357,#573,.T.);
#6872=EDGE_CURVE('',#5258,#5358,#574,.T.);
#6873=EDGE_CURVE('',#5264,#5359,#575,.T.);
#6874=EDGE_CURVE('',#5360,#5263,#576,.T.);
#6875=EDGE_CURVE('',#5359,#5360,#3339,.T.);
#6876=EDGE_CURVE('',#5361,#5359,#4105,.T.);
#6877=EDGE_CURVE('',#5362,#5360,#4106,.T.);
#6878=EDGE_CURVE('',#5361,#5362,#3340,.T.);
#6879=EDGE_CURVE('',#5269,#5361,#577,.T.);
#6880=EDGE_CURVE('',#5270,#5362,#578,.T.);
#6881=EDGE_CURVE('',#5276,#5363,#579,.T.);
#6882=EDGE_CURVE('',#5364,#5275,#580,.T.);
#6883=EDGE_CURVE('',#5363,#5364,#3341,.T.);
#6884=EDGE_CURVE('',#5365,#5363,#4107,.T.);
#6885=EDGE_CURVE('',#5366,#5364,#4108,.T.);
#6886=EDGE_CURVE('',#5365,#5366,#3342,.T.);
#6887=EDGE_CURVE('',#5281,#5365,#581,.T.);
#6888=EDGE_CURVE('',#5282,#5366,#582,.T.);
#6889=EDGE_CURVE('',#5288,#5367,#583,.T.);
#6890=EDGE_CURVE('',#5368,#5287,#584,.T.);
#6891=EDGE_CURVE('',#5367,#5368,#3343,.T.);
#6892=EDGE_CURVE('',#5369,#5367,#4109,.T.);
#6893=EDGE_CURVE('',#5370,#5368,#4110,.T.);
#6894=EDGE_CURVE('',#5369,#5370,#3344,.T.);
#6895=EDGE_CURVE('',#5293,#5369,#585,.T.);
#6896=EDGE_CURVE('',#5294,#5370,#586,.T.);
#6897=EDGE_CURVE('',#5300,#5371,#587,.T.);
#6898=EDGE_CURVE('',#5372,#5299,#588,.T.);
#6899=EDGE_CURVE('',#5371,#5372,#3345,.T.);
#6900=EDGE_CURVE('',#5373,#5371,#4111,.T.);
#6901=EDGE_CURVE('',#5374,#5372,#4112,.T.);
#6902=EDGE_CURVE('',#5373,#5374,#3346,.T.);
#6903=EDGE_CURVE('',#5305,#5373,#589,.T.);
#6904=EDGE_CURVE('',#5306,#5374,#590,.T.);
#6905=EDGE_CURVE('',#5312,#5375,#591,.T.);
#6906=EDGE_CURVE('',#5376,#5311,#592,.T.);
#6907=EDGE_CURVE('',#5375,#5376,#3347,.T.);
#6908=EDGE_CURVE('',#5377,#5375,#4113,.T.);
#6909=EDGE_CURVE('',#5378,#5376,#4114,.T.);
#6910=EDGE_CURVE('',#5377,#5378,#3348,.T.);
#6911=EDGE_CURVE('',#5317,#5377,#593,.T.);
#6912=EDGE_CURVE('',#5318,#5378,#594,.T.);
#6913=EDGE_CURVE('',#5324,#5379,#595,.T.);
#6914=EDGE_CURVE('',#5380,#5323,#596,.T.);
#6915=EDGE_CURVE('',#5379,#5380,#3349,.T.);
#6916=EDGE_CURVE('',#5381,#5379,#4115,.T.);
#6917=EDGE_CURVE('',#5382,#5380,#4116,.T.);
#6918=EDGE_CURVE('',#5381,#5382,#3350,.T.);
#6919=EDGE_CURVE('',#5329,#5381,#597,.T.);
#6920=EDGE_CURVE('',#5330,#5382,#598,.T.);
#6921=EDGE_CURVE('',#5336,#5383,#599,.T.);
#6922=EDGE_CURVE('',#5384,#5335,#600,.T.);
#6923=EDGE_CURVE('',#5383,#5384,#3351,.T.);
#6924=EDGE_CURVE('',#5385,#5383,#4117,.T.);
#6925=EDGE_CURVE('',#5386,#5384,#4118,.T.);
#6926=EDGE_CURVE('',#5385,#5386,#3352,.T.);
#6927=EDGE_CURVE('',#5341,#5385,#601,.T.);
#6928=EDGE_CURVE('',#5342,#5386,#602,.T.);
#6929=EDGE_CURVE('',#5348,#5387,#603,.T.);
#6930=EDGE_CURVE('',#5388,#5347,#604,.T.);
#6931=EDGE_CURVE('',#5387,#5388,#3353,.T.);
#6932=EDGE_CURVE('',#5389,#5387,#4119,.T.);
#6933=EDGE_CURVE('',#5390,#5388,#4120,.T.);
#6934=EDGE_CURVE('',#5389,#5390,#3354,.T.);
#6935=EDGE_CURVE('',#5353,#5389,#605,.T.);
#6936=EDGE_CURVE('',#5354,#5390,#606,.T.);
#6937=EDGE_CURVE('',#5274,#5265,#4121,.T.);
#6938=EDGE_CURVE('',#5286,#5277,#4122,.T.);
#6939=EDGE_CURVE('',#5298,#5289,#4123,.T.);
#6940=EDGE_CURVE('',#5310,#5301,#4124,.T.);
#6941=EDGE_CURVE('',#5322,#5313,#4125,.T.);
#6942=EDGE_CURVE('',#5334,#5325,#4126,.T.);
#6943=EDGE_CURVE('',#5346,#5337,#4127,.T.);
#6944=EDGE_CURVE('',#5391,#5349,#4128,.T.);
#6945=EDGE_CURVE('',#5392,#5391,#4129,.T.);
#6946=EDGE_CURVE('',#5392,#5393,#3355,.T.);
#6947=EDGE_CURVE('',#5393,#5394,#607,.T.);
#6948=EDGE_CURVE('',#5395,#5394,#4130,.T.);
#6949=EDGE_CURVE('',#5396,#5395,#608,.T.);
#6950=EDGE_CURVE('',#5397,#5396,#3356,.T.);
#6951=EDGE_CURVE('',#5398,#5397,#4131,.T.);
#6952=EDGE_CURVE('',#5250,#5398,#4132,.T.);
#6953=EDGE_CURVE('',#5262,#5253,#4133,.T.);
#6954=EDGE_CURVE('',#5247,#5399,#4134,.T.);
#6955=EDGE_CURVE('',#5400,#5399,#4135,.T.);
#6956=EDGE_CURVE('',#5400,#5401,#3357,.T.);
#6957=EDGE_CURVE('',#5401,#5402,#609,.T.);
#6958=EDGE_CURVE('',#5402,#5403,#4136,.T.);
#6959=EDGE_CURVE('',#5403,#5404,#610,.T.);
#6960=EDGE_CURVE('',#5404,#5405,#3358,.T.);
#6961=EDGE_CURVE('',#5406,#5405,#4137,.T.);
#6962=EDGE_CURVE('',#5406,#5352,#4138,.T.);
#6963=EDGE_CURVE('',#5343,#5340,#4139,.T.);
#6964=EDGE_CURVE('',#5331,#5328,#4140,.T.);
#6965=EDGE_CURVE('',#5319,#5316,#4141,.T.);
#6966=EDGE_CURVE('',#5307,#5304,#4142,.T.);
#6967=EDGE_CURVE('',#5295,#5292,#4143,.T.);
#6968=EDGE_CURVE('',#5283,#5280,#4144,.T.);
#6969=EDGE_CURVE('',#5271,#5268,#4145,.T.);
#6970=EDGE_CURVE('',#5259,#5256,#4146,.T.);
#6971=EDGE_CURVE('',#5391,#5406,#3359,.T.);
#6972=EDGE_CURVE('',#5405,#5392,#3360,.T.);
#6973=EDGE_CURVE('',#5393,#5404,#3361,.T.);
#6974=EDGE_CURVE('',#5397,#5400,#3362,.T.);
#6975=EDGE_CURVE('',#5399,#5398,#3363,.T.);
#6976=EDGE_CURVE('',#5396,#5401,#3364,.T.);
#6977=EDGE_CURVE('',#5394,#5403,#3365,.T.);
#6978=EDGE_CURVE('',#5395,#5402,#3366,.T.);
#6979=EDGE_CURVE('',#5407,#5407,#4147,.T.);
#6980=EDGE_CURVE('',#5407,#5408,#4148,.T.);
#6981=EDGE_CURVE('',#5408,#5408,#4149,.T.);
#6982=EDGE_CURVE('',#5409,#5410,#4150,.T.);
#6983=EDGE_CURVE('',#5410,#5409,#4151,.T.);
#6984=EDGE_CURVE('',#5410,#5411,#4152,.T.);
#6985=EDGE_CURVE('',#5412,#5411,#4153,.T.);
#6986=EDGE_CURVE('',#5411,#5412,#4154,.T.);
#6987=EDGE_CURVE('',#5413,#5414,#4155,.T.);
#6988=EDGE_CURVE('',#5414,#5413,#4156,.T.);
#6989=EDGE_CURVE('',#5414,#5415,#4157,.T.);
#6990=EDGE_CURVE('',#5415,#5415,#4158,.T.);
#6991=EDGE_CURVE('',#5409,#5416,#3367,.T.);
#6992=EDGE_CURVE('',#5416,#5416,#4159,.T.);
#6993=EDGE_CURVE('',#5413,#5412,#3368,.T.);
#6994=EDGE_CURVE('',#5415,#5417,#3369,.T.);
#6995=EDGE_CURVE('',#5417,#5417,#4160,.T.);
#6996=EDGE_CURVE('',#5408,#5418,#3370,.T.);
#6997=EDGE_CURVE('',#5418,#5418,#4161,.T.);
#6998=EDGE_CURVE('',#5419,#5419,#4162,.T.);
#6999=EDGE_CURVE('',#5419,#5407,#3371,.T.);
#7000=EDGE_CURVE('',#5420,#5421,#4163,.T.);
#7001=EDGE_CURVE('',#5422,#5423,#4164,.T.);
#7002=EDGE_CURVE('',#5424,#5425,#4165,.T.);
#7003=EDGE_CURVE('',#5426,#5427,#4166,.T.);
#7004=EDGE_CURVE('',#5428,#5429,#4167,.T.);
#7005=EDGE_CURVE('',#5430,#5431,#4168,.T.);
#7006=EDGE_CURVE('',#5432,#5433,#4169,.T.);
#7007=EDGE_CURVE('',#5434,#5434,#4170,.T.);
#7008=EDGE_CURVE('',#5434,#5435,#4171,.T.);
#7009=EDGE_CURVE('',#5436,#5435,#4172,.T.);
#7010=EDGE_CURVE('',#5435,#5436,#4173,.T.);
#7011=EDGE_CURVE('',#5437,#5437,#4174,.T.);
#7012=EDGE_CURVE('',#5437,#5438,#4175,.T.);
#7013=EDGE_CURVE('',#5438,#5438,#4176,.T.);
#7014=EDGE_CURVE('',#5439,#5439,#4177,.T.);
#7015=EDGE_CURVE('',#5439,#5440,#4178,.T.);
#7016=EDGE_CURVE('',#5440,#5440,#4179,.T.);
#7017=EDGE_CURVE('',#5441,#5442,#4180,.T.);
#7018=EDGE_CURVE('',#5442,#5441,#4181,.T.);
#7019=EDGE_CURVE('',#5442,#5443,#4182,.T.);
#7020=EDGE_CURVE('',#5443,#5443,#4183,.T.);
#7021=EDGE_CURVE('',#5444,#5444,#4184,.T.);
#7022=EDGE_CURVE('',#5444,#5445,#3372,.T.);
#7023=EDGE_CURVE('',#5445,#5445,#4185,.T.);
#7024=EDGE_CURVE('',#5446,#5446,#4186,.T.);
#7025=EDGE_CURVE('',#5446,#5436,#3373,.T.);
#7026=EDGE_CURVE('',#5441,#5447,#3374,.T.);
#7027=EDGE_CURVE('',#5447,#5447,#4187,.T.);
#7028=EDGE_CURVE('',#5447,#5448,#4188,.T.);
#7029=EDGE_CURVE('',#5448,#5448,#4189,.T.);
#7030=EDGE_CURVE('',#5448,#5437,#3375,.T.);
#7031=EDGE_CURVE('',#5440,#5449,#3376,.T.);
#7032=EDGE_CURVE('',#5449,#5449,#4190,.T.);
#7033=EDGE_CURVE('',#5450,#5450,#4191,.T.);
#7034=EDGE_CURVE('',#5450,#5451,#3377,.T.);
#7035=EDGE_CURVE('',#5451,#5451,#4192,.T.);
#7036=EDGE_CURVE('',#5452,#5452,#4193,.T.);
#7037=EDGE_CURVE('',#5452,#5453,#3378,.T.);
#7038=EDGE_CURVE('',#5453,#5453,#4194,.T.);
#7039=EDGE_CURVE('',#5454,#5455,#4195,.T.);
#7040=EDGE_CURVE('',#5455,#5456,#3379,.T.);
#7041=EDGE_CURVE('',#5456,#5456,#4196,.T.);
#7042=EDGE_CURVE('',#5455,#5454,#4197,.T.);
#7043=EDGE_CURVE('',#5454,#5452,#3380,.T.);
#7044=EDGE_CURVE('',#5457,#5457,#4198,.T.);
#7045=EDGE_CURVE('',#5457,#5458,#4199,.T.);
#7046=EDGE_CURVE('',#5458,#5458,#4200,.T.);
#7047=EDGE_CURVE('',#5459,#5460,#611,.T.);
#7048=EDGE_CURVE('',#5459,#5461,#612,.T.);
#7049=EDGE_CURVE('',#5461,#5462,#613,.T.);
#7050=EDGE_CURVE('',#5462,#5460,#614,.T.);
#7051=EDGE_CURVE('',#5463,#5464,#615,.T.);
#7052=EDGE_CURVE('',#5463,#5465,#616,.T.);
#7053=EDGE_CURVE('',#5465,#5466,#617,.T.);
#7054=EDGE_CURVE('',#5466,#5464,#618,.T.);
#7055=EDGE_CURVE('',#5467,#5468,#4201,.T.);
#7056=EDGE_CURVE('',#5468,#5469,#4202,.T.);
#7057=EDGE_CURVE('',#5469,#5470,#4203,.T.);
#7058=EDGE_CURVE('',#5470,#5471,#619,.T.);
#7059=EDGE_CURVE('',#5472,#5471,#4204,.T.);
#7060=EDGE_CURVE('',#5472,#5473,#620,.T.);
#7061=EDGE_CURVE('',#5473,#5469,#4205,.T.);
#7062=EDGE_CURVE('',#5468,#5474,#4206,.T.);
#7063=EDGE_CURVE('',#5474,#5475,#621,.T.);
#7064=EDGE_CURVE('',#5476,#5475,#4207,.T.);
#7065=EDGE_CURVE('',#5476,#5467,#622,.T.);
#7066=EDGE_CURVE('',#5477,#5477,#4208,.T.);
#7067=EDGE_CURVE('',#5478,#5478,#4209,.T.);
#7068=EDGE_CURVE('',#5479,#5479,#4210,.T.);
#7069=EDGE_CURVE('',#5479,#5480,#4211,.T.);
#7070=EDGE_CURVE('',#5480,#5480,#4212,.T.);
#7071=EDGE_CURVE('',#5481,#5482,#623,.T.);
#7072=EDGE_CURVE('',#5481,#5483,#624,.T.);
#7073=EDGE_CURVE('',#5483,#5484,#625,.T.);
#7074=EDGE_CURVE('',#5484,#5482,#626,.T.);
#7075=EDGE_CURVE('',#5485,#5486,#627,.T.);
#7076=EDGE_CURVE('',#5485,#5487,#628,.T.);
#7077=EDGE_CURVE('',#5487,#5488,#629,.T.);
#7078=EDGE_CURVE('',#5488,#5486,#630,.T.);
#7079=EDGE_CURVE('',#5489,#5490,#4213,.T.);
#7080=EDGE_CURVE('',#5490,#5491,#4214,.T.);
#7081=EDGE_CURVE('',#5491,#5492,#4215,.T.);
#7082=EDGE_CURVE('',#5492,#5493,#631,.T.);
#7083=EDGE_CURVE('',#5494,#5493,#4216,.T.);
#7084=EDGE_CURVE('',#5494,#5495,#632,.T.);
#7085=EDGE_CURVE('',#5495,#5491,#4217,.T.);
#7086=EDGE_CURVE('',#5490,#5496,#4218,.T.);
#7087=EDGE_CURVE('',#5496,#5497,#633,.T.);
#7088=EDGE_CURVE('',#5498,#5497,#4219,.T.);
#7089=EDGE_CURVE('',#5498,#5489,#634,.T.);
#7090=EDGE_CURVE('',#5499,#5499,#4220,.T.);
#7091=EDGE_CURVE('',#5500,#5500,#4221,.T.);
#7092=EDGE_CURVE('',#5501,#5501,#4222,.T.);
#7093=EDGE_CURVE('',#5501,#5502,#4223,.T.);
#7094=EDGE_CURVE('',#5502,#5502,#4224,.T.);
#7095=EDGE_CURVE('',#5503,#5504,#635,.T.);
#7096=EDGE_CURVE('',#5503,#5505,#636,.T.);
#7097=EDGE_CURVE('',#5505,#5506,#637,.T.);
#7098=EDGE_CURVE('',#5506,#5504,#638,.T.);
#7099=EDGE_CURVE('',#5507,#5508,#639,.T.);
#7100=EDGE_CURVE('',#5507,#5509,#640,.T.);
#7101=EDGE_CURVE('',#5509,#5510,#641,.T.);
#7102=EDGE_CURVE('',#5510,#5508,#642,.T.);
#7103=EDGE_CURVE('',#5511,#5512,#4225,.T.);
#7104=EDGE_CURVE('',#5512,#5513,#4226,.T.);
#7105=EDGE_CURVE('',#5513,#5514,#4227,.T.);
#7106=EDGE_CURVE('',#5514,#5515,#643,.T.);
#7107=EDGE_CURVE('',#5516,#5515,#4228,.T.);
#7108=EDGE_CURVE('',#5516,#5517,#644,.T.);
#7109=EDGE_CURVE('',#5517,#5513,#4229,.T.);
#7110=EDGE_CURVE('',#5512,#5518,#4230,.T.);
#7111=EDGE_CURVE('',#5518,#5519,#645,.T.);
#7112=EDGE_CURVE('',#5520,#5519,#4231,.T.);
#7113=EDGE_CURVE('',#5520,#5511,#646,.T.);
#7114=EDGE_CURVE('',#5521,#5521,#4232,.T.);
#7115=EDGE_CURVE('',#5522,#5522,#4233,.T.);
#7116=EDGE_CURVE('',#5523,#5523,#4234,.T.);
#7117=EDGE_CURVE('',#5523,#5524,#4235,.T.);
#7118=EDGE_CURVE('',#5524,#5524,#4236,.T.);
#7119=EDGE_CURVE('',#5525,#5526,#647,.T.);
#7120=EDGE_CURVE('',#5525,#5527,#648,.T.);
#7121=EDGE_CURVE('',#5527,#5528,#649,.T.);
#7122=EDGE_CURVE('',#5528,#5526,#650,.T.);
#7123=EDGE_CURVE('',#5529,#5530,#651,.T.);
#7124=EDGE_CURVE('',#5529,#5531,#652,.T.);
#7125=EDGE_CURVE('',#5531,#5532,#653,.T.);
#7126=EDGE_CURVE('',#5532,#5530,#654,.T.);
#7127=EDGE_CURVE('',#5533,#5534,#4237,.T.);
#7128=EDGE_CURVE('',#5534,#5535,#4238,.T.);
#7129=EDGE_CURVE('',#5535,#5536,#4239,.T.);
#7130=EDGE_CURVE('',#5536,#5537,#655,.T.);
#7131=EDGE_CURVE('',#5538,#5537,#4240,.T.);
#7132=EDGE_CURVE('',#5538,#5539,#656,.T.);
#7133=EDGE_CURVE('',#5539,#5535,#4241,.T.);
#7134=EDGE_CURVE('',#5534,#5540,#4242,.T.);
#7135=EDGE_CURVE('',#5540,#5541,#657,.T.);
#7136=EDGE_CURVE('',#5542,#5541,#4243,.T.);
#7137=EDGE_CURVE('',#5542,#5533,#658,.T.);
#7138=EDGE_CURVE('',#5543,#5543,#4244,.T.);
#7139=EDGE_CURVE('',#5544,#5544,#4245,.T.);
#7140=EDGE_CURVE('',#5545,#5545,#4246,.T.);
#7141=EDGE_CURVE('',#5545,#5546,#4247,.T.);
#7142=EDGE_CURVE('',#5546,#5546,#4248,.T.);
#7143=EDGE_CURVE('',#5547,#5548,#659,.T.);
#7144=EDGE_CURVE('',#5547,#5549,#660,.T.);
#7145=EDGE_CURVE('',#5549,#5550,#661,.T.);
#7146=EDGE_CURVE('',#5550,#5548,#662,.T.);
#7147=EDGE_CURVE('',#5551,#5552,#663,.T.);
#7148=EDGE_CURVE('',#5551,#5553,#664,.T.);
#7149=EDGE_CURVE('',#5553,#5554,#665,.T.);
#7150=EDGE_CURVE('',#5554,#5552,#666,.T.);
#7151=EDGE_CURVE('',#5555,#5556,#4249,.T.);
#7152=EDGE_CURVE('',#5556,#5557,#4250,.T.);
#7153=EDGE_CURVE('',#5557,#5558,#4251,.T.);
#7154=EDGE_CURVE('',#5558,#5559,#667,.T.);
#7155=EDGE_CURVE('',#5560,#5559,#4252,.T.);
#7156=EDGE_CURVE('',#5560,#5561,#668,.T.);
#7157=EDGE_CURVE('',#5561,#5557,#4253,.T.);
#7158=EDGE_CURVE('',#5556,#5562,#4254,.T.);
#7159=EDGE_CURVE('',#5562,#5563,#669,.T.);
#7160=EDGE_CURVE('',#5564,#5563,#4255,.T.);
#7161=EDGE_CURVE('',#5564,#5555,#670,.T.);
#7162=EDGE_CURVE('',#5565,#5565,#4256,.T.);
#7163=EDGE_CURVE('',#5566,#5566,#4257,.T.);
#7164=EDGE_CURVE('',#5567,#5567,#4258,.T.);
#7165=EDGE_CURVE('',#5567,#5568,#4259,.T.);
#7166=EDGE_CURVE('',#5568,#5568,#4260,.T.);
#7167=EDGE_CURVE('',#5569,#5570,#671,.T.);
#7168=EDGE_CURVE('',#5569,#5571,#672,.T.);
#7169=EDGE_CURVE('',#5572,#5571,#673,.T.);
#7170=EDGE_CURVE('',#5570,#5572,#674,.T.);
#7171=EDGE_CURVE('',#5573,#5574,#675,.T.);
#7172=EDGE_CURVE('',#5573,#5575,#676,.T.);
#7173=EDGE_CURVE('',#5575,#5576,#677,.T.);
#7174=EDGE_CURVE('',#5576,#5574,#678,.T.);
#7175=EDGE_CURVE('',#5577,#5578,#4261,.T.);
#7176=EDGE_CURVE('',#5579,#5577,#679,.T.);
#7177=EDGE_CURVE('',#5579,#5580,#4262,.T.);
#7178=EDGE_CURVE('',#5581,#5580,#680,.T.);
#7179=EDGE_CURVE('',#5578,#5581,#4263,.T.);
#7180=EDGE_CURVE('',#5578,#5582,#4264,.T.);
#7181=EDGE_CURVE('',#5582,#5583,#4265,.T.);
#7182=EDGE_CURVE('',#5583,#5584,#681,.T.);
#7183=EDGE_CURVE('',#5585,#5584,#4266,.T.);
#7184=EDGE_CURVE('',#5585,#5586,#682,.T.);
#7185=EDGE_CURVE('',#5586,#5582,#4267,.T.);
#7186=EDGE_CURVE('',#5587,#5587,#4268,.T.);
#7187=EDGE_CURVE('',#5588,#5588,#4269,.T.);
#7188=EDGE_CURVE('',#5589,#5590,#4270,.T.);
#7189=EDGE_CURVE('',#5590,#5591,#4271,.T.);
#7190=EDGE_CURVE('',#5591,#5592,#4272,.T.);
#7191=EDGE_CURVE('',#5592,#5593,#683,.T.);
#7192=EDGE_CURVE('',#5594,#5593,#4273,.T.);
#7193=EDGE_CURVE('',#5594,#5595,#684,.T.);
#7194=EDGE_CURVE('',#5595,#5591,#4274,.T.);
#7195=EDGE_CURVE('',#5590,#5596,#4275,.T.);
#7196=EDGE_CURVE('',#5596,#5597,#685,.T.);
#7197=EDGE_CURVE('',#5598,#5597,#4276,.T.);
#7198=EDGE_CURVE('',#5598,#5589,#686,.T.);
#7199=EDGE_CURVE('',#5599,#5599,#4277,.T.);
#7200=EDGE_CURVE('',#5600,#5600,#4278,.T.);
#7201=EDGE_CURVE('',#5601,#5601,#4279,.T.);
#7202=EDGE_CURVE('',#5601,#5602,#4280,.T.);
#7203=EDGE_CURVE('',#5602,#5602,#4281,.T.);
#7204=EDGE_CURVE('',#5603,#5604,#687,.T.);
#7205=EDGE_CURVE('',#5603,#5605,#688,.T.);
#7206=EDGE_CURVE('',#5605,#5606,#689,.T.);
#7207=EDGE_CURVE('',#5606,#5604,#690,.T.);
#7208=EDGE_CURVE('',#5607,#5608,#691,.T.);
#7209=EDGE_CURVE('',#5607,#5609,#692,.T.);
#7210=EDGE_CURVE('',#5609,#5610,#693,.T.);
#7211=EDGE_CURVE('',#5610,#5608,#694,.T.);
#7212=EDGE_CURVE('',#5610,#5572,#4282,.T.);
#7213=EDGE_CURVE('',#5608,#5571,#4283,.T.);
#7214=EDGE_CURVE('',#5569,#5607,#4284,.T.);
#7215=EDGE_CURVE('',#5570,#5609,#4285,.T.);
#7216=EDGE_CURVE('',#5597,#5594,#4286,.T.);
#7217=EDGE_CURVE('',#5593,#5598,#4287,.T.);
#7218=EDGE_CURVE('',#5596,#5595,#4288,.T.);
#7219=EDGE_CURVE('',#5592,#5589,#4289,.T.);
#7220=EDGE_CURVE('',#5576,#5549,#4290,.T.);
#7221=EDGE_CURVE('',#5550,#5575,#4291,.T.);
#7222=EDGE_CURVE('',#5574,#5547,#4292,.T.);
#7223=EDGE_CURVE('',#5548,#5573,#4293,.T.);
#7224=EDGE_CURVE('',#5563,#5560,#4294,.T.);
#7225=EDGE_CURVE('',#5562,#5561,#4295,.T.);
#7226=EDGE_CURVE('',#5558,#5555,#4296,.T.);
#7227=EDGE_CURVE('',#5559,#5564,#4297,.T.);
#7228=EDGE_CURVE('',#5554,#5527,#4298,.T.);
#7229=EDGE_CURVE('',#5528,#5553,#4299,.T.);
#7230=EDGE_CURVE('',#5552,#5525,#4300,.T.);
#7231=EDGE_CURVE('',#5526,#5551,#4301,.T.);
#7232=EDGE_CURVE('',#5541,#5538,#4302,.T.);
#7233=EDGE_CURVE('',#5540,#5539,#4303,.T.);
#7234=EDGE_CURVE('',#5536,#5533,#4304,.T.);
#7235=EDGE_CURVE('',#5537,#5542,#4305,.T.);
#7236=EDGE_CURVE('',#5532,#5505,#4306,.T.);
#7237=EDGE_CURVE('',#5506,#5531,#4307,.T.);
#7238=EDGE_CURVE('',#5530,#5503,#4308,.T.);
#7239=EDGE_CURVE('',#5504,#5529,#4309,.T.);
#7240=EDGE_CURVE('',#5519,#5516,#4310,.T.);
#7241=EDGE_CURVE('',#5518,#5517,#4311,.T.);
#7242=EDGE_CURVE('',#5514,#5511,#4312,.T.);
#7243=EDGE_CURVE('',#5515,#5520,#4313,.T.);
#7244=EDGE_CURVE('',#5510,#5483,#4314,.T.);
#7245=EDGE_CURVE('',#5484,#5509,#4315,.T.);
#7246=EDGE_CURVE('',#5508,#5481,#4316,.T.);
#7247=EDGE_CURVE('',#5482,#5507,#4317,.T.);
#7248=EDGE_CURVE('',#5497,#5494,#4318,.T.);
#7249=EDGE_CURVE('',#5496,#5495,#4319,.T.);
#7250=EDGE_CURVE('',#5492,#5489,#4320,.T.);
#7251=EDGE_CURVE('',#5493,#5498,#4321,.T.);
#7252=EDGE_CURVE('',#5488,#5461,#4322,.T.);
#7253=EDGE_CURVE('',#5462,#5487,#4323,.T.);
#7254=EDGE_CURVE('',#5486,#5459,#4324,.T.);
#7255=EDGE_CURVE('',#5460,#5485,#4325,.T.);
#7256=EDGE_CURVE('',#5475,#5472,#4326,.T.);
#7257=EDGE_CURVE('',#5474,#5473,#4327,.T.);
#7258=EDGE_CURVE('',#5470,#5467,#4328,.T.);
#7259=EDGE_CURVE('',#5471,#5476,#4329,.T.);
#7260=EDGE_CURVE('',#5466,#5605,#4330,.T.);
#7261=EDGE_CURVE('',#5606,#5465,#4331,.T.);
#7262=EDGE_CURVE('',#5464,#5603,#4332,.T.);
#7263=EDGE_CURVE('',#5604,#5463,#4333,.T.);
#7264=EDGE_CURVE('',#5579,#5585,#4334,.T.);
#7265=EDGE_CURVE('',#5584,#5580,#4335,.T.);
#7266=EDGE_CURVE('',#5577,#5586,#4336,.T.);
#7267=EDGE_CURVE('',#5583,#5581,#4337,.T.);
#7268=EDGE_CURVE('',#5611,#5611,#4338,.T.);
#7269=EDGE_CURVE('',#5611,#5612,#4339,.T.);
#7270=EDGE_CURVE('',#5612,#5612,#4340,.T.);
#7271=EDGE_CURVE('',#5613,#5614,#4341,.T.);
#7272=EDGE_CURVE('',#5614,#5613,#4342,.T.);
#7273=EDGE_CURVE('',#5614,#5615,#4343,.T.);
#7274=EDGE_CURVE('',#5616,#5615,#4344,.T.);
#7275=EDGE_CURVE('',#5615,#5616,#4345,.T.);
#7276=EDGE_CURVE('',#5617,#5618,#4346,.T.);
#7277=EDGE_CURVE('',#5618,#5617,#4347,.T.);
#7278=EDGE_CURVE('',#5618,#5619,#4348,.T.);
#7279=EDGE_CURVE('',#5619,#5619,#4349,.T.);
#7280=EDGE_CURVE('',#5613,#5620,#3381,.T.);
#7281=EDGE_CURVE('',#5620,#5620,#4350,.T.);
#7282=EDGE_CURVE('',#5617,#5616,#3382,.T.);
#7283=EDGE_CURVE('',#5619,#5621,#3383,.T.);
#7284=EDGE_CURVE('',#5621,#5621,#4351,.T.);
#7285=EDGE_CURVE('',#5612,#5622,#3384,.T.);
#7286=EDGE_CURVE('',#5622,#5622,#4352,.T.);
#7287=EDGE_CURVE('',#5623,#5623,#4353,.T.);
#7288=EDGE_CURVE('',#5623,#5611,#3385,.T.);
#7289=EDGE_CURVE('',#5624,#5625,#4354,.T.);
#7290=EDGE_CURVE('',#5626,#5627,#4355,.T.);
#7291=EDGE_CURVE('',#5628,#5629,#4356,.T.);
#7292=EDGE_CURVE('',#5630,#5631,#4357,.T.);
#7293=EDGE_CURVE('',#5632,#5633,#4358,.T.);
#7294=EDGE_CURVE('',#5634,#5635,#4359,.T.);
#7295=EDGE_CURVE('',#5636,#5637,#4360,.T.);
#7296=EDGE_CURVE('',#5638,#5638,#4361,.T.);
#7297=EDGE_CURVE('',#5638,#5639,#4362,.T.);
#7298=EDGE_CURVE('',#5640,#5639,#4363,.T.);
#7299=EDGE_CURVE('',#5639,#5640,#4364,.T.);
#7300=EDGE_CURVE('',#5641,#5641,#4365,.T.);
#7301=EDGE_CURVE('',#5641,#5642,#4366,.T.);
#7302=EDGE_CURVE('',#5642,#5642,#4367,.T.);
#7303=EDGE_CURVE('',#5643,#5643,#4368,.T.);
#7304=EDGE_CURVE('',#5643,#5644,#4369,.T.);
#7305=EDGE_CURVE('',#5644,#5644,#4370,.T.);
#7306=EDGE_CURVE('',#5645,#5646,#4371,.T.);
#7307=EDGE_CURVE('',#5646,#5645,#4372,.T.);
#7308=EDGE_CURVE('',#5646,#5647,#4373,.T.);
#7309=EDGE_CURVE('',#5647,#5647,#4374,.T.);
#7310=EDGE_CURVE('',#5648,#5648,#4375,.T.);
#7311=EDGE_CURVE('',#5648,#5649,#3386,.T.);
#7312=EDGE_CURVE('',#5649,#5649,#4376,.T.);
#7313=EDGE_CURVE('',#5650,#5650,#4377,.T.);
#7314=EDGE_CURVE('',#5650,#5640,#3387,.T.);
#7315=EDGE_CURVE('',#5645,#5651,#3388,.T.);
#7316=EDGE_CURVE('',#5651,#5651,#4378,.T.);
#7317=EDGE_CURVE('',#5651,#5652,#4379,.T.);
#7318=EDGE_CURVE('',#5652,#5652,#4380,.T.);
#7319=EDGE_CURVE('',#5652,#5641,#3389,.T.);
#7320=EDGE_CURVE('',#5644,#5653,#3390,.T.);
#7321=EDGE_CURVE('',#5653,#5653,#4381,.T.);
#7322=EDGE_CURVE('',#5654,#5654,#4382,.T.);
#7323=EDGE_CURVE('',#5654,#5655,#3391,.T.);
#7324=EDGE_CURVE('',#5655,#5655,#4383,.T.);
#7325=EDGE_CURVE('',#5656,#5656,#4384,.T.);
#7326=EDGE_CURVE('',#5656,#5657,#3392,.T.);
#7327=EDGE_CURVE('',#5657,#5657,#4385,.T.);
#7328=EDGE_CURVE('',#5658,#5659,#4386,.T.);
#7329=EDGE_CURVE('',#5659,#5660,#3393,.T.);
#7330=EDGE_CURVE('',#5660,#5660,#4387,.T.);
#7331=EDGE_CURVE('',#5659,#5658,#4388,.T.);
#7332=EDGE_CURVE('',#5658,#5656,#3394,.T.);
#7333=EDGE_CURVE('',#5661,#5661,#4389,.T.);
#7334=EDGE_CURVE('',#5661,#5662,#4390,.T.);
#7335=EDGE_CURVE('',#5662,#5662,#4391,.T.);
#7336=EDGE_CURVE('',#5663,#5664,#695,.T.);
#7337=EDGE_CURVE('',#5663,#5665,#696,.T.);
#7338=EDGE_CURVE('',#5665,#5666,#697,.T.);
#7339=EDGE_CURVE('',#5666,#5664,#698,.T.);
#7340=EDGE_CURVE('',#5667,#5668,#699,.T.);
#7341=EDGE_CURVE('',#5667,#5669,#700,.T.);
#7342=EDGE_CURVE('',#5669,#5670,#701,.T.);
#7343=EDGE_CURVE('',#5670,#5668,#702,.T.);
#7344=EDGE_CURVE('',#5671,#5672,#4392,.T.);
#7345=EDGE_CURVE('',#5672,#5673,#4393,.T.);
#7346=EDGE_CURVE('',#5673,#5674,#4394,.T.);
#7347=EDGE_CURVE('',#5674,#5675,#703,.T.);
#7348=EDGE_CURVE('',#5676,#5675,#4395,.T.);
#7349=EDGE_CURVE('',#5676,#5677,#704,.T.);
#7350=EDGE_CURVE('',#5677,#5673,#4396,.T.);
#7351=EDGE_CURVE('',#5672,#5678,#4397,.T.);
#7352=EDGE_CURVE('',#5678,#5679,#705,.T.);
#7353=EDGE_CURVE('',#5680,#5679,#4398,.T.);
#7354=EDGE_CURVE('',#5680,#5671,#706,.T.);
#7355=EDGE_CURVE('',#5681,#5681,#4399,.T.);
#7356=EDGE_CURVE('',#5682,#5682,#4400,.T.);
#7357=EDGE_CURVE('',#5683,#5683,#4401,.T.);
#7358=EDGE_CURVE('',#5683,#5684,#4402,.T.);
#7359=EDGE_CURVE('',#5684,#5684,#4403,.T.);
#7360=EDGE_CURVE('',#5685,#5686,#707,.T.);
#7361=EDGE_CURVE('',#5685,#5687,#708,.T.);
#7362=EDGE_CURVE('',#5687,#5688,#709,.T.);
#7363=EDGE_CURVE('',#5688,#5686,#710,.T.);
#7364=EDGE_CURVE('',#5689,#5690,#711,.T.);
#7365=EDGE_CURVE('',#5689,#5691,#712,.T.);
#7366=EDGE_CURVE('',#5691,#5692,#713,.T.);
#7367=EDGE_CURVE('',#5692,#5690,#714,.T.);
#7368=EDGE_CURVE('',#5693,#5694,#4404,.T.);
#7369=EDGE_CURVE('',#5694,#5695,#4405,.T.);
#7370=EDGE_CURVE('',#5695,#5696,#4406,.T.);
#7371=EDGE_CURVE('',#5696,#5697,#715,.T.);
#7372=EDGE_CURVE('',#5698,#5697,#4407,.T.);
#7373=EDGE_CURVE('',#5698,#5699,#716,.T.);
#7374=EDGE_CURVE('',#5699,#5695,#4408,.T.);
#7375=EDGE_CURVE('',#5694,#5700,#4409,.T.);
#7376=EDGE_CURVE('',#5700,#5701,#717,.T.);
#7377=EDGE_CURVE('',#5702,#5701,#4410,.T.);
#7378=EDGE_CURVE('',#5702,#5693,#718,.T.);
#7379=EDGE_CURVE('',#5703,#5703,#4411,.T.);
#7380=EDGE_CURVE('',#5704,#5704,#4412,.T.);
#7381=EDGE_CURVE('',#5705,#5705,#4413,.T.);
#7382=EDGE_CURVE('',#5705,#5706,#4414,.T.);
#7383=EDGE_CURVE('',#5706,#5706,#4415,.T.);
#7384=EDGE_CURVE('',#5707,#5708,#719,.T.);
#7385=EDGE_CURVE('',#5707,#5709,#720,.T.);
#7386=EDGE_CURVE('',#5709,#5710,#721,.T.);
#7387=EDGE_CURVE('',#5710,#5708,#722,.T.);
#7388=EDGE_CURVE('',#5711,#5712,#723,.T.);
#7389=EDGE_CURVE('',#5711,#5713,#724,.T.);
#7390=EDGE_CURVE('',#5713,#5714,#725,.T.);
#7391=EDGE_CURVE('',#5714,#5712,#726,.T.);
#7392=EDGE_CURVE('',#5715,#5716,#4416,.T.);
#7393=EDGE_CURVE('',#5716,#5717,#4417,.T.);
#7394=EDGE_CURVE('',#5717,#5718,#4418,.T.);
#7395=EDGE_CURVE('',#5718,#5719,#727,.T.);
#7396=EDGE_CURVE('',#5720,#5719,#4419,.T.);
#7397=EDGE_CURVE('',#5720,#5721,#728,.T.);
#7398=EDGE_CURVE('',#5721,#5717,#4420,.T.);
#7399=EDGE_CURVE('',#5716,#5722,#4421,.T.);
#7400=EDGE_CURVE('',#5722,#5723,#729,.T.);
#7401=EDGE_CURVE('',#5724,#5723,#4422,.T.);
#7402=EDGE_CURVE('',#5724,#5715,#730,.T.);
#7403=EDGE_CURVE('',#5725,#5725,#4423,.T.);
#7404=EDGE_CURVE('',#5726,#5726,#4424,.T.);
#7405=EDGE_CURVE('',#5727,#5727,#4425,.T.);
#7406=EDGE_CURVE('',#5727,#5728,#4426,.T.);
#7407=EDGE_CURVE('',#5728,#5728,#4427,.T.);
#7408=EDGE_CURVE('',#5729,#5730,#731,.T.);
#7409=EDGE_CURVE('',#5729,#5731,#732,.T.);
#7410=EDGE_CURVE('',#5731,#5732,#733,.T.);
#7411=EDGE_CURVE('',#5732,#5730,#734,.T.);
#7412=EDGE_CURVE('',#5733,#5734,#735,.T.);
#7413=EDGE_CURVE('',#5733,#5735,#736,.T.);
#7414=EDGE_CURVE('',#5735,#5736,#737,.T.);
#7415=EDGE_CURVE('',#5736,#5734,#738,.T.);
#7416=EDGE_CURVE('',#5737,#5738,#4428,.T.);
#7417=EDGE_CURVE('',#5738,#5739,#4429,.T.);
#7418=EDGE_CURVE('',#5739,#5740,#4430,.T.);
#7419=EDGE_CURVE('',#5740,#5741,#739,.T.);
#7420=EDGE_CURVE('',#5742,#5741,#4431,.T.);
#7421=EDGE_CURVE('',#5742,#5743,#740,.T.);
#7422=EDGE_CURVE('',#5743,#5739,#4432,.T.);
#7423=EDGE_CURVE('',#5738,#5744,#4433,.T.);
#7424=EDGE_CURVE('',#5744,#5745,#741,.T.);
#7425=EDGE_CURVE('',#5746,#5745,#4434,.T.);
#7426=EDGE_CURVE('',#5746,#5737,#742,.T.);
#7427=EDGE_CURVE('',#5747,#5747,#4435,.T.);
#7428=EDGE_CURVE('',#5748,#5748,#4436,.T.);
#7429=EDGE_CURVE('',#5749,#5749,#4437,.T.);
#7430=EDGE_CURVE('',#5749,#5750,#4438,.T.);
#7431=EDGE_CURVE('',#5750,#5750,#4439,.T.);
#7432=EDGE_CURVE('',#5751,#5752,#743,.T.);
#7433=EDGE_CURVE('',#5751,#5753,#744,.T.);
#7434=EDGE_CURVE('',#5753,#5754,#745,.T.);
#7435=EDGE_CURVE('',#5754,#5752,#746,.T.);
#7436=EDGE_CURVE('',#5755,#5756,#747,.T.);
#7437=EDGE_CURVE('',#5755,#5757,#748,.T.);
#7438=EDGE_CURVE('',#5757,#5758,#749,.T.);
#7439=EDGE_CURVE('',#5758,#5756,#750,.T.);
#7440=EDGE_CURVE('',#5759,#5760,#4440,.T.);
#7441=EDGE_CURVE('',#5760,#5761,#4441,.T.);
#7442=EDGE_CURVE('',#5761,#5762,#4442,.T.);
#7443=EDGE_CURVE('',#5762,#5763,#751,.T.);
#7444=EDGE_CURVE('',#5764,#5763,#4443,.T.);
#7445=EDGE_CURVE('',#5764,#5765,#752,.T.);
#7446=EDGE_CURVE('',#5765,#5761,#4444,.T.);
#7447=EDGE_CURVE('',#5760,#5766,#4445,.T.);
#7448=EDGE_CURVE('',#5766,#5767,#753,.T.);
#7449=EDGE_CURVE('',#5768,#5767,#4446,.T.);
#7450=EDGE_CURVE('',#5768,#5759,#754,.T.);
#7451=EDGE_CURVE('',#5769,#5769,#4447,.T.);
#7452=EDGE_CURVE('',#5770,#5770,#4448,.T.);
#7453=EDGE_CURVE('',#5771,#5771,#4449,.T.);
#7454=EDGE_CURVE('',#5771,#5772,#4450,.T.);
#7455=EDGE_CURVE('',#5772,#5772,#4451,.T.);
#7456=EDGE_CURVE('',#5773,#5774,#755,.T.);
#7457=EDGE_CURVE('',#5773,#5775,#756,.T.);
#7458=EDGE_CURVE('',#5776,#5775,#757,.T.);
#7459=EDGE_CURVE('',#5774,#5776,#758,.T.);
#7460=EDGE_CURVE('',#5777,#5778,#759,.T.);
#7461=EDGE_CURVE('',#5777,#5779,#760,.T.);
#7462=EDGE_CURVE('',#5779,#5780,#761,.T.);
#7463=EDGE_CURVE('',#5780,#5778,#762,.T.);
#7464=EDGE_CURVE('',#5781,#5782,#4452,.T.);
#7465=EDGE_CURVE('',#5783,#5781,#763,.T.);
#7466=EDGE_CURVE('',#5783,#5784,#4453,.T.);
#7467=EDGE_CURVE('',#5785,#5784,#764,.T.);
#7468=EDGE_CURVE('',#5782,#5785,#4454,.T.);
#7469=EDGE_CURVE('',#5782,#5786,#4455,.T.);
#7470=EDGE_CURVE('',#5786,#5787,#4456,.T.);
#7471=EDGE_CURVE('',#5787,#5788,#765,.T.);
#7472=EDGE_CURVE('',#5789,#5788,#4457,.T.);
#7473=EDGE_CURVE('',#5789,#5790,#766,.T.);
#7474=EDGE_CURVE('',#5790,#5786,#4458,.T.);
#7475=EDGE_CURVE('',#5791,#5791,#4459,.T.);
#7476=EDGE_CURVE('',#5792,#5792,#4460,.T.);
#7477=EDGE_CURVE('',#5793,#5794,#4461,.T.);
#7478=EDGE_CURVE('',#5794,#5795,#4462,.T.);
#7479=EDGE_CURVE('',#5795,#5796,#4463,.T.);
#7480=EDGE_CURVE('',#5796,#5797,#767,.T.);
#7481=EDGE_CURVE('',#5798,#5797,#4464,.T.);
#7482=EDGE_CURVE('',#5798,#5799,#768,.T.);
#7483=EDGE_CURVE('',#5799,#5795,#4465,.T.);
#7484=EDGE_CURVE('',#5794,#5800,#4466,.T.);
#7485=EDGE_CURVE('',#5800,#5801,#769,.T.);
#7486=EDGE_CURVE('',#5802,#5801,#4467,.T.);
#7487=EDGE_CURVE('',#5802,#5793,#770,.T.);
#7488=EDGE_CURVE('',#5803,#5803,#4468,.T.);
#7489=EDGE_CURVE('',#5804,#5804,#4469,.T.);
#7490=EDGE_CURVE('',#5805,#5805,#4470,.T.);
#7491=EDGE_CURVE('',#5805,#5806,#4471,.T.);
#7492=EDGE_CURVE('',#5806,#5806,#4472,.T.);
#7493=EDGE_CURVE('',#5807,#5808,#771,.T.);
#7494=EDGE_CURVE('',#5807,#5809,#772,.T.);
#7495=EDGE_CURVE('',#5809,#5810,#773,.T.);
#7496=EDGE_CURVE('',#5810,#5808,#774,.T.);
#7497=EDGE_CURVE('',#5811,#5812,#775,.T.);
#7498=EDGE_CURVE('',#5811,#5813,#776,.T.);
#7499=EDGE_CURVE('',#5813,#5814,#777,.T.);
#7500=EDGE_CURVE('',#5814,#5812,#778,.T.);
#7501=EDGE_CURVE('',#5814,#5776,#4473,.T.);
#7502=EDGE_CURVE('',#5812,#5775,#4474,.T.);
#7503=EDGE_CURVE('',#5773,#5811,#4475,.T.);
#7504=EDGE_CURVE('',#5774,#5813,#4476,.T.);
#7505=EDGE_CURVE('',#5801,#5798,#4477,.T.);
#7506=EDGE_CURVE('',#5797,#5802,#4478,.T.);
#7507=EDGE_CURVE('',#5800,#5799,#4479,.T.);
#7508=EDGE_CURVE('',#5796,#5793,#4480,.T.);
#7509=EDGE_CURVE('',#5780,#5753,#4481,.T.);
#7510=EDGE_CURVE('',#5754,#5779,#4482,.T.);
#7511=EDGE_CURVE('',#5778,#5751,#4483,.T.);
#7512=EDGE_CURVE('',#5752,#5777,#4484,.T.);
#7513=EDGE_CURVE('',#5767,#5764,#4485,.T.);
#7514=EDGE_CURVE('',#5766,#5765,#4486,.T.);
#7515=EDGE_CURVE('',#5762,#5759,#4487,.T.);
#7516=EDGE_CURVE('',#5763,#5768,#4488,.T.);
#7517=EDGE_CURVE('',#5758,#5731,#4489,.T.);
#7518=EDGE_CURVE('',#5732,#5757,#4490,.T.);
#7519=EDGE_CURVE('',#5756,#5729,#4491,.T.);
#7520=EDGE_CURVE('',#5730,#5755,#4492,.T.);
#7521=EDGE_CURVE('',#5745,#5742,#4493,.T.);
#7522=EDGE_CURVE('',#5744,#5743,#4494,.T.);
#7523=EDGE_CURVE('',#5740,#5737,#4495,.T.);
#7524=EDGE_CURVE('',#5741,#5746,#4496,.T.);
#7525=EDGE_CURVE('',#5736,#5709,#4497,.T.);
#7526=EDGE_CURVE('',#5710,#5735,#4498,.T.);
#7527=EDGE_CURVE('',#5734,#5707,#4499,.T.);
#7528=EDGE_CURVE('',#5708,#5733,#4500,.T.);
#7529=EDGE_CURVE('',#5723,#5720,#4501,.T.);
#7530=EDGE_CURVE('',#5722,#5721,#4502,.T.);
#7531=EDGE_CURVE('',#5718,#5715,#4503,.T.);
#7532=EDGE_CURVE('',#5719,#5724,#4504,.T.);
#7533=EDGE_CURVE('',#5714,#5687,#4505,.T.);
#7534=EDGE_CURVE('',#5688,#5713,#4506,.T.);
#7535=EDGE_CURVE('',#5712,#5685,#4507,.T.);
#7536=EDGE_CURVE('',#5686,#5711,#4508,.T.);
#7537=EDGE_CURVE('',#5701,#5698,#4509,.T.);
#7538=EDGE_CURVE('',#5700,#5699,#4510,.T.);
#7539=EDGE_CURVE('',#5696,#5693,#4511,.T.);
#7540=EDGE_CURVE('',#5697,#5702,#4512,.T.);
#7541=EDGE_CURVE('',#5692,#5665,#4513,.T.);
#7542=EDGE_CURVE('',#5666,#5691,#4514,.T.);
#7543=EDGE_CURVE('',#5690,#5663,#4515,.T.);
#7544=EDGE_CURVE('',#5664,#5689,#4516,.T.);
#7545=EDGE_CURVE('',#5679,#5676,#4517,.T.);
#7546=EDGE_CURVE('',#5678,#5677,#4518,.T.);
#7547=EDGE_CURVE('',#5674,#5671,#4519,.T.);
#7548=EDGE_CURVE('',#5675,#5680,#4520,.T.);
#7549=EDGE_CURVE('',#5670,#5809,#4521,.T.);
#7550=EDGE_CURVE('',#5810,#5669,#4522,.T.);
#7551=EDGE_CURVE('',#5668,#5807,#4523,.T.);
#7552=EDGE_CURVE('',#5808,#5667,#4524,.T.);
#7553=EDGE_CURVE('',#5783,#5789,#4525,.T.);
#7554=EDGE_CURVE('',#5788,#5784,#4526,.T.);
#7555=EDGE_CURVE('',#5781,#5790,#4527,.T.);
#7556=EDGE_CURVE('',#5787,#5785,#4528,.T.);
#7557=EDGE_CURVE('',#5815,#5815,#4529,.T.);
#7558=EDGE_CURVE('',#5815,#5816,#4530,.T.);
#7559=EDGE_CURVE('',#5816,#5816,#4531,.T.);
#7560=EDGE_CURVE('',#5817,#5818,#4532,.T.);
#7561=EDGE_CURVE('',#5818,#5819,#4533,.T.);
#7562=EDGE_CURVE('',#5819,#5820,#4534,.T.);
#7563=EDGE_CURVE('',#5820,#5819,#4535,.T.);
#7564=EDGE_CURVE('',#5818,#5817,#4536,.T.);
#7565=EDGE_CURVE('',#5821,#5822,#4537,.T.);
#7566=EDGE_CURVE('',#5822,#5823,#4538,.T.);
#7567=EDGE_CURVE('',#5823,#5823,#4539,.T.);
#7568=EDGE_CURVE('',#5822,#5821,#4540,.T.);
#7569=EDGE_CURVE('',#5817,#5824,#3395,.T.);
#7570=EDGE_CURVE('',#5824,#5824,#4541,.T.);
#7571=EDGE_CURVE('',#5820,#5821,#3396,.T.);
#7572=EDGE_CURVE('',#5823,#5825,#3397,.T.);
#7573=EDGE_CURVE('',#5825,#5825,#4542,.T.);
#7574=EDGE_CURVE('',#5826,#5826,#4543,.T.);
#7575=EDGE_CURVE('',#5826,#5816,#3398,.T.);
#7576=EDGE_CURVE('',#5815,#5827,#3399,.T.);
#7577=EDGE_CURVE('',#5827,#5827,#4544,.T.);
#7578=EDGE_CURVE('',#5828,#5829,#4545,.T.);
#7579=EDGE_CURVE('',#5830,#5831,#4546,.T.);
#7580=EDGE_CURVE('',#5832,#5833,#4547,.T.);
#7581=EDGE_CURVE('',#5834,#5835,#4548,.T.);
#7582=EDGE_CURVE('',#5836,#5837,#4549,.T.);
#7583=EDGE_CURVE('',#5838,#5839,#4550,.T.);
#7584=EDGE_CURVE('',#5840,#5841,#4551,.T.);
#7585=EDGE_CURVE('',#5842,#5842,#4552,.T.);
#7586=EDGE_CURVE('',#5842,#5843,#4553,.T.);
#7587=EDGE_CURVE('',#5843,#5844,#4554,.T.);
#7588=EDGE_CURVE('',#5844,#5843,#4555,.T.);
#7589=EDGE_CURVE('',#5845,#5845,#4556,.T.);
#7590=EDGE_CURVE('',#5845,#5846,#4557,.T.);
#7591=EDGE_CURVE('',#5846,#5846,#4558,.T.);
#7592=EDGE_CURVE('',#5847,#5847,#4559,.T.);
#7593=EDGE_CURVE('',#5847,#5848,#4560,.T.);
#7594=EDGE_CURVE('',#5848,#5848,#4561,.T.);
#7595=EDGE_CURVE('',#5849,#5850,#4562,.T.);
#7596=EDGE_CURVE('',#5850,#5851,#4563,.T.);
#7597=EDGE_CURVE('',#5851,#5851,#4564,.T.);
#7598=EDGE_CURVE('',#5850,#5849,#4565,.T.);
#7599=EDGE_CURVE('',#5852,#5852,#4566,.T.);
#7600=EDGE_CURVE('',#5852,#5853,#3400,.T.);
#7601=EDGE_CURVE('',#5853,#5853,#4567,.T.);
#7602=EDGE_CURVE('',#5844,#5854,#3401,.T.);
#7603=EDGE_CURVE('',#5854,#5854,#4568,.T.);
#7604=EDGE_CURVE('',#5855,#5855,#4569,.T.);
#7605=EDGE_CURVE('',#5855,#5849,#3402,.T.);
#7606=EDGE_CURVE('',#5855,#5856,#4570,.T.);
#7607=EDGE_CURVE('',#5856,#5856,#4571,.T.);
#7608=EDGE_CURVE('',#5845,#5856,#3403,.T.);
#7609=EDGE_CURVE('',#5857,#5857,#4572,.T.);
#7610=EDGE_CURVE('',#5857,#5848,#3404,.T.);
#7611=EDGE_CURVE('',#5858,#5858,#4573,.T.);
#7612=EDGE_CURVE('',#5858,#5859,#3405,.T.);
#7613=EDGE_CURVE('',#5859,#5859,#4574,.T.);
#7614=EDGE_CURVE('',#5860,#5860,#4575,.T.);
#7615=EDGE_CURVE('',#5860,#5861,#3406,.T.);
#7616=EDGE_CURVE('',#5861,#5861,#4576,.T.);
#7617=EDGE_CURVE('',#5862,#5863,#4577,.T.);
#7618=EDGE_CURVE('',#5863,#5862,#4578,.T.);
#7619=EDGE_CURVE('',#5863,#5864,#3407,.T.);
#7620=EDGE_CURVE('',#5864,#5864,#4579,.T.);
#7621=EDGE_CURVE('',#5860,#5862,#3408,.T.);
#7622=EDGE_CURVE('',#5865,#5865,#4580,.T.);
#7623=EDGE_CURVE('',#5865,#5866,#4581,.T.);
#7624=EDGE_CURVE('',#5866,#5866,#4582,.T.);
#7625=EDGE_CURVE('',#5867,#5868,#779,.T.);
#7626=EDGE_CURVE('',#5869,#5868,#780,.T.);
#7627=EDGE_CURVE('',#5870,#5869,#781,.T.);
#7628=EDGE_CURVE('',#5867,#5870,#782,.T.);
#7629=EDGE_CURVE('',#5871,#5872,#783,.T.);
#7630=EDGE_CURVE('',#5873,#5872,#784,.T.);
#7631=EDGE_CURVE('',#5874,#5873,#785,.T.);
#7632=EDGE_CURVE('',#5871,#5874,#786,.T.);
#7633=EDGE_CURVE('',#5875,#5876,#4583,.T.);
#7634=EDGE_CURVE('',#5877,#5875,#787,.T.);
#7635=EDGE_CURVE('',#5877,#5878,#4584,.T.);
#7636=EDGE_CURVE('',#5879,#5878,#788,.T.);
#7637=EDGE_CURVE('',#5876,#5879,#4585,.T.);
#7638=EDGE_CURVE('',#5876,#5880,#4586,.T.);
#7639=EDGE_CURVE('',#5881,#5880,#4587,.T.);
#7640=EDGE_CURVE('',#5882,#5881,#789,.T.);
#7641=EDGE_CURVE('',#5882,#5883,#4588,.T.);
#7642=EDGE_CURVE('',#5884,#5883,#790,.T.);
#7643=EDGE_CURVE('',#5880,#5884,#4589,.T.);
#7644=EDGE_CURVE('',#5885,#5885,#4590,.T.);
#7645=EDGE_CURVE('',#5886,#5886,#4591,.T.);
#7646=EDGE_CURVE('',#5887,#5887,#4592,.T.);
#7647=EDGE_CURVE('',#5887,#5888,#4593,.T.);
#7648=EDGE_CURVE('',#5888,#5888,#4594,.T.);
#7649=EDGE_CURVE('',#5889,#5890,#791,.T.);
#7650=EDGE_CURVE('',#5891,#5890,#792,.T.);
#7651=EDGE_CURVE('',#5892,#5891,#793,.T.);
#7652=EDGE_CURVE('',#5889,#5892,#794,.T.);
#7653=EDGE_CURVE('',#5893,#5894,#795,.T.);
#7654=EDGE_CURVE('',#5895,#5894,#796,.T.);
#7655=EDGE_CURVE('',#5896,#5895,#797,.T.);
#7656=EDGE_CURVE('',#5893,#5896,#798,.T.);
#7657=EDGE_CURVE('',#5897,#5898,#4595,.T.);
#7658=EDGE_CURVE('',#5899,#5897,#799,.T.);
#7659=EDGE_CURVE('',#5899,#5900,#4596,.T.);
#7660=EDGE_CURVE('',#5901,#5900,#800,.T.);
#7661=EDGE_CURVE('',#5898,#5901,#4597,.T.);
#7662=EDGE_CURVE('',#5898,#5902,#4598,.T.);
#7663=EDGE_CURVE('',#5903,#5902,#4599,.T.);
#7664=EDGE_CURVE('',#5904,#5903,#801,.T.);
#7665=EDGE_CURVE('',#5904,#5905,#4600,.T.);
#7666=EDGE_CURVE('',#5906,#5905,#802,.T.);
#7667=EDGE_CURVE('',#5902,#5906,#4601,.T.);
#7668=EDGE_CURVE('',#5907,#5907,#4602,.T.);
#7669=EDGE_CURVE('',#5908,#5908,#4603,.T.);
#7670=EDGE_CURVE('',#5909,#5909,#4604,.T.);
#7671=EDGE_CURVE('',#5909,#5910,#4605,.T.);
#7672=EDGE_CURVE('',#5910,#5910,#4606,.T.);
#7673=EDGE_CURVE('',#5911,#5912,#803,.T.);
#7674=EDGE_CURVE('',#5913,#5912,#804,.T.);
#7675=EDGE_CURVE('',#5914,#5913,#805,.T.);
#7676=EDGE_CURVE('',#5911,#5914,#806,.T.);
#7677=EDGE_CURVE('',#5915,#5916,#807,.T.);
#7678=EDGE_CURVE('',#5917,#5916,#808,.T.);
#7679=EDGE_CURVE('',#5918,#5917,#809,.T.);
#7680=EDGE_CURVE('',#5915,#5918,#810,.T.);
#7681=EDGE_CURVE('',#5919,#5920,#4607,.T.);
#7682=EDGE_CURVE('',#5921,#5919,#811,.T.);
#7683=EDGE_CURVE('',#5921,#5922,#4608,.T.);
#7684=EDGE_CURVE('',#5923,#5922,#812,.T.);
#7685=EDGE_CURVE('',#5920,#5923,#4609,.T.);
#7686=EDGE_CURVE('',#5920,#5924,#4610,.T.);
#7687=EDGE_CURVE('',#5925,#5924,#4611,.T.);
#7688=EDGE_CURVE('',#5926,#5925,#813,.T.);
#7689=EDGE_CURVE('',#5926,#5927,#4612,.T.);
#7690=EDGE_CURVE('',#5928,#5927,#814,.T.);
#7691=EDGE_CURVE('',#5924,#5928,#4613,.T.);
#7692=EDGE_CURVE('',#5929,#5929,#4614,.T.);
#7693=EDGE_CURVE('',#5930,#5930,#4615,.T.);
#7694=EDGE_CURVE('',#5931,#5931,#4616,.T.);
#7695=EDGE_CURVE('',#5931,#5932,#4617,.T.);
#7696=EDGE_CURVE('',#5932,#5932,#4618,.T.);
#7697=EDGE_CURVE('',#5933,#5934,#815,.T.);
#7698=EDGE_CURVE('',#5935,#5934,#816,.T.);
#7699=EDGE_CURVE('',#5936,#5935,#817,.T.);
#7700=EDGE_CURVE('',#5933,#5936,#818,.T.);
#7701=EDGE_CURVE('',#5937,#5938,#819,.T.);
#7702=EDGE_CURVE('',#5939,#5938,#820,.T.);
#7703=EDGE_CURVE('',#5940,#5939,#821,.T.);
#7704=EDGE_CURVE('',#5937,#5940,#822,.T.);
#7705=EDGE_CURVE('',#5941,#5942,#4619,.T.);
#7706=EDGE_CURVE('',#5943,#5941,#823,.T.);
#7707=EDGE_CURVE('',#5943,#5944,#4620,.T.);
#7708=EDGE_CURVE('',#5945,#5944,#824,.T.);
#7709=EDGE_CURVE('',#5942,#5945,#4621,.T.);
#7710=EDGE_CURVE('',#5942,#5946,#4622,.T.);
#7711=EDGE_CURVE('',#5947,#5946,#4623,.T.);
#7712=EDGE_CURVE('',#5948,#5947,#825,.T.);
#7713=EDGE_CURVE('',#5948,#5949,#4624,.T.);
#7714=EDGE_CURVE('',#5950,#5949,#826,.T.);
#7715=EDGE_CURVE('',#5946,#5950,#4625,.T.);
#7716=EDGE_CURVE('',#5951,#5951,#4626,.T.);
#7717=EDGE_CURVE('',#5952,#5952,#4627,.T.);
#7718=EDGE_CURVE('',#5953,#5953,#4628,.T.);
#7719=EDGE_CURVE('',#5953,#5954,#4629,.T.);
#7720=EDGE_CURVE('',#5954,#5954,#4630,.T.);
#7721=EDGE_CURVE('',#5955,#5956,#827,.T.);
#7722=EDGE_CURVE('',#5957,#5956,#828,.T.);
#7723=EDGE_CURVE('',#5958,#5957,#829,.T.);
#7724=EDGE_CURVE('',#5955,#5958,#830,.T.);
#7725=EDGE_CURVE('',#5959,#5960,#831,.T.);
#7726=EDGE_CURVE('',#5961,#5960,#832,.T.);
#7727=EDGE_CURVE('',#5962,#5961,#833,.T.);
#7728=EDGE_CURVE('',#5959,#5962,#834,.T.);
#7729=EDGE_CURVE('',#5963,#5964,#4631,.T.);
#7730=EDGE_CURVE('',#5965,#5963,#835,.T.);
#7731=EDGE_CURVE('',#5965,#5966,#4632,.T.);
#7732=EDGE_CURVE('',#5967,#5966,#836,.T.);
#7733=EDGE_CURVE('',#5964,#5967,#4633,.T.);
#7734=EDGE_CURVE('',#5964,#5968,#4634,.T.);
#7735=EDGE_CURVE('',#5969,#5968,#4635,.T.);
#7736=EDGE_CURVE('',#5970,#5969,#837,.T.);
#7737=EDGE_CURVE('',#5970,#5971,#4636,.T.);
#7738=EDGE_CURVE('',#5972,#5971,#838,.T.);
#7739=EDGE_CURVE('',#5968,#5972,#4637,.T.);
#7740=EDGE_CURVE('',#5973,#5973,#4638,.T.);
#7741=EDGE_CURVE('',#5974,#5974,#4639,.T.);
#7742=EDGE_CURVE('',#5975,#5975,#4640,.T.);
#7743=EDGE_CURVE('',#5975,#5976,#4641,.T.);
#7744=EDGE_CURVE('',#5976,#5976,#4642,.T.);
#7745=EDGE_CURVE('',#5977,#5978,#839,.T.);
#7746=EDGE_CURVE('',#5978,#5979,#840,.T.);
#7747=EDGE_CURVE('',#5979,#5980,#841,.T.);
#7748=EDGE_CURVE('',#5977,#5980,#842,.T.);
#7749=EDGE_CURVE('',#5981,#5982,#843,.T.);
#7750=EDGE_CURVE('',#5983,#5982,#844,.T.);
#7751=EDGE_CURVE('',#5984,#5983,#845,.T.);
#7752=EDGE_CURVE('',#5981,#5984,#846,.T.);
#7753=EDGE_CURVE('',#5985,#5986,#4643,.T.);
#7754=EDGE_CURVE('',#5986,#5987,#4644,.T.);
#7755=EDGE_CURVE('',#5988,#5987,#4645,.T.);
#7756=EDGE_CURVE('',#5989,#5988,#847,.T.);
#7757=EDGE_CURVE('',#5989,#5990,#4646,.T.);
#7758=EDGE_CURVE('',#5991,#5990,#848,.T.);
#7759=EDGE_CURVE('',#5987,#5991,#4647,.T.);
#7760=EDGE_CURVE('',#5986,#5992,#4648,.T.);
#7761=EDGE_CURVE('',#5992,#5993,#849,.T.);
#7762=EDGE_CURVE('',#5994,#5993,#4649,.T.);
#7763=EDGE_CURVE('',#5994,#5985,#850,.T.);
#7764=EDGE_CURVE('',#5995,#5995,#4650,.T.);
#7765=EDGE_CURVE('',#5996,#5996,#4651,.T.);
#7766=EDGE_CURVE('',#5997,#5998,#4652,.T.);
#7767=EDGE_CURVE('',#5999,#5997,#851,.T.);
#7768=EDGE_CURVE('',#5999,#6000,#4653,.T.);
#7769=EDGE_CURVE('',#6001,#6000,#852,.T.);
#7770=EDGE_CURVE('',#5998,#6001,#4654,.T.);
#7771=EDGE_CURVE('',#5998,#6002,#4655,.T.);
#7772=EDGE_CURVE('',#6003,#6002,#4656,.T.);
#7773=EDGE_CURVE('',#6004,#6003,#853,.T.);
#7774=EDGE_CURVE('',#6004,#6005,#4657,.T.);
#7775=EDGE_CURVE('',#6006,#6005,#854,.T.);
#7776=EDGE_CURVE('',#6002,#6006,#4658,.T.);
#7777=EDGE_CURVE('',#6007,#6007,#4659,.T.);
#7778=EDGE_CURVE('',#6008,#6008,#4660,.T.);
#7779=EDGE_CURVE('',#6009,#6009,#4661,.T.);
#7780=EDGE_CURVE('',#6009,#6010,#4662,.T.);
#7781=EDGE_CURVE('',#6010,#6010,#4663,.T.);
#7782=EDGE_CURVE('',#6011,#6012,#855,.T.);
#7783=EDGE_CURVE('',#6013,#6012,#856,.T.);
#7784=EDGE_CURVE('',#6014,#6013,#857,.T.);
#7785=EDGE_CURVE('',#6011,#6014,#858,.T.);
#7786=EDGE_CURVE('',#6015,#6016,#859,.T.);
#7787=EDGE_CURVE('',#6017,#6016,#860,.T.);
#7788=EDGE_CURVE('',#6018,#6017,#861,.T.);
#7789=EDGE_CURVE('',#6015,#6018,#862,.T.);
#7790=EDGE_CURVE('',#6017,#5979,#4664,.T.);
#7791=EDGE_CURVE('',#6016,#5980,#4665,.T.);
#7792=EDGE_CURVE('',#5977,#6015,#4666,.T.);
#7793=EDGE_CURVE('',#5978,#6018,#4667,.T.);
#7794=EDGE_CURVE('',#6000,#6004,#4668,.T.);
#7795=EDGE_CURVE('',#6005,#5999,#4669,.T.);
#7796=EDGE_CURVE('',#6006,#5997,#4670,.T.);
#7797=EDGE_CURVE('',#6001,#6003,#4671,.T.);
#7798=EDGE_CURVE('',#5957,#5984,#4672,.T.);
#7799=EDGE_CURVE('',#5983,#5958,#4673,.T.);
#7800=EDGE_CURVE('',#5982,#5955,#4674,.T.);
#7801=EDGE_CURVE('',#5956,#5981,#4675,.T.);
#7802=EDGE_CURVE('',#5967,#5969,#4676,.T.);
#7803=EDGE_CURVE('',#5966,#5970,#4677,.T.);
#7804=EDGE_CURVE('',#5971,#5965,#4678,.T.);
#7805=EDGE_CURVE('',#5972,#5963,#4679,.T.);
#7806=EDGE_CURVE('',#5935,#5962,#4680,.T.);
#7807=EDGE_CURVE('',#5961,#5936,#4681,.T.);
#7808=EDGE_CURVE('',#5960,#5933,#4682,.T.);
#7809=EDGE_CURVE('',#5934,#5959,#4683,.T.);
#7810=EDGE_CURVE('',#5945,#5947,#4684,.T.);
#7811=EDGE_CURVE('',#5944,#5948,#4685,.T.);
#7812=EDGE_CURVE('',#5949,#5943,#4686,.T.);
#7813=EDGE_CURVE('',#5950,#5941,#4687,.T.);
#7814=EDGE_CURVE('',#5913,#5940,#4688,.T.);
#7815=EDGE_CURVE('',#5939,#5914,#4689,.T.);
#7816=EDGE_CURVE('',#5938,#5911,#4690,.T.);
#7817=EDGE_CURVE('',#5912,#5937,#4691,.T.);
#7818=EDGE_CURVE('',#5923,#5925,#4692,.T.);
#7819=EDGE_CURVE('',#5922,#5926,#4693,.T.);
#7820=EDGE_CURVE('',#5927,#5921,#4694,.T.);
#7821=EDGE_CURVE('',#5928,#5919,#4695,.T.);
#7822=EDGE_CURVE('',#5891,#5918,#4696,.T.);
#7823=EDGE_CURVE('',#5917,#5892,#4697,.T.);
#7824=EDGE_CURVE('',#5916,#5889,#4698,.T.);
#7825=EDGE_CURVE('',#5890,#5915,#4699,.T.);
#7826=EDGE_CURVE('',#5901,#5903,#4700,.T.);
#7827=EDGE_CURVE('',#5900,#5904,#4701,.T.);
#7828=EDGE_CURVE('',#5905,#5899,#4702,.T.);
#7829=EDGE_CURVE('',#5906,#5897,#4703,.T.);
#7830=EDGE_CURVE('',#5869,#5896,#4704,.T.);
#7831=EDGE_CURVE('',#5895,#5870,#4705,.T.);
#7832=EDGE_CURVE('',#5894,#5867,#4706,.T.);
#7833=EDGE_CURVE('',#5868,#5893,#4707,.T.);
#7834=EDGE_CURVE('',#5879,#5881,#4708,.T.);
#7835=EDGE_CURVE('',#5878,#5882,#4709,.T.);
#7836=EDGE_CURVE('',#5883,#5877,#4710,.T.);
#7837=EDGE_CURVE('',#5884,#5875,#4711,.T.);
#7838=EDGE_CURVE('',#6013,#5874,#4712,.T.);
#7839=EDGE_CURVE('',#5873,#6014,#4713,.T.);
#7840=EDGE_CURVE('',#5872,#6011,#4714,.T.);
#7841=EDGE_CURVE('',#6012,#5871,#4715,.T.);
#7842=EDGE_CURVE('',#5990,#5993,#4716,.T.);
#7843=EDGE_CURVE('',#5994,#5989,#4717,.T.);
#7844=EDGE_CURVE('',#5985,#5988,#4718,.T.);
#7845=EDGE_CURVE('',#5991,#5992,#4719,.T.);
#7846=EDGE_CURVE('',#6019,#6019,#4720,.T.);
#7847=EDGE_CURVE('',#6019,#6020,#4721,.T.);
#7848=EDGE_CURVE('',#6020,#6020,#4722,.T.);
#7849=EDGE_CURVE('',#6021,#6022,#4723,.T.);
#7850=EDGE_CURVE('',#6022,#6023,#4724,.T.);
#7851=EDGE_CURVE('',#6023,#6024,#4725,.T.);
#7852=EDGE_CURVE('',#6024,#6023,#4726,.T.);
#7853=EDGE_CURVE('',#6022,#6021,#4727,.T.);
#7854=EDGE_CURVE('',#6025,#6026,#4728,.T.);
#7855=EDGE_CURVE('',#6026,#6027,#4729,.T.);
#7856=EDGE_CURVE('',#6027,#6027,#4730,.T.);
#7857=EDGE_CURVE('',#6026,#6025,#4731,.T.);
#7858=EDGE_CURVE('',#6021,#6028,#3409,.T.);
#7859=EDGE_CURVE('',#6028,#6028,#4732,.T.);
#7860=EDGE_CURVE('',#6024,#6025,#3410,.T.);
#7861=EDGE_CURVE('',#6027,#6029,#3411,.T.);
#7862=EDGE_CURVE('',#6029,#6029,#4733,.T.);
#7863=EDGE_CURVE('',#6030,#6030,#4734,.T.);
#7864=EDGE_CURVE('',#6030,#6020,#3412,.T.);
#7865=EDGE_CURVE('',#6019,#6031,#3413,.T.);
#7866=EDGE_CURVE('',#6031,#6031,#4735,.T.);
#7867=EDGE_CURVE('',#6032,#6033,#4736,.T.);
#7868=EDGE_CURVE('',#6034,#6035,#4737,.T.);
#7869=EDGE_CURVE('',#6036,#6037,#4738,.T.);
#7870=EDGE_CURVE('',#6038,#6039,#4739,.T.);
#7871=EDGE_CURVE('',#6040,#6041,#4740,.T.);
#7872=EDGE_CURVE('',#6042,#6043,#4741,.T.);
#7873=EDGE_CURVE('',#6044,#6045,#4742,.T.);
#7874=EDGE_CURVE('',#6046,#6046,#4743,.T.);
#7875=EDGE_CURVE('',#6046,#6047,#4744,.T.);
#7876=EDGE_CURVE('',#6047,#6048,#4745,.T.);
#7877=EDGE_CURVE('',#6048,#6047,#4746,.T.);
#7878=EDGE_CURVE('',#6049,#6049,#4747,.T.);
#7879=EDGE_CURVE('',#6049,#6050,#4748,.T.);
#7880=EDGE_CURVE('',#6050,#6050,#4749,.T.);
#7881=EDGE_CURVE('',#6051,#6051,#4750,.T.);
#7882=EDGE_CURVE('',#6051,#6052,#4751,.T.);
#7883=EDGE_CURVE('',#6052,#6052,#4752,.T.);
#7884=EDGE_CURVE('',#6053,#6054,#4753,.T.);
#7885=EDGE_CURVE('',#6054,#6055,#4754,.T.);
#7886=EDGE_CURVE('',#6055,#6055,#4755,.T.);
#7887=EDGE_CURVE('',#6054,#6053,#4756,.T.);
#7888=EDGE_CURVE('',#6056,#6056,#4757,.T.);
#7889=EDGE_CURVE('',#6056,#6057,#3414,.T.);
#7890=EDGE_CURVE('',#6057,#6057,#4758,.T.);
#7891=EDGE_CURVE('',#6048,#6058,#3415,.T.);
#7892=EDGE_CURVE('',#6058,#6058,#4759,.T.);
#7893=EDGE_CURVE('',#6059,#6059,#4760,.T.);
#7894=EDGE_CURVE('',#6059,#6053,#3416,.T.);
#7895=EDGE_CURVE('',#6059,#6060,#4761,.T.);
#7896=EDGE_CURVE('',#6060,#6060,#4762,.T.);
#7897=EDGE_CURVE('',#6049,#6060,#3417,.T.);
#7898=EDGE_CURVE('',#6061,#6061,#4763,.T.);
#7899=EDGE_CURVE('',#6061,#6052,#3418,.T.);
#7900=EDGE_CURVE('',#6062,#6062,#4764,.T.);
#7901=EDGE_CURVE('',#6062,#6063,#3419,.T.);
#7902=EDGE_CURVE('',#6063,#6063,#4765,.T.);
#7903=EDGE_CURVE('',#6064,#6064,#4766,.T.);
#7904=EDGE_CURVE('',#6064,#6065,#3420,.T.);
#7905=EDGE_CURVE('',#6065,#6065,#4767,.T.);
#7906=EDGE_CURVE('',#6066,#6067,#4768,.T.);
#7907=EDGE_CURVE('',#6067,#6066,#4769,.T.);
#7908=EDGE_CURVE('',#6067,#6068,#3421,.T.);
#7909=EDGE_CURVE('',#6068,#6068,#4770,.T.);
#7910=EDGE_CURVE('',#6064,#6066,#3422,.T.);
#7911=EDGE_CURVE('',#6069,#6069,#4771,.T.);
#7912=EDGE_CURVE('',#6069,#6070,#4772,.T.);
#7913=EDGE_CURVE('',#6070,#6070,#4773,.T.);
#7914=EDGE_CURVE('',#6071,#6072,#863,.T.);
#7915=EDGE_CURVE('',#6073,#6072,#864,.T.);
#7916=EDGE_CURVE('',#6074,#6073,#865,.T.);
#7917=EDGE_CURVE('',#6071,#6074,#866,.T.);
#7918=EDGE_CURVE('',#6075,#6076,#867,.T.);
#7919=EDGE_CURVE('',#6077,#6076,#868,.T.);
#7920=EDGE_CURVE('',#6078,#6077,#869,.T.);
#7921=EDGE_CURVE('',#6075,#6078,#870,.T.);
#7922=EDGE_CURVE('',#6079,#6080,#4774,.T.);
#7923=EDGE_CURVE('',#6081,#6079,#871,.T.);
#7924=EDGE_CURVE('',#6081,#6082,#4775,.T.);
#7925=EDGE_CURVE('',#6083,#6082,#872,.T.);
#7926=EDGE_CURVE('',#6080,#6083,#4776,.T.);
#7927=EDGE_CURVE('',#6080,#6084,#4777,.T.);
#7928=EDGE_CURVE('',#6085,#6084,#4778,.T.);
#7929=EDGE_CURVE('',#6086,#6085,#873,.T.);
#7930=EDGE_CURVE('',#6086,#6087,#4779,.T.);
#7931=EDGE_CURVE('',#6088,#6087,#874,.T.);
#7932=EDGE_CURVE('',#6084,#6088,#4780,.T.);
#7933=EDGE_CURVE('',#6089,#6089,#4781,.T.);
#7934=EDGE_CURVE('',#6090,#6090,#4782,.T.);
#7935=EDGE_CURVE('',#6091,#6091,#4783,.T.);
#7936=EDGE_CURVE('',#6091,#6092,#4784,.T.);
#7937=EDGE_CURVE('',#6092,#6092,#4785,.T.);
#7938=EDGE_CURVE('',#6093,#6094,#875,.T.);
#7939=EDGE_CURVE('',#6095,#6094,#876,.T.);
#7940=EDGE_CURVE('',#6096,#6095,#877,.T.);
#7941=EDGE_CURVE('',#6093,#6096,#878,.T.);
#7942=EDGE_CURVE('',#6097,#6098,#879,.T.);
#7943=EDGE_CURVE('',#6099,#6098,#880,.T.);
#7944=EDGE_CURVE('',#6100,#6099,#881,.T.);
#7945=EDGE_CURVE('',#6097,#6100,#882,.T.);
#7946=EDGE_CURVE('',#6101,#6102,#4786,.T.);
#7947=EDGE_CURVE('',#6103,#6101,#883,.T.);
#7948=EDGE_CURVE('',#6103,#6104,#4787,.T.);
#7949=EDGE_CURVE('',#6105,#6104,#884,.T.);
#7950=EDGE_CURVE('',#6102,#6105,#4788,.T.);
#7951=EDGE_CURVE('',#6102,#6106,#4789,.T.);
#7952=EDGE_CURVE('',#6107,#6106,#4790,.T.);
#7953=EDGE_CURVE('',#6108,#6107,#885,.T.);
#7954=EDGE_CURVE('',#6108,#6109,#4791,.T.);
#7955=EDGE_CURVE('',#6110,#6109,#886,.T.);
#7956=EDGE_CURVE('',#6106,#6110,#4792,.T.);
#7957=EDGE_CURVE('',#6111,#6111,#4793,.T.);
#7958=EDGE_CURVE('',#6112,#6112,#4794,.T.);
#7959=EDGE_CURVE('',#6113,#6113,#4795,.T.);
#7960=EDGE_CURVE('',#6113,#6114,#4796,.T.);
#7961=EDGE_CURVE('',#6114,#6114,#4797,.T.);
#7962=EDGE_CURVE('',#6115,#6116,#887,.T.);
#7963=EDGE_CURVE('',#6117,#6116,#888,.T.);
#7964=EDGE_CURVE('',#6118,#6117,#889,.T.);
#7965=EDGE_CURVE('',#6115,#6118,#890,.T.);
#7966=EDGE_CURVE('',#6119,#6120,#891,.T.);
#7967=EDGE_CURVE('',#6121,#6120,#892,.T.);
#7968=EDGE_CURVE('',#6122,#6121,#893,.T.);
#7969=EDGE_CURVE('',#6119,#6122,#894,.T.);
#7970=EDGE_CURVE('',#6123,#6124,#4798,.T.);
#7971=EDGE_CURVE('',#6125,#6123,#895,.T.);
#7972=EDGE_CURVE('',#6125,#6126,#4799,.T.);
#7973=EDGE_CURVE('',#6127,#6126,#896,.T.);
#7974=EDGE_CURVE('',#6124,#6127,#4800,.T.);
#7975=EDGE_CURVE('',#6124,#6128,#4801,.T.);
#7976=EDGE_CURVE('',#6129,#6128,#4802,.T.);
#7977=EDGE_CURVE('',#6130,#6129,#897,.T.);
#7978=EDGE_CURVE('',#6130,#6131,#4803,.T.);
#7979=EDGE_CURVE('',#6132,#6131,#898,.T.);
#7980=EDGE_CURVE('',#6128,#6132,#4804,.T.);
#7981=EDGE_CURVE('',#6133,#6133,#4805,.T.);
#7982=EDGE_CURVE('',#6134,#6134,#4806,.T.);
#7983=EDGE_CURVE('',#6135,#6135,#4807,.T.);
#7984=EDGE_CURVE('',#6135,#6136,#4808,.T.);
#7985=EDGE_CURVE('',#6136,#6136,#4809,.T.);
#7986=EDGE_CURVE('',#6137,#6138,#899,.T.);
#7987=EDGE_CURVE('',#6139,#6138,#900,.T.);
#7988=EDGE_CURVE('',#6140,#6139,#901,.T.);
#7989=EDGE_CURVE('',#6137,#6140,#902,.T.);
#7990=EDGE_CURVE('',#6141,#6142,#903,.T.);
#7991=EDGE_CURVE('',#6143,#6142,#904,.T.);
#7992=EDGE_CURVE('',#6144,#6143,#905,.T.);
#7993=EDGE_CURVE('',#6141,#6144,#906,.T.);
#7994=EDGE_CURVE('',#6145,#6146,#4810,.T.);
#7995=EDGE_CURVE('',#6147,#6145,#907,.T.);
#7996=EDGE_CURVE('',#6147,#6148,#4811,.T.);
#7997=EDGE_CURVE('',#6149,#6148,#908,.T.);
#7998=EDGE_CURVE('',#6146,#6149,#4812,.T.);
#7999=EDGE_CURVE('',#6146,#6150,#4813,.T.);
#8000=EDGE_CURVE('',#6151,#6150,#4814,.T.);
#8001=EDGE_CURVE('',#6152,#6151,#909,.T.);
#8002=EDGE_CURVE('',#6152,#6153,#4815,.T.);
#8003=EDGE_CURVE('',#6154,#6153,#910,.T.);
#8004=EDGE_CURVE('',#6150,#6154,#4816,.T.);
#8005=EDGE_CURVE('',#6155,#6155,#4817,.T.);
#8006=EDGE_CURVE('',#6156,#6156,#4818,.T.);
#8007=EDGE_CURVE('',#6157,#6157,#4819,.T.);
#8008=EDGE_CURVE('',#6157,#6158,#4820,.T.);
#8009=EDGE_CURVE('',#6158,#6158,#4821,.T.);
#8010=EDGE_CURVE('',#6159,#6160,#911,.T.);
#8011=EDGE_CURVE('',#6161,#6160,#912,.T.);
#8012=EDGE_CURVE('',#6162,#6161,#913,.T.);
#8013=EDGE_CURVE('',#6159,#6162,#914,.T.);
#8014=EDGE_CURVE('',#6163,#6164,#915,.T.);
#8015=EDGE_CURVE('',#6165,#6164,#916,.T.);
#8016=EDGE_CURVE('',#6166,#6165,#917,.T.);
#8017=EDGE_CURVE('',#6163,#6166,#918,.T.);
#8018=EDGE_CURVE('',#6167,#6168,#4822,.T.);
#8019=EDGE_CURVE('',#6169,#6167,#919,.T.);
#8020=EDGE_CURVE('',#6169,#6170,#4823,.T.);
#8021=EDGE_CURVE('',#6171,#6170,#920,.T.);
#8022=EDGE_CURVE('',#6168,#6171,#4824,.T.);
#8023=EDGE_CURVE('',#6168,#6172,#4825,.T.);
#8024=EDGE_CURVE('',#6173,#6172,#4826,.T.);
#8025=EDGE_CURVE('',#6174,#6173,#921,.T.);
#8026=EDGE_CURVE('',#6174,#6175,#4827,.T.);
#8027=EDGE_CURVE('',#6176,#6175,#922,.T.);
#8028=EDGE_CURVE('',#6172,#6176,#4828,.T.);
#8029=EDGE_CURVE('',#6177,#6177,#4829,.T.);
#8030=EDGE_CURVE('',#6178,#6178,#4830,.T.);
#8031=EDGE_CURVE('',#6179,#6179,#4831,.T.);
#8032=EDGE_CURVE('',#6179,#6180,#4832,.T.);
#8033=EDGE_CURVE('',#6180,#6180,#4833,.T.);
#8034=EDGE_CURVE('',#6181,#6182,#923,.T.);
#8035=EDGE_CURVE('',#6182,#6183,#924,.T.);
#8036=EDGE_CURVE('',#6183,#6184,#925,.T.);
#8037=EDGE_CURVE('',#6181,#6184,#926,.T.);
#8038=EDGE_CURVE('',#6185,#6186,#927,.T.);
#8039=EDGE_CURVE('',#6187,#6186,#928,.T.);
#8040=EDGE_CURVE('',#6188,#6187,#929,.T.);
#8041=EDGE_CURVE('',#6185,#6188,#930,.T.);
#8042=EDGE_CURVE('',#6189,#6190,#4834,.T.);
#8043=EDGE_CURVE('',#6190,#6191,#4835,.T.);
#8044=EDGE_CURVE('',#6192,#6191,#4836,.T.);
#8045=EDGE_CURVE('',#6193,#6192,#931,.T.);
#8046=EDGE_CURVE('',#6193,#6194,#4837,.T.);
#8047=EDGE_CURVE('',#6195,#6194,#932,.T.);
#8048=EDGE_CURVE('',#6191,#6195,#4838,.T.);
#8049=EDGE_CURVE('',#6190,#6196,#4839,.T.);
#8050=EDGE_CURVE('',#6196,#6197,#933,.T.);
#8051=EDGE_CURVE('',#6198,#6197,#4840,.T.);
#8052=EDGE_CURVE('',#6198,#6189,#934,.T.);
#8053=EDGE_CURVE('',#6199,#6199,#4841,.T.);
#8054=EDGE_CURVE('',#6200,#6200,#4842,.T.);
#8055=EDGE_CURVE('',#6201,#6202,#4843,.T.);
#8056=EDGE_CURVE('',#6203,#6201,#935,.T.);
#8057=EDGE_CURVE('',#6203,#6204,#4844,.T.);
#8058=EDGE_CURVE('',#6205,#6204,#936,.T.);
#8059=EDGE_CURVE('',#6202,#6205,#4845,.T.);
#8060=EDGE_CURVE('',#6202,#6206,#4846,.T.);
#8061=EDGE_CURVE('',#6207,#6206,#4847,.T.);
#8062=EDGE_CURVE('',#6208,#6207,#937,.T.);
#8063=EDGE_CURVE('',#6208,#6209,#4848,.T.);
#8064=EDGE_CURVE('',#6210,#6209,#938,.T.);
#8065=EDGE_CURVE('',#6206,#6210,#4849,.T.);
#8066=EDGE_CURVE('',#6211,#6211,#4850,.T.);
#8067=EDGE_CURVE('',#6212,#6212,#4851,.T.);
#8068=EDGE_CURVE('',#6213,#6213,#4852,.T.);
#8069=EDGE_CURVE('',#6213,#6214,#4853,.T.);
#8070=EDGE_CURVE('',#6214,#6214,#4854,.T.);
#8071=EDGE_CURVE('',#6215,#6216,#939,.T.);
#8072=EDGE_CURVE('',#6217,#6216,#940,.T.);
#8073=EDGE_CURVE('',#6218,#6217,#941,.T.);
#8074=EDGE_CURVE('',#6215,#6218,#942,.T.);
#8075=EDGE_CURVE('',#6219,#6220,#943,.T.);
#8076=EDGE_CURVE('',#6221,#6220,#944,.T.);
#8077=EDGE_CURVE('',#6222,#6221,#945,.T.);
#8078=EDGE_CURVE('',#6219,#6222,#946,.T.);
#8079=EDGE_CURVE('',#6221,#6183,#4855,.T.);
#8080=EDGE_CURVE('',#6220,#6184,#4856,.T.);
#8081=EDGE_CURVE('',#6181,#6219,#4857,.T.);
#8082=EDGE_CURVE('',#6182,#6222,#4858,.T.);
#8083=EDGE_CURVE('',#6204,#6208,#4859,.T.);
#8084=EDGE_CURVE('',#6209,#6203,#4860,.T.);
#8085=EDGE_CURVE('',#6210,#6201,#4861,.T.);
#8086=EDGE_CURVE('',#6205,#6207,#4862,.T.);
#8087=EDGE_CURVE('',#6161,#6188,#4863,.T.);
#8088=EDGE_CURVE('',#6187,#6162,#4864,.T.);
#8089=EDGE_CURVE('',#6186,#6159,#4865,.T.);
#8090=EDGE_CURVE('',#6160,#6185,#4866,.T.);
#8091=EDGE_CURVE('',#6171,#6173,#4867,.T.);
#8092=EDGE_CURVE('',#6170,#6174,#4868,.T.);
#8093=EDGE_CURVE('',#6175,#6169,#4869,.T.);
#8094=EDGE_CURVE('',#6176,#6167,#4870,.T.);
#8095=EDGE_CURVE('',#6139,#6166,#4871,.T.);
#8096=EDGE_CURVE('',#6165,#6140,#4872,.T.);
#8097=EDGE_CURVE('',#6164,#6137,#4873,.T.);
#8098=EDGE_CURVE('',#6138,#6163,#4874,.T.);
#8099=EDGE_CURVE('',#6149,#6151,#4875,.T.);
#8100=EDGE_CURVE('',#6148,#6152,#4876,.T.);
#8101=EDGE_CURVE('',#6153,#6147,#4877,.T.);
#8102=EDGE_CURVE('',#6154,#6145,#4878,.T.);
#8103=EDGE_CURVE('',#6117,#6144,#4879,.T.);
#8104=EDGE_CURVE('',#6143,#6118,#4880,.T.);
#8105=EDGE_CURVE('',#6142,#6115,#4881,.T.);
#8106=EDGE_CURVE('',#6116,#6141,#4882,.T.);
#8107=EDGE_CURVE('',#6127,#6129,#4883,.T.);
#8108=EDGE_CURVE('',#6126,#6130,#4884,.T.);
#8109=EDGE_CURVE('',#6131,#6125,#4885,.T.);
#8110=EDGE_CURVE('',#6132,#6123,#4886,.T.);
#8111=EDGE_CURVE('',#6095,#6122,#4887,.T.);
#8112=EDGE_CURVE('',#6121,#6096,#4888,.T.);
#8113=EDGE_CURVE('',#6120,#6093,#4889,.T.);
#8114=EDGE_CURVE('',#6094,#6119,#4890,.T.);
#8115=EDGE_CURVE('',#6105,#6107,#4891,.T.);
#8116=EDGE_CURVE('',#6104,#6108,#4892,.T.);
#8117=EDGE_CURVE('',#6109,#6103,#4893,.T.);
#8118=EDGE_CURVE('',#6110,#6101,#4894,.T.);
#8119=EDGE_CURVE('',#6073,#6100,#4895,.T.);
#8120=EDGE_CURVE('',#6099,#6074,#4896,.T.);
#8121=EDGE_CURVE('',#6098,#6071,#4897,.T.);
#8122=EDGE_CURVE('',#6072,#6097,#4898,.T.);
#8123=EDGE_CURVE('',#6083,#6085,#4899,.T.);
#8124=EDGE_CURVE('',#6082,#6086,#4900,.T.);
#8125=EDGE_CURVE('',#6087,#6081,#4901,.T.);
#8126=EDGE_CURVE('',#6088,#6079,#4902,.T.);
#8127=EDGE_CURVE('',#6217,#6078,#4903,.T.);
#8128=EDGE_CURVE('',#6077,#6218,#4904,.T.);
#8129=EDGE_CURVE('',#6076,#6215,#4905,.T.);
#8130=EDGE_CURVE('',#6216,#6075,#4906,.T.);
#8131=EDGE_CURVE('',#6194,#6197,#4907,.T.);
#8132=EDGE_CURVE('',#6198,#6193,#4908,.T.);
#8133=EDGE_CURVE('',#6189,#6192,#4909,.T.);
#8134=EDGE_CURVE('',#6195,#6196,#4910,.T.);
#8135=EDGE_CURVE('',#6223,#6223,#4911,.T.);
#8136=EDGE_CURVE('',#6223,#6224,#3423,.T.);
#8137=EDGE_CURVE('',#6224,#6224,#4912,.T.);
#8138=EDGE_CURVE('',#6225,#6226,#3424,.T.);
#8139=EDGE_CURVE('',#6227,#6225,#3425,.T.);
#8140=EDGE_CURVE('',#6228,#6227,#3426,.T.);
#8141=EDGE_CURVE('',#6226,#6228,#3427,.T.);
#8142=EDGE_CURVE('',#6229,#6229,#4913,.T.);
#8143=EDGE_CURVE('',#6229,#6230,#3428,.T.);
#8144=EDGE_CURVE('',#6230,#6230,#4914,.T.);
#8145=EDGE_CURVE('',#6231,#6232,#3429,.T.);
#8146=EDGE_CURVE('',#6232,#6233,#3430,.T.);
#8147=EDGE_CURVE('',#6233,#6234,#3431,.T.);
#8148=EDGE_CURVE('',#6234,#6231,#3432,.T.);
#8149=EDGE_CURVE('',#6234,#6227,#3433,.T.);
#8150=EDGE_CURVE('',#6231,#6225,#3434,.T.);
#8151=EDGE_CURVE('',#6232,#6226,#3435,.T.);
#8152=EDGE_CURVE('',#6233,#6228,#3436,.T.);
#8153=EDGE_CURVE('',#6235,#6235,#4915,.T.);
#8154=EDGE_CURVE('',#6235,#6236,#3437,.T.);
#8155=EDGE_CURVE('',#6236,#6236,#4916,.T.);
#8156=EDGE_CURVE('',#6237,#6237,#4917,.T.);
#8157=EDGE_CURVE('',#6237,#6238,#3438,.T.);
#8158=EDGE_CURVE('',#6238,#6238,#4918,.T.);
#8159=EDGE_CURVE('',#6239,#6240,#3439,.T.);
#8160=EDGE_CURVE('',#6241,#6239,#3440,.T.);
#8161=EDGE_CURVE('',#6242,#6241,#3441,.T.);
#8162=EDGE_CURVE('',#6240,#6242,#3442,.T.);
#8163=EDGE_CURVE('',#6239,#6243,#3443,.T.);
#8164=EDGE_CURVE('',#6244,#6243,#3444,.T.);
#8165=EDGE_CURVE('',#6241,#6244,#3445,.T.);
#8166=EDGE_CURVE('',#6240,#6245,#3446,.T.);
#8167=EDGE_CURVE('',#6243,#6245,#3447,.T.);
#8168=EDGE_CURVE('',#6246,#6244,#3448,.T.);
#8169=EDGE_CURVE('',#6242,#6246,#3449,.T.);
#8170=EDGE_CURVE('',#6245,#6246,#3450,.T.);
#8171=ORIENTED_EDGE('',*,*,#6247,.F.);
#8172=ORIENTED_EDGE('',*,*,#6248,.T.);
#8173=ORIENTED_EDGE('',*,*,#6249,.F.);
#8174=ORIENTED_EDGE('',*,*,#6248,.F.);
#8175=ORIENTED_EDGE('',*,*,#6250,.F.);
#8176=ORIENTED_EDGE('',*,*,#6251,.T.);
#8177=ORIENTED_EDGE('',*,*,#6252,.F.);
#8178=ORIENTED_EDGE('',*,*,#6251,.F.);
#8179=ORIENTED_EDGE('',*,*,#6249,.T.);
#8180=ORIENTED_EDGE('',*,*,#6250,.T.);
#8181=ORIENTED_EDGE('',*,*,#6253,.T.);
#8182=ORIENTED_EDGE('',*,*,#6254,.T.);
#8183=ORIENTED_EDGE('',*,*,#6255,.T.);
#8184=ORIENTED_EDGE('',*,*,#6256,.T.);
#8185=ORIENTED_EDGE('',*,*,#6254,.F.);
#8186=ORIENTED_EDGE('',*,*,#6257,.F.);
#8187=ORIENTED_EDGE('',*,*,#6258,.F.);
#8188=ORIENTED_EDGE('',*,*,#6259,.F.);
#8189=ORIENTED_EDGE('',*,*,#6260,.T.);
#8190=ORIENTED_EDGE('',*,*,#6261,.T.);
#8191=ORIENTED_EDGE('',*,*,#6262,.T.);
#8192=ORIENTED_EDGE('',*,*,#6263,.T.);
#8193=ORIENTED_EDGE('',*,*,#6261,.F.);
#8194=ORIENTED_EDGE('',*,*,#6264,.T.);
#8195=ORIENTED_EDGE('',*,*,#6265,.T.);
#8196=ORIENTED_EDGE('',*,*,#6266,.F.);
#8197=ORIENTED_EDGE('',*,*,#6267,.T.);
#8198=ORIENTED_EDGE('',*,*,#6268,.T.);
#8199=ORIENTED_EDGE('',*,*,#6269,.T.);
#8200=ORIENTED_EDGE('',*,*,#6270,.T.);
#8201=ORIENTED_EDGE('',*,*,#6268,.F.);
#8202=ORIENTED_EDGE('',*,*,#6271,.F.);
#8203=ORIENTED_EDGE('',*,*,#6272,.F.);
#8204=ORIENTED_EDGE('',*,*,#6273,.F.);
#8205=ORIENTED_EDGE('',*,*,#6274,.T.);
#8206=ORIENTED_EDGE('',*,*,#6275,.T.);
#8207=ORIENTED_EDGE('',*,*,#6276,.T.);
#8208=ORIENTED_EDGE('',*,*,#6277,.T.);
#8209=ORIENTED_EDGE('',*,*,#6275,.F.);
#8210=ORIENTED_EDGE('',*,*,#6278,.T.);
#8211=ORIENTED_EDGE('',*,*,#6279,.T.);
#8212=ORIENTED_EDGE('',*,*,#6280,.F.);
#8213=ORIENTED_EDGE('',*,*,#6281,.T.);
#8214=ORIENTED_EDGE('',*,*,#6282,.T.);
#8215=ORIENTED_EDGE('',*,*,#6283,.T.);
#8216=ORIENTED_EDGE('',*,*,#6284,.T.);
#8217=ORIENTED_EDGE('',*,*,#6282,.F.);
#8218=ORIENTED_EDGE('',*,*,#6285,.F.);
#8219=ORIENTED_EDGE('',*,*,#6286,.F.);
#8220=ORIENTED_EDGE('',*,*,#6287,.F.);
#8221=ORIENTED_EDGE('',*,*,#6288,.T.);
#8222=ORIENTED_EDGE('',*,*,#6289,.T.);
#8223=ORIENTED_EDGE('',*,*,#6290,.T.);
#8224=ORIENTED_EDGE('',*,*,#6291,.T.);
#8225=ORIENTED_EDGE('',*,*,#6289,.F.);
#8226=ORIENTED_EDGE('',*,*,#6292,.T.);
#8227=ORIENTED_EDGE('',*,*,#6293,.T.);
#8228=ORIENTED_EDGE('',*,*,#6294,.F.);
#8229=ORIENTED_EDGE('',*,*,#6295,.T.);
#8230=ORIENTED_EDGE('',*,*,#6296,.T.);
#8231=ORIENTED_EDGE('',*,*,#6297,.T.);
#8232=ORIENTED_EDGE('',*,*,#6298,.T.);
#8233=ORIENTED_EDGE('',*,*,#6296,.F.);
#8234=ORIENTED_EDGE('',*,*,#6299,.F.);
#8235=ORIENTED_EDGE('',*,*,#6300,.F.);
#8236=ORIENTED_EDGE('',*,*,#6301,.F.);
#8237=ORIENTED_EDGE('',*,*,#6302,.T.);
#8238=ORIENTED_EDGE('',*,*,#6303,.T.);
#8239=ORIENTED_EDGE('',*,*,#6304,.T.);
#8240=ORIENTED_EDGE('',*,*,#6305,.T.);
#8241=ORIENTED_EDGE('',*,*,#6303,.F.);
#8242=ORIENTED_EDGE('',*,*,#6306,.T.);
#8243=ORIENTED_EDGE('',*,*,#6307,.T.);
#8244=ORIENTED_EDGE('',*,*,#6308,.F.);
#8245=ORIENTED_EDGE('',*,*,#6309,.T.);
#8246=ORIENTED_EDGE('',*,*,#6310,.T.);
#8247=ORIENTED_EDGE('',*,*,#6311,.T.);
#8248=ORIENTED_EDGE('',*,*,#6312,.T.);
#8249=ORIENTED_EDGE('',*,*,#6310,.F.);
#8250=ORIENTED_EDGE('',*,*,#6313,.F.);
#8251=ORIENTED_EDGE('',*,*,#6314,.F.);
#8252=ORIENTED_EDGE('',*,*,#6315,.F.);
#8253=ORIENTED_EDGE('',*,*,#6316,.T.);
#8254=ORIENTED_EDGE('',*,*,#6317,.T.);
#8255=ORIENTED_EDGE('',*,*,#6318,.T.);
#8256=ORIENTED_EDGE('',*,*,#6319,.T.);
#8257=ORIENTED_EDGE('',*,*,#6317,.F.);
#8258=ORIENTED_EDGE('',*,*,#6320,.T.);
#8259=ORIENTED_EDGE('',*,*,#6321,.T.);
#8260=ORIENTED_EDGE('',*,*,#6322,.F.);
#8261=ORIENTED_EDGE('',*,*,#6323,.T.);
#8262=ORIENTED_EDGE('',*,*,#6324,.T.);
#8263=ORIENTED_EDGE('',*,*,#6325,.T.);
#8264=ORIENTED_EDGE('',*,*,#6326,.T.);
#8265=ORIENTED_EDGE('',*,*,#6324,.F.);
#8266=ORIENTED_EDGE('',*,*,#6327,.F.);
#8267=ORIENTED_EDGE('',*,*,#6328,.F.);
#8268=ORIENTED_EDGE('',*,*,#6329,.F.);
#8269=ORIENTED_EDGE('',*,*,#6330,.T.);
#8270=ORIENTED_EDGE('',*,*,#6331,.T.);
#8271=ORIENTED_EDGE('',*,*,#6332,.T.);
#8272=ORIENTED_EDGE('',*,*,#6333,.T.);
#8273=ORIENTED_EDGE('',*,*,#6331,.F.);
#8274=ORIENTED_EDGE('',*,*,#6334,.T.);
#8275=ORIENTED_EDGE('',*,*,#6335,.T.);
#8276=ORIENTED_EDGE('',*,*,#6336,.F.);
#8277=ORIENTED_EDGE('',*,*,#6337,.T.);
#8278=ORIENTED_EDGE('',*,*,#6338,.T.);
#8279=ORIENTED_EDGE('',*,*,#6339,.T.);
#8280=ORIENTED_EDGE('',*,*,#6340,.T.);
#8281=ORIENTED_EDGE('',*,*,#6338,.F.);
#8282=ORIENTED_EDGE('',*,*,#6341,.F.);
#8283=ORIENTED_EDGE('',*,*,#6342,.F.);
#8284=ORIENTED_EDGE('',*,*,#6343,.F.);
#8285=ORIENTED_EDGE('',*,*,#6344,.T.);
#8286=ORIENTED_EDGE('',*,*,#6345,.T.);
#8287=ORIENTED_EDGE('',*,*,#6346,.T.);
#8288=ORIENTED_EDGE('',*,*,#6347,.T.);
#8289=ORIENTED_EDGE('',*,*,#6345,.F.);
#8290=ORIENTED_EDGE('',*,*,#6348,.T.);
#8291=ORIENTED_EDGE('',*,*,#6349,.T.);
#8292=ORIENTED_EDGE('',*,*,#6350,.F.);
#8293=ORIENTED_EDGE('',*,*,#6351,.T.);
#8294=ORIENTED_EDGE('',*,*,#6352,.T.);
#8295=ORIENTED_EDGE('',*,*,#6353,.T.);
#8296=ORIENTED_EDGE('',*,*,#6354,.T.);
#8297=ORIENTED_EDGE('',*,*,#6352,.F.);
#8298=ORIENTED_EDGE('',*,*,#6355,.F.);
#8299=ORIENTED_EDGE('',*,*,#6356,.F.);
#8300=ORIENTED_EDGE('',*,*,#6357,.F.);
#8301=ORIENTED_EDGE('',*,*,#6358,.T.);
#8302=ORIENTED_EDGE('',*,*,#6359,.T.);
#8303=ORIENTED_EDGE('',*,*,#6360,.T.);
#8304=ORIENTED_EDGE('',*,*,#6361,.T.);
#8305=ORIENTED_EDGE('',*,*,#6359,.F.);
#8306=ORIENTED_EDGE('',*,*,#6362,.T.);
#8307=ORIENTED_EDGE('',*,*,#6363,.T.);
#8308=ORIENTED_EDGE('',*,*,#6364,.F.);
#8309=ORIENTED_EDGE('',*,*,#6365,.T.);
#8310=ORIENTED_EDGE('',*,*,#6366,.T.);
#8311=ORIENTED_EDGE('',*,*,#6367,.T.);
#8312=ORIENTED_EDGE('',*,*,#6368,.T.);
#8313=ORIENTED_EDGE('',*,*,#6366,.F.);
#8314=ORIENTED_EDGE('',*,*,#6369,.F.);
#8315=ORIENTED_EDGE('',*,*,#6370,.F.);
#8316=ORIENTED_EDGE('',*,*,#6371,.F.);
#8317=ORIENTED_EDGE('',*,*,#6372,.T.);
#8318=ORIENTED_EDGE('',*,*,#6373,.T.);
#8319=ORIENTED_EDGE('',*,*,#6374,.T.);
#8320=ORIENTED_EDGE('',*,*,#6375,.T.);
#8321=ORIENTED_EDGE('',*,*,#6373,.F.);
#8322=ORIENTED_EDGE('',*,*,#6376,.T.);
#8323=ORIENTED_EDGE('',*,*,#6377,.T.);
#8324=ORIENTED_EDGE('',*,*,#6378,.F.);
#8325=ORIENTED_EDGE('',*,*,#6379,.T.);
#8326=ORIENTED_EDGE('',*,*,#6380,.T.);
#8327=ORIENTED_EDGE('',*,*,#6381,.T.);
#8328=ORIENTED_EDGE('',*,*,#6382,.T.);
#8329=ORIENTED_EDGE('',*,*,#6380,.F.);
#8330=ORIENTED_EDGE('',*,*,#6383,.F.);
#8331=ORIENTED_EDGE('',*,*,#6384,.F.);
#8332=ORIENTED_EDGE('',*,*,#6385,.F.);
#8333=ORIENTED_EDGE('',*,*,#6386,.T.);
#8334=ORIENTED_EDGE('',*,*,#6387,.T.);
#8335=ORIENTED_EDGE('',*,*,#6388,.T.);
#8336=ORIENTED_EDGE('',*,*,#6389,.T.);
#8337=ORIENTED_EDGE('',*,*,#6387,.F.);
#8338=ORIENTED_EDGE('',*,*,#6390,.T.);
#8339=ORIENTED_EDGE('',*,*,#6391,.T.);
#8340=ORIENTED_EDGE('',*,*,#6392,.F.);
#8341=ORIENTED_EDGE('',*,*,#6393,.T.);
#8342=ORIENTED_EDGE('',*,*,#6394,.T.);
#8343=ORIENTED_EDGE('',*,*,#6395,.T.);
#8344=ORIENTED_EDGE('',*,*,#6396,.T.);
#8345=ORIENTED_EDGE('',*,*,#6394,.F.);
#8346=ORIENTED_EDGE('',*,*,#6397,.F.);
#8347=ORIENTED_EDGE('',*,*,#6398,.F.);
#8348=ORIENTED_EDGE('',*,*,#6399,.F.);
#8349=ORIENTED_EDGE('',*,*,#6400,.T.);
#8350=ORIENTED_EDGE('',*,*,#6401,.T.);
#8351=ORIENTED_EDGE('',*,*,#6402,.T.);
#8352=ORIENTED_EDGE('',*,*,#6403,.T.);
#8353=ORIENTED_EDGE('',*,*,#6401,.F.);
#8354=ORIENTED_EDGE('',*,*,#6404,.T.);
#8355=ORIENTED_EDGE('',*,*,#6405,.T.);
#8356=ORIENTED_EDGE('',*,*,#6406,.F.);
#8357=ORIENTED_EDGE('',*,*,#6407,.T.);
#8358=ORIENTED_EDGE('',*,*,#6408,.T.);
#8359=ORIENTED_EDGE('',*,*,#6409,.T.);
#8360=ORIENTED_EDGE('',*,*,#6410,.T.);
#8361=ORIENTED_EDGE('',*,*,#6408,.F.);
#8362=ORIENTED_EDGE('',*,*,#6411,.F.);
#8363=ORIENTED_EDGE('',*,*,#6412,.F.);
#8364=ORIENTED_EDGE('',*,*,#6413,.F.);
#8365=ORIENTED_EDGE('',*,*,#6414,.T.);
#8366=ORIENTED_EDGE('',*,*,#6415,.T.);
#8367=ORIENTED_EDGE('',*,*,#6416,.T.);
#8368=ORIENTED_EDGE('',*,*,#6417,.T.);
#8369=ORIENTED_EDGE('',*,*,#6415,.F.);
#8370=ORIENTED_EDGE('',*,*,#6418,.T.);
#8371=ORIENTED_EDGE('',*,*,#6419,.T.);
#8372=ORIENTED_EDGE('',*,*,#6420,.F.);
#8373=ORIENTED_EDGE('',*,*,#6421,.T.);
#8374=ORIENTED_EDGE('',*,*,#6422,.T.);
#8375=ORIENTED_EDGE('',*,*,#6423,.T.);
#8376=ORIENTED_EDGE('',*,*,#6424,.T.);
#8377=ORIENTED_EDGE('',*,*,#6422,.F.);
#8378=ORIENTED_EDGE('',*,*,#6425,.F.);
#8379=ORIENTED_EDGE('',*,*,#6426,.F.);
#8380=ORIENTED_EDGE('',*,*,#6427,.F.);
#8381=ORIENTED_EDGE('',*,*,#6428,.T.);
#8382=ORIENTED_EDGE('',*,*,#6429,.T.);
#8383=ORIENTED_EDGE('',*,*,#6430,.T.);
#8384=ORIENTED_EDGE('',*,*,#6431,.T.);
#8385=ORIENTED_EDGE('',*,*,#6429,.F.);
#8386=ORIENTED_EDGE('',*,*,#6432,.T.);
#8387=ORIENTED_EDGE('',*,*,#6433,.T.);
#8388=ORIENTED_EDGE('',*,*,#6434,.F.);
#8389=ORIENTED_EDGE('',*,*,#6435,.T.);
#8390=ORIENTED_EDGE('',*,*,#6436,.T.);
#8391=ORIENTED_EDGE('',*,*,#6437,.T.);
#8392=ORIENTED_EDGE('',*,*,#6438,.T.);
#8393=ORIENTED_EDGE('',*,*,#6436,.F.);
#8394=ORIENTED_EDGE('',*,*,#6439,.F.);
#8395=ORIENTED_EDGE('',*,*,#6440,.F.);
#8396=ORIENTED_EDGE('',*,*,#6441,.F.);
#8397=ORIENTED_EDGE('',*,*,#6442,.T.);
#8398=ORIENTED_EDGE('',*,*,#6443,.T.);
#8399=ORIENTED_EDGE('',*,*,#6444,.T.);
#8400=ORIENTED_EDGE('',*,*,#6445,.T.);
#8401=ORIENTED_EDGE('',*,*,#6443,.F.);
#8402=ORIENTED_EDGE('',*,*,#6446,.T.);
#8403=ORIENTED_EDGE('',*,*,#6447,.T.);
#8404=ORIENTED_EDGE('',*,*,#6448,.F.);
#8405=ORIENTED_EDGE('',*,*,#6449,.T.);
#8406=ORIENTED_EDGE('',*,*,#6450,.T.);
#8407=ORIENTED_EDGE('',*,*,#6451,.T.);
#8408=ORIENTED_EDGE('',*,*,#6452,.T.);
#8409=ORIENTED_EDGE('',*,*,#6450,.F.);
#8410=ORIENTED_EDGE('',*,*,#6453,.F.);
#8411=ORIENTED_EDGE('',*,*,#6454,.F.);
#8412=ORIENTED_EDGE('',*,*,#6455,.F.);
#8413=ORIENTED_EDGE('',*,*,#6456,.T.);
#8414=ORIENTED_EDGE('',*,*,#6457,.T.);
#8415=ORIENTED_EDGE('',*,*,#6458,.T.);
#8416=ORIENTED_EDGE('',*,*,#6459,.T.);
#8417=ORIENTED_EDGE('',*,*,#6457,.F.);
#8418=ORIENTED_EDGE('',*,*,#6460,.T.);
#8419=ORIENTED_EDGE('',*,*,#6461,.T.);
#8420=ORIENTED_EDGE('',*,*,#6462,.F.);
#8421=ORIENTED_EDGE('',*,*,#6463,.T.);
#8422=ORIENTED_EDGE('',*,*,#6464,.T.);
#8423=ORIENTED_EDGE('',*,*,#6465,.T.);
#8424=ORIENTED_EDGE('',*,*,#6466,.T.);
#8425=ORIENTED_EDGE('',*,*,#6464,.F.);
#8426=ORIENTED_EDGE('',*,*,#6467,.F.);
#8427=ORIENTED_EDGE('',*,*,#6468,.F.);
#8428=ORIENTED_EDGE('',*,*,#6469,.F.);
#8429=ORIENTED_EDGE('',*,*,#6470,.T.);
#8430=ORIENTED_EDGE('',*,*,#6471,.T.);
#8431=ORIENTED_EDGE('',*,*,#6472,.T.);
#8432=ORIENTED_EDGE('',*,*,#6473,.T.);
#8433=ORIENTED_EDGE('',*,*,#6471,.F.);
#8434=ORIENTED_EDGE('',*,*,#6474,.T.);
#8435=ORIENTED_EDGE('',*,*,#6475,.T.);
#8436=ORIENTED_EDGE('',*,*,#6476,.F.);
#8437=ORIENTED_EDGE('',*,*,#6477,.T.);
#8438=ORIENTED_EDGE('',*,*,#6478,.T.);
#8439=ORIENTED_EDGE('',*,*,#6479,.T.);
#8440=ORIENTED_EDGE('',*,*,#6480,.T.);
#8441=ORIENTED_EDGE('',*,*,#6478,.F.);
#8442=ORIENTED_EDGE('',*,*,#6481,.F.);
#8443=ORIENTED_EDGE('',*,*,#6482,.F.);
#8444=ORIENTED_EDGE('',*,*,#6483,.F.);
#8445=ORIENTED_EDGE('',*,*,#6484,.T.);
#8446=ORIENTED_EDGE('',*,*,#6485,.T.);
#8447=ORIENTED_EDGE('',*,*,#6486,.T.);
#8448=ORIENTED_EDGE('',*,*,#6487,.T.);
#8449=ORIENTED_EDGE('',*,*,#6485,.F.);
#8450=ORIENTED_EDGE('',*,*,#6488,.T.);
#8451=ORIENTED_EDGE('',*,*,#6489,.T.);
#8452=ORIENTED_EDGE('',*,*,#6490,.F.);
#8453=ORIENTED_EDGE('',*,*,#6491,.T.);
#8454=ORIENTED_EDGE('',*,*,#6492,.T.);
#8455=ORIENTED_EDGE('',*,*,#6493,.T.);
#8456=ORIENTED_EDGE('',*,*,#6494,.T.);
#8457=ORIENTED_EDGE('',*,*,#6492,.F.);
#8458=ORIENTED_EDGE('',*,*,#6495,.F.);
#8459=ORIENTED_EDGE('',*,*,#6496,.F.);
#8460=ORIENTED_EDGE('',*,*,#6497,.F.);
#8461=ORIENTED_EDGE('',*,*,#6498,.T.);
#8462=ORIENTED_EDGE('',*,*,#6499,.T.);
#8463=ORIENTED_EDGE('',*,*,#6500,.T.);
#8464=ORIENTED_EDGE('',*,*,#6501,.T.);
#8465=ORIENTED_EDGE('',*,*,#6499,.F.);
#8466=ORIENTED_EDGE('',*,*,#6502,.T.);
#8467=ORIENTED_EDGE('',*,*,#6503,.T.);
#8468=ORIENTED_EDGE('',*,*,#6504,.F.);
#8469=ORIENTED_EDGE('',*,*,#6505,.T.);
#8470=ORIENTED_EDGE('',*,*,#6506,.T.);
#8471=ORIENTED_EDGE('',*,*,#6507,.T.);
#8472=ORIENTED_EDGE('',*,*,#6508,.T.);
#8473=ORIENTED_EDGE('',*,*,#6506,.F.);
#8474=ORIENTED_EDGE('',*,*,#6509,.F.);
#8475=ORIENTED_EDGE('',*,*,#6510,.F.);
#8476=ORIENTED_EDGE('',*,*,#6511,.F.);
#8477=ORIENTED_EDGE('',*,*,#6512,.T.);
#8478=ORIENTED_EDGE('',*,*,#6513,.T.);
#8479=ORIENTED_EDGE('',*,*,#6514,.T.);
#8480=ORIENTED_EDGE('',*,*,#6515,.T.);
#8481=ORIENTED_EDGE('',*,*,#6513,.F.);
#8482=ORIENTED_EDGE('',*,*,#6516,.T.);
#8483=ORIENTED_EDGE('',*,*,#6517,.T.);
#8484=ORIENTED_EDGE('',*,*,#6518,.F.);
#8485=ORIENTED_EDGE('',*,*,#6519,.F.);
#8486=ORIENTED_EDGE('',*,*,#6258,.T.);
#8487=ORIENTED_EDGE('',*,*,#6520,.F.);
#8488=ORIENTED_EDGE('',*,*,#6521,.F.);
#8489=ORIENTED_EDGE('',*,*,#6522,.T.);
#8490=ORIENTED_EDGE('',*,*,#6521,.T.);
#8491=ORIENTED_EDGE('',*,*,#6523,.F.);
#8492=ORIENTED_EDGE('',*,*,#6524,.F.);
#8493=ORIENTED_EDGE('',*,*,#6525,.T.);
#8494=ORIENTED_EDGE('',*,*,#6524,.T.);
#8495=ORIENTED_EDGE('',*,*,#6526,.F.);
#8496=ORIENTED_EDGE('',*,*,#6265,.F.);
#8497=ORIENTED_EDGE('',*,*,#6527,.F.);
#8498=ORIENTED_EDGE('',*,*,#6272,.T.);
#8499=ORIENTED_EDGE('',*,*,#6528,.F.);
#8500=ORIENTED_EDGE('',*,*,#6529,.F.);
#8501=ORIENTED_EDGE('',*,*,#6530,.T.);
#8502=ORIENTED_EDGE('',*,*,#6529,.T.);
#8503=ORIENTED_EDGE('',*,*,#6531,.F.);
#8504=ORIENTED_EDGE('',*,*,#6532,.F.);
#8505=ORIENTED_EDGE('',*,*,#6533,.T.);
#8506=ORIENTED_EDGE('',*,*,#6532,.T.);
#8507=ORIENTED_EDGE('',*,*,#6534,.F.);
#8508=ORIENTED_EDGE('',*,*,#6279,.F.);
#8509=ORIENTED_EDGE('',*,*,#6535,.F.);
#8510=ORIENTED_EDGE('',*,*,#6286,.T.);
#8511=ORIENTED_EDGE('',*,*,#6536,.F.);
#8512=ORIENTED_EDGE('',*,*,#6537,.F.);
#8513=ORIENTED_EDGE('',*,*,#6538,.T.);
#8514=ORIENTED_EDGE('',*,*,#6537,.T.);
#8515=ORIENTED_EDGE('',*,*,#6539,.F.);
#8516=ORIENTED_EDGE('',*,*,#6540,.F.);
#8517=ORIENTED_EDGE('',*,*,#6541,.T.);
#8518=ORIENTED_EDGE('',*,*,#6540,.T.);
#8519=ORIENTED_EDGE('',*,*,#6542,.F.);
#8520=ORIENTED_EDGE('',*,*,#6293,.F.);
#8521=ORIENTED_EDGE('',*,*,#6543,.F.);
#8522=ORIENTED_EDGE('',*,*,#6300,.T.);
#8523=ORIENTED_EDGE('',*,*,#6544,.F.);
#8524=ORIENTED_EDGE('',*,*,#6545,.F.);
#8525=ORIENTED_EDGE('',*,*,#6546,.T.);
#8526=ORIENTED_EDGE('',*,*,#6545,.T.);
#8527=ORIENTED_EDGE('',*,*,#6547,.F.);
#8528=ORIENTED_EDGE('',*,*,#6548,.F.);
#8529=ORIENTED_EDGE('',*,*,#6549,.T.);
#8530=ORIENTED_EDGE('',*,*,#6548,.T.);
#8531=ORIENTED_EDGE('',*,*,#6550,.F.);
#8532=ORIENTED_EDGE('',*,*,#6307,.F.);
#8533=ORIENTED_EDGE('',*,*,#6551,.F.);
#8534=ORIENTED_EDGE('',*,*,#6314,.T.);
#8535=ORIENTED_EDGE('',*,*,#6552,.F.);
#8536=ORIENTED_EDGE('',*,*,#6553,.F.);
#8537=ORIENTED_EDGE('',*,*,#6554,.T.);
#8538=ORIENTED_EDGE('',*,*,#6553,.T.);
#8539=ORIENTED_EDGE('',*,*,#6555,.F.);
#8540=ORIENTED_EDGE('',*,*,#6556,.F.);
#8541=ORIENTED_EDGE('',*,*,#6557,.T.);
#8542=ORIENTED_EDGE('',*,*,#6556,.T.);
#8543=ORIENTED_EDGE('',*,*,#6558,.F.);
#8544=ORIENTED_EDGE('',*,*,#6321,.F.);
#8545=ORIENTED_EDGE('',*,*,#6559,.F.);
#8546=ORIENTED_EDGE('',*,*,#6328,.T.);
#8547=ORIENTED_EDGE('',*,*,#6560,.F.);
#8548=ORIENTED_EDGE('',*,*,#6561,.F.);
#8549=ORIENTED_EDGE('',*,*,#6562,.T.);
#8550=ORIENTED_EDGE('',*,*,#6561,.T.);
#8551=ORIENTED_EDGE('',*,*,#6563,.F.);
#8552=ORIENTED_EDGE('',*,*,#6564,.F.);
#8553=ORIENTED_EDGE('',*,*,#6565,.T.);
#8554=ORIENTED_EDGE('',*,*,#6564,.T.);
#8555=ORIENTED_EDGE('',*,*,#6566,.F.);
#8556=ORIENTED_EDGE('',*,*,#6335,.F.);
#8557=ORIENTED_EDGE('',*,*,#6567,.F.);
#8558=ORIENTED_EDGE('',*,*,#6342,.T.);
#8559=ORIENTED_EDGE('',*,*,#6568,.F.);
#8560=ORIENTED_EDGE('',*,*,#6569,.F.);
#8561=ORIENTED_EDGE('',*,*,#6570,.T.);
#8562=ORIENTED_EDGE('',*,*,#6569,.T.);
#8563=ORIENTED_EDGE('',*,*,#6571,.F.);
#8564=ORIENTED_EDGE('',*,*,#6572,.F.);
#8565=ORIENTED_EDGE('',*,*,#6573,.T.);
#8566=ORIENTED_EDGE('',*,*,#6572,.T.);
#8567=ORIENTED_EDGE('',*,*,#6574,.F.);
#8568=ORIENTED_EDGE('',*,*,#6349,.F.);
#8569=ORIENTED_EDGE('',*,*,#6575,.F.);
#8570=ORIENTED_EDGE('',*,*,#6356,.T.);
#8571=ORIENTED_EDGE('',*,*,#6576,.F.);
#8572=ORIENTED_EDGE('',*,*,#6577,.F.);
#8573=ORIENTED_EDGE('',*,*,#6578,.T.);
#8574=ORIENTED_EDGE('',*,*,#6577,.T.);
#8575=ORIENTED_EDGE('',*,*,#6579,.F.);
#8576=ORIENTED_EDGE('',*,*,#6580,.F.);
#8577=ORIENTED_EDGE('',*,*,#6581,.T.);
#8578=ORIENTED_EDGE('',*,*,#6580,.T.);
#8579=ORIENTED_EDGE('',*,*,#6582,.F.);
#8580=ORIENTED_EDGE('',*,*,#6363,.F.);
#8581=ORIENTED_EDGE('',*,*,#6583,.F.);
#8582=ORIENTED_EDGE('',*,*,#6370,.T.);
#8583=ORIENTED_EDGE('',*,*,#6584,.F.);
#8584=ORIENTED_EDGE('',*,*,#6585,.F.);
#8585=ORIENTED_EDGE('',*,*,#6586,.T.);
#8586=ORIENTED_EDGE('',*,*,#6585,.T.);
#8587=ORIENTED_EDGE('',*,*,#6587,.F.);
#8588=ORIENTED_EDGE('',*,*,#6588,.F.);
#8589=ORIENTED_EDGE('',*,*,#6589,.T.);
#8590=ORIENTED_EDGE('',*,*,#6588,.T.);
#8591=ORIENTED_EDGE('',*,*,#6590,.F.);
#8592=ORIENTED_EDGE('',*,*,#6377,.F.);
#8593=ORIENTED_EDGE('',*,*,#6591,.F.);
#8594=ORIENTED_EDGE('',*,*,#6384,.T.);
#8595=ORIENTED_EDGE('',*,*,#6592,.F.);
#8596=ORIENTED_EDGE('',*,*,#6593,.F.);
#8597=ORIENTED_EDGE('',*,*,#6594,.T.);
#8598=ORIENTED_EDGE('',*,*,#6593,.T.);
#8599=ORIENTED_EDGE('',*,*,#6595,.F.);
#8600=ORIENTED_EDGE('',*,*,#6596,.F.);
#8601=ORIENTED_EDGE('',*,*,#6597,.T.);
#8602=ORIENTED_EDGE('',*,*,#6596,.T.);
#8603=ORIENTED_EDGE('',*,*,#6598,.F.);
#8604=ORIENTED_EDGE('',*,*,#6391,.F.);
#8605=ORIENTED_EDGE('',*,*,#6599,.F.);
#8606=ORIENTED_EDGE('',*,*,#6398,.T.);
#8607=ORIENTED_EDGE('',*,*,#6600,.F.);
#8608=ORIENTED_EDGE('',*,*,#6601,.F.);
#8609=ORIENTED_EDGE('',*,*,#6602,.T.);
#8610=ORIENTED_EDGE('',*,*,#6601,.T.);
#8611=ORIENTED_EDGE('',*,*,#6603,.F.);
#8612=ORIENTED_EDGE('',*,*,#6604,.F.);
#8613=ORIENTED_EDGE('',*,*,#6605,.T.);
#8614=ORIENTED_EDGE('',*,*,#6604,.T.);
#8615=ORIENTED_EDGE('',*,*,#6606,.F.);
#8616=ORIENTED_EDGE('',*,*,#6405,.F.);
#8617=ORIENTED_EDGE('',*,*,#6607,.F.);
#8618=ORIENTED_EDGE('',*,*,#6412,.T.);
#8619=ORIENTED_EDGE('',*,*,#6608,.F.);
#8620=ORIENTED_EDGE('',*,*,#6609,.F.);
#8621=ORIENTED_EDGE('',*,*,#6610,.T.);
#8622=ORIENTED_EDGE('',*,*,#6609,.T.);
#8623=ORIENTED_EDGE('',*,*,#6611,.F.);
#8624=ORIENTED_EDGE('',*,*,#6612,.F.);
#8625=ORIENTED_EDGE('',*,*,#6613,.T.);
#8626=ORIENTED_EDGE('',*,*,#6612,.T.);
#8627=ORIENTED_EDGE('',*,*,#6614,.F.);
#8628=ORIENTED_EDGE('',*,*,#6419,.F.);
#8629=ORIENTED_EDGE('',*,*,#6615,.F.);
#8630=ORIENTED_EDGE('',*,*,#6426,.T.);
#8631=ORIENTED_EDGE('',*,*,#6616,.F.);
#8632=ORIENTED_EDGE('',*,*,#6617,.F.);
#8633=ORIENTED_EDGE('',*,*,#6618,.T.);
#8634=ORIENTED_EDGE('',*,*,#6617,.T.);
#8635=ORIENTED_EDGE('',*,*,#6619,.F.);
#8636=ORIENTED_EDGE('',*,*,#6620,.F.);
#8637=ORIENTED_EDGE('',*,*,#6621,.T.);
#8638=ORIENTED_EDGE('',*,*,#6620,.T.);
#8639=ORIENTED_EDGE('',*,*,#6622,.F.);
#8640=ORIENTED_EDGE('',*,*,#6433,.F.);
#8641=ORIENTED_EDGE('',*,*,#6623,.F.);
#8642=ORIENTED_EDGE('',*,*,#6440,.T.);
#8643=ORIENTED_EDGE('',*,*,#6624,.F.);
#8644=ORIENTED_EDGE('',*,*,#6625,.F.);
#8645=ORIENTED_EDGE('',*,*,#6626,.T.);
#8646=ORIENTED_EDGE('',*,*,#6625,.T.);
#8647=ORIENTED_EDGE('',*,*,#6627,.F.);
#8648=ORIENTED_EDGE('',*,*,#6628,.F.);
#8649=ORIENTED_EDGE('',*,*,#6629,.T.);
#8650=ORIENTED_EDGE('',*,*,#6628,.T.);
#8651=ORIENTED_EDGE('',*,*,#6630,.F.);
#8652=ORIENTED_EDGE('',*,*,#6447,.F.);
#8653=ORIENTED_EDGE('',*,*,#6631,.F.);
#8654=ORIENTED_EDGE('',*,*,#6454,.T.);
#8655=ORIENTED_EDGE('',*,*,#6632,.F.);
#8656=ORIENTED_EDGE('',*,*,#6633,.F.);
#8657=ORIENTED_EDGE('',*,*,#6634,.T.);
#8658=ORIENTED_EDGE('',*,*,#6633,.T.);
#8659=ORIENTED_EDGE('',*,*,#6635,.F.);
#8660=ORIENTED_EDGE('',*,*,#6636,.F.);
#8661=ORIENTED_EDGE('',*,*,#6637,.T.);
#8662=ORIENTED_EDGE('',*,*,#6636,.T.);
#8663=ORIENTED_EDGE('',*,*,#6638,.F.);
#8664=ORIENTED_EDGE('',*,*,#6461,.F.);
#8665=ORIENTED_EDGE('',*,*,#6639,.F.);
#8666=ORIENTED_EDGE('',*,*,#6468,.T.);
#8667=ORIENTED_EDGE('',*,*,#6640,.F.);
#8668=ORIENTED_EDGE('',*,*,#6641,.F.);
#8669=ORIENTED_EDGE('',*,*,#6642,.T.);
#8670=ORIENTED_EDGE('',*,*,#6641,.T.);
#8671=ORIENTED_EDGE('',*,*,#6643,.F.);
#8672=ORIENTED_EDGE('',*,*,#6644,.F.);
#8673=ORIENTED_EDGE('',*,*,#6645,.T.);
#8674=ORIENTED_EDGE('',*,*,#6644,.T.);
#8675=ORIENTED_EDGE('',*,*,#6646,.F.);
#8676=ORIENTED_EDGE('',*,*,#6475,.F.);
#8677=ORIENTED_EDGE('',*,*,#6647,.F.);
#8678=ORIENTED_EDGE('',*,*,#6482,.T.);
#8679=ORIENTED_EDGE('',*,*,#6648,.F.);
#8680=ORIENTED_EDGE('',*,*,#6649,.F.);
#8681=ORIENTED_EDGE('',*,*,#6650,.T.);
#8682=ORIENTED_EDGE('',*,*,#6649,.T.);
#8683=ORIENTED_EDGE('',*,*,#6651,.F.);
#8684=ORIENTED_EDGE('',*,*,#6652,.F.);
#8685=ORIENTED_EDGE('',*,*,#6653,.T.);
#8686=ORIENTED_EDGE('',*,*,#6652,.T.);
#8687=ORIENTED_EDGE('',*,*,#6654,.F.);
#8688=ORIENTED_EDGE('',*,*,#6489,.F.);
#8689=ORIENTED_EDGE('',*,*,#6655,.F.);
#8690=ORIENTED_EDGE('',*,*,#6496,.T.);
#8691=ORIENTED_EDGE('',*,*,#6656,.F.);
#8692=ORIENTED_EDGE('',*,*,#6657,.F.);
#8693=ORIENTED_EDGE('',*,*,#6658,.T.);
#8694=ORIENTED_EDGE('',*,*,#6657,.T.);
#8695=ORIENTED_EDGE('',*,*,#6659,.F.);
#8696=ORIENTED_EDGE('',*,*,#6660,.F.);
#8697=ORIENTED_EDGE('',*,*,#6661,.T.);
#8698=ORIENTED_EDGE('',*,*,#6660,.T.);
#8699=ORIENTED_EDGE('',*,*,#6662,.F.);
#8700=ORIENTED_EDGE('',*,*,#6503,.F.);
#8701=ORIENTED_EDGE('',*,*,#6663,.F.);
#8702=ORIENTED_EDGE('',*,*,#6510,.T.);
#8703=ORIENTED_EDGE('',*,*,#6664,.F.);
#8704=ORIENTED_EDGE('',*,*,#6665,.F.);
#8705=ORIENTED_EDGE('',*,*,#6666,.T.);
#8706=ORIENTED_EDGE('',*,*,#6665,.T.);
#8707=ORIENTED_EDGE('',*,*,#6667,.F.);
#8708=ORIENTED_EDGE('',*,*,#6668,.F.);
#8709=ORIENTED_EDGE('',*,*,#6669,.T.);
#8710=ORIENTED_EDGE('',*,*,#6668,.T.);
#8711=ORIENTED_EDGE('',*,*,#6670,.F.);
#8712=ORIENTED_EDGE('',*,*,#6517,.F.);
#8713=ORIENTED_EDGE('',*,*,#6269,.F.);
#8714=ORIENTED_EDGE('',*,*,#6273,.T.);
#8715=ORIENTED_EDGE('',*,*,#6527,.T.);
#8716=ORIENTED_EDGE('',*,*,#6530,.F.);
#8717=ORIENTED_EDGE('',*,*,#6533,.F.);
#8718=ORIENTED_EDGE('',*,*,#6278,.F.);
#8719=ORIENTED_EDGE('',*,*,#6274,.F.);
#8720=ORIENTED_EDGE('',*,*,#6671,.F.);
#8721=ORIENTED_EDGE('',*,*,#6283,.F.);
#8722=ORIENTED_EDGE('',*,*,#6287,.T.);
#8723=ORIENTED_EDGE('',*,*,#6535,.T.);
#8724=ORIENTED_EDGE('',*,*,#6538,.F.);
#8725=ORIENTED_EDGE('',*,*,#6541,.F.);
#8726=ORIENTED_EDGE('',*,*,#6292,.F.);
#8727=ORIENTED_EDGE('',*,*,#6288,.F.);
#8728=ORIENTED_EDGE('',*,*,#6672,.F.);
#8729=ORIENTED_EDGE('',*,*,#6297,.F.);
#8730=ORIENTED_EDGE('',*,*,#6301,.T.);
#8731=ORIENTED_EDGE('',*,*,#6543,.T.);
#8732=ORIENTED_EDGE('',*,*,#6546,.F.);
#8733=ORIENTED_EDGE('',*,*,#6549,.F.);
#8734=ORIENTED_EDGE('',*,*,#6306,.F.);
#8735=ORIENTED_EDGE('',*,*,#6302,.F.);
#8736=ORIENTED_EDGE('',*,*,#6673,.F.);
#8737=ORIENTED_EDGE('',*,*,#6311,.F.);
#8738=ORIENTED_EDGE('',*,*,#6315,.T.);
#8739=ORIENTED_EDGE('',*,*,#6551,.T.);
#8740=ORIENTED_EDGE('',*,*,#6554,.F.);
#8741=ORIENTED_EDGE('',*,*,#6557,.F.);
#8742=ORIENTED_EDGE('',*,*,#6320,.F.);
#8743=ORIENTED_EDGE('',*,*,#6316,.F.);
#8744=ORIENTED_EDGE('',*,*,#6674,.F.);
#8745=ORIENTED_EDGE('',*,*,#6325,.F.);
#8746=ORIENTED_EDGE('',*,*,#6329,.T.);
#8747=ORIENTED_EDGE('',*,*,#6559,.T.);
#8748=ORIENTED_EDGE('',*,*,#6562,.F.);
#8749=ORIENTED_EDGE('',*,*,#6565,.F.);
#8750=ORIENTED_EDGE('',*,*,#6334,.F.);
#8751=ORIENTED_EDGE('',*,*,#6330,.F.);
#8752=ORIENTED_EDGE('',*,*,#6675,.F.);
#8753=ORIENTED_EDGE('',*,*,#6339,.F.);
#8754=ORIENTED_EDGE('',*,*,#6343,.T.);
#8755=ORIENTED_EDGE('',*,*,#6567,.T.);
#8756=ORIENTED_EDGE('',*,*,#6570,.F.);
#8757=ORIENTED_EDGE('',*,*,#6573,.F.);
#8758=ORIENTED_EDGE('',*,*,#6348,.F.);
#8759=ORIENTED_EDGE('',*,*,#6344,.F.);
#8760=ORIENTED_EDGE('',*,*,#6676,.F.);
#8761=ORIENTED_EDGE('',*,*,#6353,.F.);
#8762=ORIENTED_EDGE('',*,*,#6357,.T.);
#8763=ORIENTED_EDGE('',*,*,#6575,.T.);
#8764=ORIENTED_EDGE('',*,*,#6578,.F.);
#8765=ORIENTED_EDGE('',*,*,#6581,.F.);
#8766=ORIENTED_EDGE('',*,*,#6362,.F.);
#8767=ORIENTED_EDGE('',*,*,#6358,.F.);
#8768=ORIENTED_EDGE('',*,*,#6677,.F.);
#8769=ORIENTED_EDGE('',*,*,#6367,.F.);
#8770=ORIENTED_EDGE('',*,*,#6371,.T.);
#8771=ORIENTED_EDGE('',*,*,#6583,.T.);
#8772=ORIENTED_EDGE('',*,*,#6586,.F.);
#8773=ORIENTED_EDGE('',*,*,#6589,.F.);
#8774=ORIENTED_EDGE('',*,*,#6376,.F.);
#8775=ORIENTED_EDGE('',*,*,#6372,.F.);
#8776=ORIENTED_EDGE('',*,*,#6678,.F.);
#8777=ORIENTED_EDGE('',*,*,#6381,.F.);
#8778=ORIENTED_EDGE('',*,*,#6385,.T.);
#8779=ORIENTED_EDGE('',*,*,#6591,.T.);
#8780=ORIENTED_EDGE('',*,*,#6594,.F.);
#8781=ORIENTED_EDGE('',*,*,#6597,.F.);
#8782=ORIENTED_EDGE('',*,*,#6390,.F.);
#8783=ORIENTED_EDGE('',*,*,#6386,.F.);
#8784=ORIENTED_EDGE('',*,*,#6679,.F.);
#8785=ORIENTED_EDGE('',*,*,#6395,.F.);
#8786=ORIENTED_EDGE('',*,*,#6399,.T.);
#8787=ORIENTED_EDGE('',*,*,#6599,.T.);
#8788=ORIENTED_EDGE('',*,*,#6602,.F.);
#8789=ORIENTED_EDGE('',*,*,#6605,.F.);
#8790=ORIENTED_EDGE('',*,*,#6404,.F.);
#8791=ORIENTED_EDGE('',*,*,#6400,.F.);
#8792=ORIENTED_EDGE('',*,*,#6680,.F.);
#8793=ORIENTED_EDGE('',*,*,#6409,.F.);
#8794=ORIENTED_EDGE('',*,*,#6413,.T.);
#8795=ORIENTED_EDGE('',*,*,#6607,.T.);
#8796=ORIENTED_EDGE('',*,*,#6610,.F.);
#8797=ORIENTED_EDGE('',*,*,#6613,.F.);
#8798=ORIENTED_EDGE('',*,*,#6418,.F.);
#8799=ORIENTED_EDGE('',*,*,#6414,.F.);
#8800=ORIENTED_EDGE('',*,*,#6681,.F.);
#8801=ORIENTED_EDGE('',*,*,#6423,.F.);
#8802=ORIENTED_EDGE('',*,*,#6427,.T.);
#8803=ORIENTED_EDGE('',*,*,#6615,.T.);
#8804=ORIENTED_EDGE('',*,*,#6618,.F.);
#8805=ORIENTED_EDGE('',*,*,#6621,.F.);
#8806=ORIENTED_EDGE('',*,*,#6432,.F.);
#8807=ORIENTED_EDGE('',*,*,#6428,.F.);
#8808=ORIENTED_EDGE('',*,*,#6682,.F.);
#8809=ORIENTED_EDGE('',*,*,#6437,.F.);
#8810=ORIENTED_EDGE('',*,*,#6441,.T.);
#8811=ORIENTED_EDGE('',*,*,#6623,.T.);
#8812=ORIENTED_EDGE('',*,*,#6626,.F.);
#8813=ORIENTED_EDGE('',*,*,#6629,.F.);
#8814=ORIENTED_EDGE('',*,*,#6446,.F.);
#8815=ORIENTED_EDGE('',*,*,#6442,.F.);
#8816=ORIENTED_EDGE('',*,*,#6683,.F.);
#8817=ORIENTED_EDGE('',*,*,#6451,.F.);
#8818=ORIENTED_EDGE('',*,*,#6455,.T.);
#8819=ORIENTED_EDGE('',*,*,#6631,.T.);
#8820=ORIENTED_EDGE('',*,*,#6634,.F.);
#8821=ORIENTED_EDGE('',*,*,#6637,.F.);
#8822=ORIENTED_EDGE('',*,*,#6460,.F.);
#8823=ORIENTED_EDGE('',*,*,#6456,.F.);
#8824=ORIENTED_EDGE('',*,*,#6684,.F.);
#8825=ORIENTED_EDGE('',*,*,#6465,.F.);
#8826=ORIENTED_EDGE('',*,*,#6469,.T.);
#8827=ORIENTED_EDGE('',*,*,#6639,.T.);
#8828=ORIENTED_EDGE('',*,*,#6642,.F.);
#8829=ORIENTED_EDGE('',*,*,#6645,.F.);
#8830=ORIENTED_EDGE('',*,*,#6474,.F.);
#8831=ORIENTED_EDGE('',*,*,#6470,.F.);
#8832=ORIENTED_EDGE('',*,*,#6685,.F.);
#8833=ORIENTED_EDGE('',*,*,#6479,.F.);
#8834=ORIENTED_EDGE('',*,*,#6483,.T.);
#8835=ORIENTED_EDGE('',*,*,#6647,.T.);
#8836=ORIENTED_EDGE('',*,*,#6650,.F.);
#8837=ORIENTED_EDGE('',*,*,#6653,.F.);
#8838=ORIENTED_EDGE('',*,*,#6488,.F.);
#8839=ORIENTED_EDGE('',*,*,#6484,.F.);
#8840=ORIENTED_EDGE('',*,*,#6686,.F.);
#8841=ORIENTED_EDGE('',*,*,#6493,.F.);
#8842=ORIENTED_EDGE('',*,*,#6497,.T.);
#8843=ORIENTED_EDGE('',*,*,#6655,.T.);
#8844=ORIENTED_EDGE('',*,*,#6658,.F.);
#8845=ORIENTED_EDGE('',*,*,#6661,.F.);
#8846=ORIENTED_EDGE('',*,*,#6502,.F.);
#8847=ORIENTED_EDGE('',*,*,#6498,.F.);
#8848=ORIENTED_EDGE('',*,*,#6687,.F.);
#8849=ORIENTED_EDGE('',*,*,#6507,.F.);
#8850=ORIENTED_EDGE('',*,*,#6511,.T.);
#8851=ORIENTED_EDGE('',*,*,#6663,.T.);
#8852=ORIENTED_EDGE('',*,*,#6666,.F.);
#8853=ORIENTED_EDGE('',*,*,#6669,.F.);
#8854=ORIENTED_EDGE('',*,*,#6516,.F.);
#8855=ORIENTED_EDGE('',*,*,#6512,.F.);
#8856=ORIENTED_EDGE('',*,*,#6688,.F.);
#8857=ORIENTED_EDGE('',*,*,#6689,.F.);
#8858=ORIENTED_EDGE('',*,*,#6690,.T.);
#8859=ORIENTED_EDGE('',*,*,#6691,.T.);
#8860=ORIENTED_EDGE('',*,*,#6692,.F.);
#8861=ORIENTED_EDGE('',*,*,#6693,.F.);
#8862=ORIENTED_EDGE('',*,*,#6694,.F.);
#8863=ORIENTED_EDGE('',*,*,#6695,.F.);
#8864=ORIENTED_EDGE('',*,*,#6696,.F.);
#8865=ORIENTED_EDGE('',*,*,#6255,.F.);
#8866=ORIENTED_EDGE('',*,*,#6259,.T.);
#8867=ORIENTED_EDGE('',*,*,#6519,.T.);
#8868=ORIENTED_EDGE('',*,*,#6522,.F.);
#8869=ORIENTED_EDGE('',*,*,#6525,.F.);
#8870=ORIENTED_EDGE('',*,*,#6264,.F.);
#8871=ORIENTED_EDGE('',*,*,#6260,.F.);
#8872=ORIENTED_EDGE('',*,*,#6697,.F.);
#8873=ORIENTED_EDGE('',*,*,#6252,.T.);
#8874=ORIENTED_EDGE('',*,*,#6698,.T.);
#8875=ORIENTED_EDGE('',*,*,#6699,.F.);
#8876=ORIENTED_EDGE('',*,*,#6700,.T.);
#8877=ORIENTED_EDGE('',*,*,#6701,.T.);
#8878=ORIENTED_EDGE('',*,*,#6702,.T.);
#8879=ORIENTED_EDGE('',*,*,#6703,.T.);
#8880=ORIENTED_EDGE('',*,*,#6704,.T.);
#8881=ORIENTED_EDGE('',*,*,#6705,.F.);
#8882=ORIENTED_EDGE('',*,*,#6706,.T.);
#8883=ORIENTED_EDGE('',*,*,#6514,.F.);
#8884=ORIENTED_EDGE('',*,*,#6518,.T.);
#8885=ORIENTED_EDGE('',*,*,#6670,.T.);
#8886=ORIENTED_EDGE('',*,*,#6667,.T.);
#8887=ORIENTED_EDGE('',*,*,#6664,.T.);
#8888=ORIENTED_EDGE('',*,*,#6509,.T.);
#8889=ORIENTED_EDGE('',*,*,#6505,.F.);
#8890=ORIENTED_EDGE('',*,*,#6707,.T.);
#8891=ORIENTED_EDGE('',*,*,#6500,.F.);
#8892=ORIENTED_EDGE('',*,*,#6504,.T.);
#8893=ORIENTED_EDGE('',*,*,#6662,.T.);
#8894=ORIENTED_EDGE('',*,*,#6659,.T.);
#8895=ORIENTED_EDGE('',*,*,#6656,.T.);
#8896=ORIENTED_EDGE('',*,*,#6495,.T.);
#8897=ORIENTED_EDGE('',*,*,#6491,.F.);
#8898=ORIENTED_EDGE('',*,*,#6708,.T.);
#8899=ORIENTED_EDGE('',*,*,#6486,.F.);
#8900=ORIENTED_EDGE('',*,*,#6490,.T.);
#8901=ORIENTED_EDGE('',*,*,#6654,.T.);
#8902=ORIENTED_EDGE('',*,*,#6651,.T.);
#8903=ORIENTED_EDGE('',*,*,#6648,.T.);
#8904=ORIENTED_EDGE('',*,*,#6481,.T.);
#8905=ORIENTED_EDGE('',*,*,#6477,.F.);
#8906=ORIENTED_EDGE('',*,*,#6709,.T.);
#8907=ORIENTED_EDGE('',*,*,#6472,.F.);
#8908=ORIENTED_EDGE('',*,*,#6476,.T.);
#8909=ORIENTED_EDGE('',*,*,#6646,.T.);
#8910=ORIENTED_EDGE('',*,*,#6643,.T.);
#8911=ORIENTED_EDGE('',*,*,#6640,.T.);
#8912=ORIENTED_EDGE('',*,*,#6467,.T.);
#8913=ORIENTED_EDGE('',*,*,#6463,.F.);
#8914=ORIENTED_EDGE('',*,*,#6710,.T.);
#8915=ORIENTED_EDGE('',*,*,#6458,.F.);
#8916=ORIENTED_EDGE('',*,*,#6462,.T.);
#8917=ORIENTED_EDGE('',*,*,#6638,.T.);
#8918=ORIENTED_EDGE('',*,*,#6635,.T.);
#8919=ORIENTED_EDGE('',*,*,#6632,.T.);
#8920=ORIENTED_EDGE('',*,*,#6453,.T.);
#8921=ORIENTED_EDGE('',*,*,#6449,.F.);
#8922=ORIENTED_EDGE('',*,*,#6711,.T.);
#8923=ORIENTED_EDGE('',*,*,#6444,.F.);
#8924=ORIENTED_EDGE('',*,*,#6448,.T.);
#8925=ORIENTED_EDGE('',*,*,#6630,.T.);
#8926=ORIENTED_EDGE('',*,*,#6627,.T.);
#8927=ORIENTED_EDGE('',*,*,#6624,.T.);
#8928=ORIENTED_EDGE('',*,*,#6439,.T.);
#8929=ORIENTED_EDGE('',*,*,#6435,.F.);
#8930=ORIENTED_EDGE('',*,*,#6712,.T.);
#8931=ORIENTED_EDGE('',*,*,#6430,.F.);
#8932=ORIENTED_EDGE('',*,*,#6434,.T.);
#8933=ORIENTED_EDGE('',*,*,#6622,.T.);
#8934=ORIENTED_EDGE('',*,*,#6619,.T.);
#8935=ORIENTED_EDGE('',*,*,#6616,.T.);
#8936=ORIENTED_EDGE('',*,*,#6425,.T.);
#8937=ORIENTED_EDGE('',*,*,#6421,.F.);
#8938=ORIENTED_EDGE('',*,*,#6713,.T.);
#8939=ORIENTED_EDGE('',*,*,#6416,.F.);
#8940=ORIENTED_EDGE('',*,*,#6420,.T.);
#8941=ORIENTED_EDGE('',*,*,#6614,.T.);
#8942=ORIENTED_EDGE('',*,*,#6611,.T.);
#8943=ORIENTED_EDGE('',*,*,#6608,.T.);
#8944=ORIENTED_EDGE('',*,*,#6411,.T.);
#8945=ORIENTED_EDGE('',*,*,#6407,.F.);
#8946=ORIENTED_EDGE('',*,*,#6714,.T.);
#8947=ORIENTED_EDGE('',*,*,#6402,.F.);
#8948=ORIENTED_EDGE('',*,*,#6406,.T.);
#8949=ORIENTED_EDGE('',*,*,#6606,.T.);
#8950=ORIENTED_EDGE('',*,*,#6603,.T.);
#8951=ORIENTED_EDGE('',*,*,#6600,.T.);
#8952=ORIENTED_EDGE('',*,*,#6397,.T.);
#8953=ORIENTED_EDGE('',*,*,#6393,.F.);
#8954=ORIENTED_EDGE('',*,*,#6715,.T.);
#8955=ORIENTED_EDGE('',*,*,#6388,.F.);
#8956=ORIENTED_EDGE('',*,*,#6392,.T.);
#8957=ORIENTED_EDGE('',*,*,#6598,.T.);
#8958=ORIENTED_EDGE('',*,*,#6595,.T.);
#8959=ORIENTED_EDGE('',*,*,#6592,.T.);
#8960=ORIENTED_EDGE('',*,*,#6383,.T.);
#8961=ORIENTED_EDGE('',*,*,#6379,.F.);
#8962=ORIENTED_EDGE('',*,*,#6716,.T.);
#8963=ORIENTED_EDGE('',*,*,#6374,.F.);
#8964=ORIENTED_EDGE('',*,*,#6378,.T.);
#8965=ORIENTED_EDGE('',*,*,#6590,.T.);
#8966=ORIENTED_EDGE('',*,*,#6587,.T.);
#8967=ORIENTED_EDGE('',*,*,#6584,.T.);
#8968=ORIENTED_EDGE('',*,*,#6369,.T.);
#8969=ORIENTED_EDGE('',*,*,#6365,.F.);
#8970=ORIENTED_EDGE('',*,*,#6717,.T.);
#8971=ORIENTED_EDGE('',*,*,#6360,.F.);
#8972=ORIENTED_EDGE('',*,*,#6364,.T.);
#8973=ORIENTED_EDGE('',*,*,#6582,.T.);
#8974=ORIENTED_EDGE('',*,*,#6579,.T.);
#8975=ORIENTED_EDGE('',*,*,#6576,.T.);
#8976=ORIENTED_EDGE('',*,*,#6355,.T.);
#8977=ORIENTED_EDGE('',*,*,#6351,.F.);
#8978=ORIENTED_EDGE('',*,*,#6718,.T.);
#8979=ORIENTED_EDGE('',*,*,#6346,.F.);
#8980=ORIENTED_EDGE('',*,*,#6350,.T.);
#8981=ORIENTED_EDGE('',*,*,#6574,.T.);
#8982=ORIENTED_EDGE('',*,*,#6571,.T.);
#8983=ORIENTED_EDGE('',*,*,#6568,.T.);
#8984=ORIENTED_EDGE('',*,*,#6341,.T.);
#8985=ORIENTED_EDGE('',*,*,#6337,.F.);
#8986=ORIENTED_EDGE('',*,*,#6719,.T.);
#8987=ORIENTED_EDGE('',*,*,#6332,.F.);
#8988=ORIENTED_EDGE('',*,*,#6336,.T.);
#8989=ORIENTED_EDGE('',*,*,#6566,.T.);
#8990=ORIENTED_EDGE('',*,*,#6563,.T.);
#8991=ORIENTED_EDGE('',*,*,#6560,.T.);
#8992=ORIENTED_EDGE('',*,*,#6327,.T.);
#8993=ORIENTED_EDGE('',*,*,#6323,.F.);
#8994=ORIENTED_EDGE('',*,*,#6720,.T.);
#8995=ORIENTED_EDGE('',*,*,#6318,.F.);
#8996=ORIENTED_EDGE('',*,*,#6322,.T.);
#8997=ORIENTED_EDGE('',*,*,#6558,.T.);
#8998=ORIENTED_EDGE('',*,*,#6555,.T.);
#8999=ORIENTED_EDGE('',*,*,#6552,.T.);
#9000=ORIENTED_EDGE('',*,*,#6313,.T.);
#9001=ORIENTED_EDGE('',*,*,#6309,.F.);
#9002=ORIENTED_EDGE('',*,*,#6721,.T.);
#9003=ORIENTED_EDGE('',*,*,#6304,.F.);
#9004=ORIENTED_EDGE('',*,*,#6308,.T.);
#9005=ORIENTED_EDGE('',*,*,#6550,.T.);
#9006=ORIENTED_EDGE('',*,*,#6547,.T.);
#9007=ORIENTED_EDGE('',*,*,#6544,.T.);
#9008=ORIENTED_EDGE('',*,*,#6299,.T.);
#9009=ORIENTED_EDGE('',*,*,#6295,.F.);
#9010=ORIENTED_EDGE('',*,*,#6722,.T.);
#9011=ORIENTED_EDGE('',*,*,#6290,.F.);
#9012=ORIENTED_EDGE('',*,*,#6294,.T.);
#9013=ORIENTED_EDGE('',*,*,#6542,.T.);
#9014=ORIENTED_EDGE('',*,*,#6539,.T.);
#9015=ORIENTED_EDGE('',*,*,#6536,.T.);
#9016=ORIENTED_EDGE('',*,*,#6285,.T.);
#9017=ORIENTED_EDGE('',*,*,#6281,.F.);
#9018=ORIENTED_EDGE('',*,*,#6723,.T.);
#9019=ORIENTED_EDGE('',*,*,#6276,.F.);
#9020=ORIENTED_EDGE('',*,*,#6280,.T.);
#9021=ORIENTED_EDGE('',*,*,#6534,.T.);
#9022=ORIENTED_EDGE('',*,*,#6531,.T.);
#9023=ORIENTED_EDGE('',*,*,#6528,.T.);
#9024=ORIENTED_EDGE('',*,*,#6271,.T.);
#9025=ORIENTED_EDGE('',*,*,#6267,.F.);
#9026=ORIENTED_EDGE('',*,*,#6724,.T.);
#9027=ORIENTED_EDGE('',*,*,#6262,.F.);
#9028=ORIENTED_EDGE('',*,*,#6266,.T.);
#9029=ORIENTED_EDGE('',*,*,#6526,.T.);
#9030=ORIENTED_EDGE('',*,*,#6523,.T.);
#9031=ORIENTED_EDGE('',*,*,#6520,.T.);
#9032=ORIENTED_EDGE('',*,*,#6257,.T.);
#9033=ORIENTED_EDGE('',*,*,#6253,.F.);
#9034=ORIENTED_EDGE('',*,*,#6247,.T.);
#9035=ORIENTED_EDGE('',*,*,#6515,.F.);
#9036=ORIENTED_EDGE('',*,*,#6706,.F.);
#9037=ORIENTED_EDGE('',*,*,#6725,.F.);
#9038=ORIENTED_EDGE('',*,*,#6688,.T.);
#9039=ORIENTED_EDGE('',*,*,#6501,.F.);
#9040=ORIENTED_EDGE('',*,*,#6707,.F.);
#9041=ORIENTED_EDGE('',*,*,#6508,.F.);
#9042=ORIENTED_EDGE('',*,*,#6687,.T.);
#9043=ORIENTED_EDGE('',*,*,#6487,.F.);
#9044=ORIENTED_EDGE('',*,*,#6708,.F.);
#9045=ORIENTED_EDGE('',*,*,#6494,.F.);
#9046=ORIENTED_EDGE('',*,*,#6686,.T.);
#9047=ORIENTED_EDGE('',*,*,#6473,.F.);
#9048=ORIENTED_EDGE('',*,*,#6709,.F.);
#9049=ORIENTED_EDGE('',*,*,#6480,.F.);
#9050=ORIENTED_EDGE('',*,*,#6685,.T.);
#9051=ORIENTED_EDGE('',*,*,#6459,.F.);
#9052=ORIENTED_EDGE('',*,*,#6710,.F.);
#9053=ORIENTED_EDGE('',*,*,#6466,.F.);
#9054=ORIENTED_EDGE('',*,*,#6684,.T.);
#9055=ORIENTED_EDGE('',*,*,#6445,.F.);
#9056=ORIENTED_EDGE('',*,*,#6711,.F.);
#9057=ORIENTED_EDGE('',*,*,#6452,.F.);
#9058=ORIENTED_EDGE('',*,*,#6683,.T.);
#9059=ORIENTED_EDGE('',*,*,#6431,.F.);
#9060=ORIENTED_EDGE('',*,*,#6712,.F.);
#9061=ORIENTED_EDGE('',*,*,#6438,.F.);
#9062=ORIENTED_EDGE('',*,*,#6682,.T.);
#9063=ORIENTED_EDGE('',*,*,#6417,.F.);
#9064=ORIENTED_EDGE('',*,*,#6713,.F.);
#9065=ORIENTED_EDGE('',*,*,#6424,.F.);
#9066=ORIENTED_EDGE('',*,*,#6681,.T.);
#9067=ORIENTED_EDGE('',*,*,#6403,.F.);
#9068=ORIENTED_EDGE('',*,*,#6714,.F.);
#9069=ORIENTED_EDGE('',*,*,#6410,.F.);
#9070=ORIENTED_EDGE('',*,*,#6680,.T.);
#9071=ORIENTED_EDGE('',*,*,#6389,.F.);
#9072=ORIENTED_EDGE('',*,*,#6715,.F.);
#9073=ORIENTED_EDGE('',*,*,#6396,.F.);
#9074=ORIENTED_EDGE('',*,*,#6679,.T.);
#9075=ORIENTED_EDGE('',*,*,#6375,.F.);
#9076=ORIENTED_EDGE('',*,*,#6716,.F.);
#9077=ORIENTED_EDGE('',*,*,#6382,.F.);
#9078=ORIENTED_EDGE('',*,*,#6678,.T.);
#9079=ORIENTED_EDGE('',*,*,#6361,.F.);
#9080=ORIENTED_EDGE('',*,*,#6717,.F.);
#9081=ORIENTED_EDGE('',*,*,#6368,.F.);
#9082=ORIENTED_EDGE('',*,*,#6677,.T.);
#9083=ORIENTED_EDGE('',*,*,#6347,.F.);
#9084=ORIENTED_EDGE('',*,*,#6718,.F.);
#9085=ORIENTED_EDGE('',*,*,#6354,.F.);
#9086=ORIENTED_EDGE('',*,*,#6676,.T.);
#9087=ORIENTED_EDGE('',*,*,#6333,.F.);
#9088=ORIENTED_EDGE('',*,*,#6719,.F.);
#9089=ORIENTED_EDGE('',*,*,#6340,.F.);
#9090=ORIENTED_EDGE('',*,*,#6675,.T.);
#9091=ORIENTED_EDGE('',*,*,#6319,.F.);
#9092=ORIENTED_EDGE('',*,*,#6720,.F.);
#9093=ORIENTED_EDGE('',*,*,#6326,.F.);
#9094=ORIENTED_EDGE('',*,*,#6674,.T.);
#9095=ORIENTED_EDGE('',*,*,#6305,.F.);
#9096=ORIENTED_EDGE('',*,*,#6721,.F.);
#9097=ORIENTED_EDGE('',*,*,#6312,.F.);
#9098=ORIENTED_EDGE('',*,*,#6673,.T.);
#9099=ORIENTED_EDGE('',*,*,#6291,.F.);
#9100=ORIENTED_EDGE('',*,*,#6722,.F.);
#9101=ORIENTED_EDGE('',*,*,#6298,.F.);
#9102=ORIENTED_EDGE('',*,*,#6672,.T.);
#9103=ORIENTED_EDGE('',*,*,#6277,.F.);
#9104=ORIENTED_EDGE('',*,*,#6723,.F.);
#9105=ORIENTED_EDGE('',*,*,#6284,.F.);
#9106=ORIENTED_EDGE('',*,*,#6671,.T.);
#9107=ORIENTED_EDGE('',*,*,#6263,.F.);
#9108=ORIENTED_EDGE('',*,*,#6724,.F.);
#9109=ORIENTED_EDGE('',*,*,#6270,.F.);
#9110=ORIENTED_EDGE('',*,*,#6697,.T.);
#9111=ORIENTED_EDGE('',*,*,#6705,.T.);
#9112=ORIENTED_EDGE('',*,*,#6726,.T.);
#9113=ORIENTED_EDGE('',*,*,#6689,.T.);
#9114=ORIENTED_EDGE('',*,*,#6725,.T.);
#9115=ORIENTED_EDGE('',*,*,#6726,.F.);
#9116=ORIENTED_EDGE('',*,*,#6704,.F.);
#9117=ORIENTED_EDGE('',*,*,#6727,.F.);
#9118=ORIENTED_EDGE('',*,*,#6690,.F.);
#9119=ORIENTED_EDGE('',*,*,#6695,.T.);
#9120=ORIENTED_EDGE('',*,*,#6728,.T.);
#9121=ORIENTED_EDGE('',*,*,#6699,.T.);
#9122=ORIENTED_EDGE('',*,*,#6729,.T.);
#9123=ORIENTED_EDGE('',*,*,#6728,.F.);
#9124=ORIENTED_EDGE('',*,*,#6694,.T.);
#9125=ORIENTED_EDGE('',*,*,#6730,.T.);
#9126=ORIENTED_EDGE('',*,*,#6700,.F.);
#9127=ORIENTED_EDGE('',*,*,#6691,.F.);
#9128=ORIENTED_EDGE('',*,*,#6727,.T.);
#9129=ORIENTED_EDGE('',*,*,#6703,.F.);
#9130=ORIENTED_EDGE('',*,*,#6731,.F.);
#9131=ORIENTED_EDGE('',*,*,#6692,.T.);
#9132=ORIENTED_EDGE('',*,*,#6731,.T.);
#9133=ORIENTED_EDGE('',*,*,#6702,.F.);
#9134=ORIENTED_EDGE('',*,*,#6732,.F.);
#9135=ORIENTED_EDGE('',*,*,#6693,.T.);
#9136=ORIENTED_EDGE('',*,*,#6732,.T.);
#9137=ORIENTED_EDGE('',*,*,#6701,.F.);
#9138=ORIENTED_EDGE('',*,*,#6730,.F.);
#9139=ORIENTED_EDGE('',*,*,#6256,.F.);
#9140=ORIENTED_EDGE('',*,*,#6696,.T.);
#9141=ORIENTED_EDGE('',*,*,#6729,.F.);
#9142=ORIENTED_EDGE('',*,*,#6698,.F.);
#9143=ORIENTED_EDGE('',*,*,#6733,.F.);
#9144=ORIENTED_EDGE('',*,*,#6734,.T.);
#9145=ORIENTED_EDGE('',*,*,#6735,.F.);
#9146=ORIENTED_EDGE('',*,*,#6734,.F.);
#9147=ORIENTED_EDGE('',*,*,#6736,.F.);
#9148=ORIENTED_EDGE('',*,*,#6737,.T.);
#9149=ORIENTED_EDGE('',*,*,#6738,.F.);
#9150=ORIENTED_EDGE('',*,*,#6737,.F.);
#9151=ORIENTED_EDGE('',*,*,#6735,.T.);
#9152=ORIENTED_EDGE('',*,*,#6736,.T.);
#9153=ORIENTED_EDGE('',*,*,#6739,.T.);
#9154=ORIENTED_EDGE('',*,*,#6740,.T.);
#9155=ORIENTED_EDGE('',*,*,#6741,.T.);
#9156=ORIENTED_EDGE('',*,*,#6742,.T.);
#9157=ORIENTED_EDGE('',*,*,#6740,.F.);
#9158=ORIENTED_EDGE('',*,*,#6743,.F.);
#9159=ORIENTED_EDGE('',*,*,#6744,.F.);
#9160=ORIENTED_EDGE('',*,*,#6745,.F.);
#9161=ORIENTED_EDGE('',*,*,#6746,.T.);
#9162=ORIENTED_EDGE('',*,*,#6747,.T.);
#9163=ORIENTED_EDGE('',*,*,#6748,.T.);
#9164=ORIENTED_EDGE('',*,*,#6749,.T.);
#9165=ORIENTED_EDGE('',*,*,#6747,.F.);
#9166=ORIENTED_EDGE('',*,*,#6750,.T.);
#9167=ORIENTED_EDGE('',*,*,#6751,.T.);
#9168=ORIENTED_EDGE('',*,*,#6752,.F.);
#9169=ORIENTED_EDGE('',*,*,#6753,.T.);
#9170=ORIENTED_EDGE('',*,*,#6754,.T.);
#9171=ORIENTED_EDGE('',*,*,#6755,.T.);
#9172=ORIENTED_EDGE('',*,*,#6756,.T.);
#9173=ORIENTED_EDGE('',*,*,#6754,.F.);
#9174=ORIENTED_EDGE('',*,*,#6757,.F.);
#9175=ORIENTED_EDGE('',*,*,#6758,.F.);
#9176=ORIENTED_EDGE('',*,*,#6759,.F.);
#9177=ORIENTED_EDGE('',*,*,#6760,.T.);
#9178=ORIENTED_EDGE('',*,*,#6761,.T.);
#9179=ORIENTED_EDGE('',*,*,#6762,.T.);
#9180=ORIENTED_EDGE('',*,*,#6763,.T.);
#9181=ORIENTED_EDGE('',*,*,#6761,.F.);
#9182=ORIENTED_EDGE('',*,*,#6764,.T.);
#9183=ORIENTED_EDGE('',*,*,#6765,.T.);
#9184=ORIENTED_EDGE('',*,*,#6766,.F.);
#9185=ORIENTED_EDGE('',*,*,#6767,.T.);
#9186=ORIENTED_EDGE('',*,*,#6768,.T.);
#9187=ORIENTED_EDGE('',*,*,#6769,.T.);
#9188=ORIENTED_EDGE('',*,*,#6770,.T.);
#9189=ORIENTED_EDGE('',*,*,#6768,.F.);
#9190=ORIENTED_EDGE('',*,*,#6771,.F.);
#9191=ORIENTED_EDGE('',*,*,#6772,.F.);
#9192=ORIENTED_EDGE('',*,*,#6773,.F.);
#9193=ORIENTED_EDGE('',*,*,#6774,.T.);
#9194=ORIENTED_EDGE('',*,*,#6775,.T.);
#9195=ORIENTED_EDGE('',*,*,#6776,.T.);
#9196=ORIENTED_EDGE('',*,*,#6777,.T.);
#9197=ORIENTED_EDGE('',*,*,#6775,.F.);
#9198=ORIENTED_EDGE('',*,*,#6778,.T.);
#9199=ORIENTED_EDGE('',*,*,#6779,.T.);
#9200=ORIENTED_EDGE('',*,*,#6780,.F.);
#9201=ORIENTED_EDGE('',*,*,#6781,.T.);
#9202=ORIENTED_EDGE('',*,*,#6782,.T.);
#9203=ORIENTED_EDGE('',*,*,#6783,.T.);
#9204=ORIENTED_EDGE('',*,*,#6784,.T.);
#9205=ORIENTED_EDGE('',*,*,#6782,.F.);
#9206=ORIENTED_EDGE('',*,*,#6785,.F.);
#9207=ORIENTED_EDGE('',*,*,#6786,.F.);
#9208=ORIENTED_EDGE('',*,*,#6787,.F.);
#9209=ORIENTED_EDGE('',*,*,#6788,.T.);
#9210=ORIENTED_EDGE('',*,*,#6789,.T.);
#9211=ORIENTED_EDGE('',*,*,#6790,.T.);
#9212=ORIENTED_EDGE('',*,*,#6791,.T.);
#9213=ORIENTED_EDGE('',*,*,#6789,.F.);
#9214=ORIENTED_EDGE('',*,*,#6792,.T.);
#9215=ORIENTED_EDGE('',*,*,#6793,.T.);
#9216=ORIENTED_EDGE('',*,*,#6794,.F.);
#9217=ORIENTED_EDGE('',*,*,#6795,.T.);
#9218=ORIENTED_EDGE('',*,*,#6796,.T.);
#9219=ORIENTED_EDGE('',*,*,#6797,.T.);
#9220=ORIENTED_EDGE('',*,*,#6798,.T.);
#9221=ORIENTED_EDGE('',*,*,#6796,.F.);
#9222=ORIENTED_EDGE('',*,*,#6799,.F.);
#9223=ORIENTED_EDGE('',*,*,#6800,.F.);
#9224=ORIENTED_EDGE('',*,*,#6801,.F.);
#9225=ORIENTED_EDGE('',*,*,#6802,.T.);
#9226=ORIENTED_EDGE('',*,*,#6803,.T.);
#9227=ORIENTED_EDGE('',*,*,#6804,.T.);
#9228=ORIENTED_EDGE('',*,*,#6805,.T.);
#9229=ORIENTED_EDGE('',*,*,#6803,.F.);
#9230=ORIENTED_EDGE('',*,*,#6806,.T.);
#9231=ORIENTED_EDGE('',*,*,#6807,.T.);
#9232=ORIENTED_EDGE('',*,*,#6808,.F.);
#9233=ORIENTED_EDGE('',*,*,#6809,.T.);
#9234=ORIENTED_EDGE('',*,*,#6810,.T.);
#9235=ORIENTED_EDGE('',*,*,#6811,.T.);
#9236=ORIENTED_EDGE('',*,*,#6812,.T.);
#9237=ORIENTED_EDGE('',*,*,#6810,.F.);
#9238=ORIENTED_EDGE('',*,*,#6813,.F.);
#9239=ORIENTED_EDGE('',*,*,#6814,.F.);
#9240=ORIENTED_EDGE('',*,*,#6815,.F.);
#9241=ORIENTED_EDGE('',*,*,#6816,.T.);
#9242=ORIENTED_EDGE('',*,*,#6817,.T.);
#9243=ORIENTED_EDGE('',*,*,#6818,.T.);
#9244=ORIENTED_EDGE('',*,*,#6819,.T.);
#9245=ORIENTED_EDGE('',*,*,#6817,.F.);
#9246=ORIENTED_EDGE('',*,*,#6820,.T.);
#9247=ORIENTED_EDGE('',*,*,#6821,.T.);
#9248=ORIENTED_EDGE('',*,*,#6822,.F.);
#9249=ORIENTED_EDGE('',*,*,#6823,.T.);
#9250=ORIENTED_EDGE('',*,*,#6824,.T.);
#9251=ORIENTED_EDGE('',*,*,#6825,.T.);
#9252=ORIENTED_EDGE('',*,*,#6826,.T.);
#9253=ORIENTED_EDGE('',*,*,#6824,.F.);
#9254=ORIENTED_EDGE('',*,*,#6827,.F.);
#9255=ORIENTED_EDGE('',*,*,#6828,.F.);
#9256=ORIENTED_EDGE('',*,*,#6829,.F.);
#9257=ORIENTED_EDGE('',*,*,#6830,.T.);
#9258=ORIENTED_EDGE('',*,*,#6831,.T.);
#9259=ORIENTED_EDGE('',*,*,#6832,.T.);
#9260=ORIENTED_EDGE('',*,*,#6833,.T.);
#9261=ORIENTED_EDGE('',*,*,#6831,.F.);
#9262=ORIENTED_EDGE('',*,*,#6834,.T.);
#9263=ORIENTED_EDGE('',*,*,#6835,.T.);
#9264=ORIENTED_EDGE('',*,*,#6836,.F.);
#9265=ORIENTED_EDGE('',*,*,#6837,.T.);
#9266=ORIENTED_EDGE('',*,*,#6838,.T.);
#9267=ORIENTED_EDGE('',*,*,#6839,.T.);
#9268=ORIENTED_EDGE('',*,*,#6840,.T.);
#9269=ORIENTED_EDGE('',*,*,#6838,.F.);
#9270=ORIENTED_EDGE('',*,*,#6841,.F.);
#9271=ORIENTED_EDGE('',*,*,#6842,.F.);
#9272=ORIENTED_EDGE('',*,*,#6843,.F.);
#9273=ORIENTED_EDGE('',*,*,#6844,.T.);
#9274=ORIENTED_EDGE('',*,*,#6845,.T.);
#9275=ORIENTED_EDGE('',*,*,#6846,.T.);
#9276=ORIENTED_EDGE('',*,*,#6847,.T.);
#9277=ORIENTED_EDGE('',*,*,#6845,.F.);
#9278=ORIENTED_EDGE('',*,*,#6848,.T.);
#9279=ORIENTED_EDGE('',*,*,#6849,.T.);
#9280=ORIENTED_EDGE('',*,*,#6850,.F.);
#9281=ORIENTED_EDGE('',*,*,#6851,.T.);
#9282=ORIENTED_EDGE('',*,*,#6852,.T.);
#9283=ORIENTED_EDGE('',*,*,#6853,.T.);
#9284=ORIENTED_EDGE('',*,*,#6854,.T.);
#9285=ORIENTED_EDGE('',*,*,#6852,.F.);
#9286=ORIENTED_EDGE('',*,*,#6855,.F.);
#9287=ORIENTED_EDGE('',*,*,#6856,.F.);
#9288=ORIENTED_EDGE('',*,*,#6857,.F.);
#9289=ORIENTED_EDGE('',*,*,#6858,.T.);
#9290=ORIENTED_EDGE('',*,*,#6859,.T.);
#9291=ORIENTED_EDGE('',*,*,#6860,.T.);
#9292=ORIENTED_EDGE('',*,*,#6861,.T.);
#9293=ORIENTED_EDGE('',*,*,#6859,.F.);
#9294=ORIENTED_EDGE('',*,*,#6862,.T.);
#9295=ORIENTED_EDGE('',*,*,#6863,.T.);
#9296=ORIENTED_EDGE('',*,*,#6864,.F.);
#9297=ORIENTED_EDGE('',*,*,#6865,.F.);
#9298=ORIENTED_EDGE('',*,*,#6744,.T.);
#9299=ORIENTED_EDGE('',*,*,#6866,.F.);
#9300=ORIENTED_EDGE('',*,*,#6867,.F.);
#9301=ORIENTED_EDGE('',*,*,#6868,.T.);
#9302=ORIENTED_EDGE('',*,*,#6867,.T.);
#9303=ORIENTED_EDGE('',*,*,#6869,.F.);
#9304=ORIENTED_EDGE('',*,*,#6870,.F.);
#9305=ORIENTED_EDGE('',*,*,#6871,.T.);
#9306=ORIENTED_EDGE('',*,*,#6870,.T.);
#9307=ORIENTED_EDGE('',*,*,#6872,.F.);
#9308=ORIENTED_EDGE('',*,*,#6751,.F.);
#9309=ORIENTED_EDGE('',*,*,#6873,.F.);
#9310=ORIENTED_EDGE('',*,*,#6758,.T.);
#9311=ORIENTED_EDGE('',*,*,#6874,.F.);
#9312=ORIENTED_EDGE('',*,*,#6875,.F.);
#9313=ORIENTED_EDGE('',*,*,#6876,.T.);
#9314=ORIENTED_EDGE('',*,*,#6875,.T.);
#9315=ORIENTED_EDGE('',*,*,#6877,.F.);
#9316=ORIENTED_EDGE('',*,*,#6878,.F.);
#9317=ORIENTED_EDGE('',*,*,#6879,.T.);
#9318=ORIENTED_EDGE('',*,*,#6878,.T.);
#9319=ORIENTED_EDGE('',*,*,#6880,.F.);
#9320=ORIENTED_EDGE('',*,*,#6765,.F.);
#9321=ORIENTED_EDGE('',*,*,#6881,.F.);
#9322=ORIENTED_EDGE('',*,*,#6772,.T.);
#9323=ORIENTED_EDGE('',*,*,#6882,.F.);
#9324=ORIENTED_EDGE('',*,*,#6883,.F.);
#9325=ORIENTED_EDGE('',*,*,#6884,.T.);
#9326=ORIENTED_EDGE('',*,*,#6883,.T.);
#9327=ORIENTED_EDGE('',*,*,#6885,.F.);
#9328=ORIENTED_EDGE('',*,*,#6886,.F.);
#9329=ORIENTED_EDGE('',*,*,#6887,.T.);
#9330=ORIENTED_EDGE('',*,*,#6886,.T.);
#9331=ORIENTED_EDGE('',*,*,#6888,.F.);
#9332=ORIENTED_EDGE('',*,*,#6779,.F.);
#9333=ORIENTED_EDGE('',*,*,#6889,.F.);
#9334=ORIENTED_EDGE('',*,*,#6786,.T.);
#9335=ORIENTED_EDGE('',*,*,#6890,.F.);
#9336=ORIENTED_EDGE('',*,*,#6891,.F.);
#9337=ORIENTED_EDGE('',*,*,#6892,.T.);
#9338=ORIENTED_EDGE('',*,*,#6891,.T.);
#9339=ORIENTED_EDGE('',*,*,#6893,.F.);
#9340=ORIENTED_EDGE('',*,*,#6894,.F.);
#9341=ORIENTED_EDGE('',*,*,#6895,.T.);
#9342=ORIENTED_EDGE('',*,*,#6894,.T.);
#9343=ORIENTED_EDGE('',*,*,#6896,.F.);
#9344=ORIENTED_EDGE('',*,*,#6793,.F.);
#9345=ORIENTED_EDGE('',*,*,#6897,.F.);
#9346=ORIENTED_EDGE('',*,*,#6800,.T.);
#9347=ORIENTED_EDGE('',*,*,#6898,.F.);
#9348=ORIENTED_EDGE('',*,*,#6899,.F.);
#9349=ORIENTED_EDGE('',*,*,#6900,.T.);
#9350=ORIENTED_EDGE('',*,*,#6899,.T.);
#9351=ORIENTED_EDGE('',*,*,#6901,.F.);
#9352=ORIENTED_EDGE('',*,*,#6902,.F.);
#9353=ORIENTED_EDGE('',*,*,#6903,.T.);
#9354=ORIENTED_EDGE('',*,*,#6902,.T.);
#9355=ORIENTED_EDGE('',*,*,#6904,.F.);
#9356=ORIENTED_EDGE('',*,*,#6807,.F.);
#9357=ORIENTED_EDGE('',*,*,#6905,.F.);
#9358=ORIENTED_EDGE('',*,*,#6814,.T.);
#9359=ORIENTED_EDGE('',*,*,#6906,.F.);
#9360=ORIENTED_EDGE('',*,*,#6907,.F.);
#9361=ORIENTED_EDGE('',*,*,#6908,.T.);
#9362=ORIENTED_EDGE('',*,*,#6907,.T.);
#9363=ORIENTED_EDGE('',*,*,#6909,.F.);
#9364=ORIENTED_EDGE('',*,*,#6910,.F.);
#9365=ORIENTED_EDGE('',*,*,#6911,.T.);
#9366=ORIENTED_EDGE('',*,*,#6910,.T.);
#9367=ORIENTED_EDGE('',*,*,#6912,.F.);
#9368=ORIENTED_EDGE('',*,*,#6821,.F.);
#9369=ORIENTED_EDGE('',*,*,#6913,.F.);
#9370=ORIENTED_EDGE('',*,*,#6828,.T.);
#9371=ORIENTED_EDGE('',*,*,#6914,.F.);
#9372=ORIENTED_EDGE('',*,*,#6915,.F.);
#9373=ORIENTED_EDGE('',*,*,#6916,.T.);
#9374=ORIENTED_EDGE('',*,*,#6915,.T.);
#9375=ORIENTED_EDGE('',*,*,#6917,.F.);
#9376=ORIENTED_EDGE('',*,*,#6918,.F.);
#9377=ORIENTED_EDGE('',*,*,#6919,.T.);
#9378=ORIENTED_EDGE('',*,*,#6918,.T.);
#9379=ORIENTED_EDGE('',*,*,#6920,.F.);
#9380=ORIENTED_EDGE('',*,*,#6835,.F.);
#9381=ORIENTED_EDGE('',*,*,#6921,.F.);
#9382=ORIENTED_EDGE('',*,*,#6842,.T.);
#9383=ORIENTED_EDGE('',*,*,#6922,.F.);
#9384=ORIENTED_EDGE('',*,*,#6923,.F.);
#9385=ORIENTED_EDGE('',*,*,#6924,.T.);
#9386=ORIENTED_EDGE('',*,*,#6923,.T.);
#9387=ORIENTED_EDGE('',*,*,#6925,.F.);
#9388=ORIENTED_EDGE('',*,*,#6926,.F.);
#9389=ORIENTED_EDGE('',*,*,#6927,.T.);
#9390=ORIENTED_EDGE('',*,*,#6926,.T.);
#9391=ORIENTED_EDGE('',*,*,#6928,.F.);
#9392=ORIENTED_EDGE('',*,*,#6849,.F.);
#9393=ORIENTED_EDGE('',*,*,#6929,.F.);
#9394=ORIENTED_EDGE('',*,*,#6856,.T.);
#9395=ORIENTED_EDGE('',*,*,#6930,.F.);
#9396=ORIENTED_EDGE('',*,*,#6931,.F.);
#9397=ORIENTED_EDGE('',*,*,#6932,.T.);
#9398=ORIENTED_EDGE('',*,*,#6931,.T.);
#9399=ORIENTED_EDGE('',*,*,#6933,.F.);
#9400=ORIENTED_EDGE('',*,*,#6934,.F.);
#9401=ORIENTED_EDGE('',*,*,#6935,.T.);
#9402=ORIENTED_EDGE('',*,*,#6934,.T.);
#9403=ORIENTED_EDGE('',*,*,#6936,.F.);
#9404=ORIENTED_EDGE('',*,*,#6863,.F.);
#9405=ORIENTED_EDGE('',*,*,#6755,.F.);
#9406=ORIENTED_EDGE('',*,*,#6759,.T.);
#9407=ORIENTED_EDGE('',*,*,#6873,.T.);
#9408=ORIENTED_EDGE('',*,*,#6876,.F.);
#9409=ORIENTED_EDGE('',*,*,#6879,.F.);
#9410=ORIENTED_EDGE('',*,*,#6764,.F.);
#9411=ORIENTED_EDGE('',*,*,#6760,.F.);
#9412=ORIENTED_EDGE('',*,*,#6937,.F.);
#9413=ORIENTED_EDGE('',*,*,#6769,.F.);
#9414=ORIENTED_EDGE('',*,*,#6773,.T.);
#9415=ORIENTED_EDGE('',*,*,#6881,.T.);
#9416=ORIENTED_EDGE('',*,*,#6884,.F.);
#9417=ORIENTED_EDGE('',*,*,#6887,.F.);
#9418=ORIENTED_EDGE('',*,*,#6778,.F.);
#9419=ORIENTED_EDGE('',*,*,#6774,.F.);
#9420=ORIENTED_EDGE('',*,*,#6938,.F.);
#9421=ORIENTED_EDGE('',*,*,#6783,.F.);
#9422=ORIENTED_EDGE('',*,*,#6787,.T.);
#9423=ORIENTED_EDGE('',*,*,#6889,.T.);
#9424=ORIENTED_EDGE('',*,*,#6892,.F.);
#9425=ORIENTED_EDGE('',*,*,#6895,.F.);
#9426=ORIENTED_EDGE('',*,*,#6792,.F.);
#9427=ORIENTED_EDGE('',*,*,#6788,.F.);
#9428=ORIENTED_EDGE('',*,*,#6939,.F.);
#9429=ORIENTED_EDGE('',*,*,#6797,.F.);
#9430=ORIENTED_EDGE('',*,*,#6801,.T.);
#9431=ORIENTED_EDGE('',*,*,#6897,.T.);
#9432=ORIENTED_EDGE('',*,*,#6900,.F.);
#9433=ORIENTED_EDGE('',*,*,#6903,.F.);
#9434=ORIENTED_EDGE('',*,*,#6806,.F.);
#9435=ORIENTED_EDGE('',*,*,#6802,.F.);
#9436=ORIENTED_EDGE('',*,*,#6940,.F.);
#9437=ORIENTED_EDGE('',*,*,#6811,.F.);
#9438=ORIENTED_EDGE('',*,*,#6815,.T.);
#9439=ORIENTED_EDGE('',*,*,#6905,.T.);
#9440=ORIENTED_EDGE('',*,*,#6908,.F.);
#9441=ORIENTED_EDGE('',*,*,#6911,.F.);
#9442=ORIENTED_EDGE('',*,*,#6820,.F.);
#9443=ORIENTED_EDGE('',*,*,#6816,.F.);
#9444=ORIENTED_EDGE('',*,*,#6941,.F.);
#9445=ORIENTED_EDGE('',*,*,#6825,.F.);
#9446=ORIENTED_EDGE('',*,*,#6829,.T.);
#9447=ORIENTED_EDGE('',*,*,#6913,.T.);
#9448=ORIENTED_EDGE('',*,*,#6916,.F.);
#9449=ORIENTED_EDGE('',*,*,#6919,.F.);
#9450=ORIENTED_EDGE('',*,*,#6834,.F.);
#9451=ORIENTED_EDGE('',*,*,#6830,.F.);
#9452=ORIENTED_EDGE('',*,*,#6942,.F.);
#9453=ORIENTED_EDGE('',*,*,#6839,.F.);
#9454=ORIENTED_EDGE('',*,*,#6843,.T.);
#9455=ORIENTED_EDGE('',*,*,#6921,.T.);
#9456=ORIENTED_EDGE('',*,*,#6924,.F.);
#9457=ORIENTED_EDGE('',*,*,#6927,.F.);
#9458=ORIENTED_EDGE('',*,*,#6848,.F.);
#9459=ORIENTED_EDGE('',*,*,#6844,.F.);
#9460=ORIENTED_EDGE('',*,*,#6943,.F.);
#9461=ORIENTED_EDGE('',*,*,#6853,.F.);
#9462=ORIENTED_EDGE('',*,*,#6857,.T.);
#9463=ORIENTED_EDGE('',*,*,#6929,.T.);
#9464=ORIENTED_EDGE('',*,*,#6932,.F.);
#9465=ORIENTED_EDGE('',*,*,#6935,.F.);
#9466=ORIENTED_EDGE('',*,*,#6862,.F.);
#9467=ORIENTED_EDGE('',*,*,#6858,.F.);
#9468=ORIENTED_EDGE('',*,*,#6944,.F.);
#9469=ORIENTED_EDGE('',*,*,#6945,.F.);
#9470=ORIENTED_EDGE('',*,*,#6946,.T.);
#9471=ORIENTED_EDGE('',*,*,#6947,.T.);
#9472=ORIENTED_EDGE('',*,*,#6948,.F.);
#9473=ORIENTED_EDGE('',*,*,#6949,.F.);
#9474=ORIENTED_EDGE('',*,*,#6950,.F.);
#9475=ORIENTED_EDGE('',*,*,#6951,.F.);
#9476=ORIENTED_EDGE('',*,*,#6952,.F.);
#9477=ORIENTED_EDGE('',*,*,#6741,.F.);
#9478=ORIENTED_EDGE('',*,*,#6745,.T.);
#9479=ORIENTED_EDGE('',*,*,#6865,.T.);
#9480=ORIENTED_EDGE('',*,*,#6868,.F.);
#9481=ORIENTED_EDGE('',*,*,#6871,.F.);
#9482=ORIENTED_EDGE('',*,*,#6750,.F.);
#9483=ORIENTED_EDGE('',*,*,#6746,.F.);
#9484=ORIENTED_EDGE('',*,*,#6953,.F.);
#9485=ORIENTED_EDGE('',*,*,#6738,.T.);
#9486=ORIENTED_EDGE('',*,*,#6954,.T.);
#9487=ORIENTED_EDGE('',*,*,#6955,.F.);
#9488=ORIENTED_EDGE('',*,*,#6956,.T.);
#9489=ORIENTED_EDGE('',*,*,#6957,.T.);
#9490=ORIENTED_EDGE('',*,*,#6958,.T.);
#9491=ORIENTED_EDGE('',*,*,#6959,.T.);
#9492=ORIENTED_EDGE('',*,*,#6960,.T.);
#9493=ORIENTED_EDGE('',*,*,#6961,.F.);
#9494=ORIENTED_EDGE('',*,*,#6962,.T.);
#9495=ORIENTED_EDGE('',*,*,#6860,.F.);
#9496=ORIENTED_EDGE('',*,*,#6864,.T.);
#9497=ORIENTED_EDGE('',*,*,#6936,.T.);
#9498=ORIENTED_EDGE('',*,*,#6933,.T.);
#9499=ORIENTED_EDGE('',*,*,#6930,.T.);
#9500=ORIENTED_EDGE('',*,*,#6855,.T.);
#9501=ORIENTED_EDGE('',*,*,#6851,.F.);
#9502=ORIENTED_EDGE('',*,*,#6963,.T.);
#9503=ORIENTED_EDGE('',*,*,#6846,.F.);
#9504=ORIENTED_EDGE('',*,*,#6850,.T.);
#9505=ORIENTED_EDGE('',*,*,#6928,.T.);
#9506=ORIENTED_EDGE('',*,*,#6925,.T.);
#9507=ORIENTED_EDGE('',*,*,#6922,.T.);
#9508=ORIENTED_EDGE('',*,*,#6841,.T.);
#9509=ORIENTED_EDGE('',*,*,#6837,.F.);
#9510=ORIENTED_EDGE('',*,*,#6964,.T.);
#9511=ORIENTED_EDGE('',*,*,#6832,.F.);
#9512=ORIENTED_EDGE('',*,*,#6836,.T.);
#9513=ORIENTED_EDGE('',*,*,#6920,.T.);
#9514=ORIENTED_EDGE('',*,*,#6917,.T.);
#9515=ORIENTED_EDGE('',*,*,#6914,.T.);
#9516=ORIENTED_EDGE('',*,*,#6827,.T.);
#9517=ORIENTED_EDGE('',*,*,#6823,.F.);
#9518=ORIENTED_EDGE('',*,*,#6965,.T.);
#9519=ORIENTED_EDGE('',*,*,#6818,.F.);
#9520=ORIENTED_EDGE('',*,*,#6822,.T.);
#9521=ORIENTED_EDGE('',*,*,#6912,.T.);
#9522=ORIENTED_EDGE('',*,*,#6909,.T.);
#9523=ORIENTED_EDGE('',*,*,#6906,.T.);
#9524=ORIENTED_EDGE('',*,*,#6813,.T.);
#9525=ORIENTED_EDGE('',*,*,#6809,.F.);
#9526=ORIENTED_EDGE('',*,*,#6966,.T.);
#9527=ORIENTED_EDGE('',*,*,#6804,.F.);
#9528=ORIENTED_EDGE('',*,*,#6808,.T.);
#9529=ORIENTED_EDGE('',*,*,#6904,.T.);
#9530=ORIENTED_EDGE('',*,*,#6901,.T.);
#9531=ORIENTED_EDGE('',*,*,#6898,.T.);
#9532=ORIENTED_EDGE('',*,*,#6799,.T.);
#9533=ORIENTED_EDGE('',*,*,#6795,.F.);
#9534=ORIENTED_EDGE('',*,*,#6967,.T.);
#9535=ORIENTED_EDGE('',*,*,#6790,.F.);
#9536=ORIENTED_EDGE('',*,*,#6794,.T.);
#9537=ORIENTED_EDGE('',*,*,#6896,.T.);
#9538=ORIENTED_EDGE('',*,*,#6893,.T.);
#9539=ORIENTED_EDGE('',*,*,#6890,.T.);
#9540=ORIENTED_EDGE('',*,*,#6785,.T.);
#9541=ORIENTED_EDGE('',*,*,#6781,.F.);
#9542=ORIENTED_EDGE('',*,*,#6968,.T.);
#9543=ORIENTED_EDGE('',*,*,#6776,.F.);
#9544=ORIENTED_EDGE('',*,*,#6780,.T.);
#9545=ORIENTED_EDGE('',*,*,#6888,.T.);
#9546=ORIENTED_EDGE('',*,*,#6885,.T.);
#9547=ORIENTED_EDGE('',*,*,#6882,.T.);
#9548=ORIENTED_EDGE('',*,*,#6771,.T.);
#9549=ORIENTED_EDGE('',*,*,#6767,.F.);
#9550=ORIENTED_EDGE('',*,*,#6969,.T.);
#9551=ORIENTED_EDGE('',*,*,#6762,.F.);
#9552=ORIENTED_EDGE('',*,*,#6766,.T.);
#9553=ORIENTED_EDGE('',*,*,#6880,.T.);
#9554=ORIENTED_EDGE('',*,*,#6877,.T.);
#9555=ORIENTED_EDGE('',*,*,#6874,.T.);
#9556=ORIENTED_EDGE('',*,*,#6757,.T.);
#9557=ORIENTED_EDGE('',*,*,#6753,.F.);
#9558=ORIENTED_EDGE('',*,*,#6970,.T.);
#9559=ORIENTED_EDGE('',*,*,#6748,.F.);
#9560=ORIENTED_EDGE('',*,*,#6752,.T.);
#9561=ORIENTED_EDGE('',*,*,#6872,.T.);
#9562=ORIENTED_EDGE('',*,*,#6869,.T.);
#9563=ORIENTED_EDGE('',*,*,#6866,.T.);
#9564=ORIENTED_EDGE('',*,*,#6743,.T.);
#9565=ORIENTED_EDGE('',*,*,#6739,.F.);
#9566=ORIENTED_EDGE('',*,*,#6733,.T.);
#9567=ORIENTED_EDGE('',*,*,#6861,.F.);
#9568=ORIENTED_EDGE('',*,*,#6962,.F.);
#9569=ORIENTED_EDGE('',*,*,#6971,.F.);
#9570=ORIENTED_EDGE('',*,*,#6944,.T.);
#9571=ORIENTED_EDGE('',*,*,#6847,.F.);
#9572=ORIENTED_EDGE('',*,*,#6963,.F.);
#9573=ORIENTED_EDGE('',*,*,#6854,.F.);
#9574=ORIENTED_EDGE('',*,*,#6943,.T.);
#9575=ORIENTED_EDGE('',*,*,#6833,.F.);
#9576=ORIENTED_EDGE('',*,*,#6964,.F.);
#9577=ORIENTED_EDGE('',*,*,#6840,.F.);
#9578=ORIENTED_EDGE('',*,*,#6942,.T.);
#9579=ORIENTED_EDGE('',*,*,#6819,.F.);
#9580=ORIENTED_EDGE('',*,*,#6965,.F.);
#9581=ORIENTED_EDGE('',*,*,#6826,.F.);
#9582=ORIENTED_EDGE('',*,*,#6941,.T.);
#9583=ORIENTED_EDGE('',*,*,#6805,.F.);
#9584=ORIENTED_EDGE('',*,*,#6966,.F.);
#9585=ORIENTED_EDGE('',*,*,#6812,.F.);
#9586=ORIENTED_EDGE('',*,*,#6940,.T.);
#9587=ORIENTED_EDGE('',*,*,#6791,.F.);
#9588=ORIENTED_EDGE('',*,*,#6967,.F.);
#9589=ORIENTED_EDGE('',*,*,#6798,.F.);
#9590=ORIENTED_EDGE('',*,*,#6939,.T.);
#9591=ORIENTED_EDGE('',*,*,#6777,.F.);
#9592=ORIENTED_EDGE('',*,*,#6968,.F.);
#9593=ORIENTED_EDGE('',*,*,#6784,.F.);
#9594=ORIENTED_EDGE('',*,*,#6938,.T.);
#9595=ORIENTED_EDGE('',*,*,#6763,.F.);
#9596=ORIENTED_EDGE('',*,*,#6969,.F.);
#9597=ORIENTED_EDGE('',*,*,#6770,.F.);
#9598=ORIENTED_EDGE('',*,*,#6937,.T.);
#9599=ORIENTED_EDGE('',*,*,#6749,.F.);
#9600=ORIENTED_EDGE('',*,*,#6970,.F.);
#9601=ORIENTED_EDGE('',*,*,#6756,.F.);
#9602=ORIENTED_EDGE('',*,*,#6953,.T.);
#9603=ORIENTED_EDGE('',*,*,#6961,.T.);
#9604=ORIENTED_EDGE('',*,*,#6972,.T.);
#9605=ORIENTED_EDGE('',*,*,#6945,.T.);
#9606=ORIENTED_EDGE('',*,*,#6971,.T.);
#9607=ORIENTED_EDGE('',*,*,#6972,.F.);
#9608=ORIENTED_EDGE('',*,*,#6960,.F.);
#9609=ORIENTED_EDGE('',*,*,#6973,.F.);
#9610=ORIENTED_EDGE('',*,*,#6946,.F.);
#9611=ORIENTED_EDGE('',*,*,#6951,.T.);
#9612=ORIENTED_EDGE('',*,*,#6974,.T.);
#9613=ORIENTED_EDGE('',*,*,#6955,.T.);
#9614=ORIENTED_EDGE('',*,*,#6975,.T.);
#9615=ORIENTED_EDGE('',*,*,#6974,.F.);
#9616=ORIENTED_EDGE('',*,*,#6950,.T.);
#9617=ORIENTED_EDGE('',*,*,#6976,.T.);
#9618=ORIENTED_EDGE('',*,*,#6956,.F.);
#9619=ORIENTED_EDGE('',*,*,#6947,.F.);
#9620=ORIENTED_EDGE('',*,*,#6973,.T.);
#9621=ORIENTED_EDGE('',*,*,#6959,.F.);
#9622=ORIENTED_EDGE('',*,*,#6977,.F.);
#9623=ORIENTED_EDGE('',*,*,#6948,.T.);
#9624=ORIENTED_EDGE('',*,*,#6977,.T.);
#9625=ORIENTED_EDGE('',*,*,#6958,.F.);
#9626=ORIENTED_EDGE('',*,*,#6978,.F.);
#9627=ORIENTED_EDGE('',*,*,#6949,.T.);
#9628=ORIENTED_EDGE('',*,*,#6978,.T.);
#9629=ORIENTED_EDGE('',*,*,#6957,.F.);
#9630=ORIENTED_EDGE('',*,*,#6976,.F.);
#9631=ORIENTED_EDGE('',*,*,#6742,.F.);
#9632=ORIENTED_EDGE('',*,*,#6952,.T.);
#9633=ORIENTED_EDGE('',*,*,#6975,.F.);
#9634=ORIENTED_EDGE('',*,*,#6954,.F.);
#9635=ORIENTED_EDGE('',*,*,#6979,.F.);
#9636=ORIENTED_EDGE('',*,*,#6980,.T.);
#9637=ORIENTED_EDGE('',*,*,#6981,.T.);
#9638=ORIENTED_EDGE('',*,*,#6980,.F.);
#9639=ORIENTED_EDGE('',*,*,#6982,.F.);
#9640=ORIENTED_EDGE('',*,*,#6983,.F.);
#9641=ORIENTED_EDGE('',*,*,#6984,.T.);
#9642=ORIENTED_EDGE('',*,*,#6985,.F.);
#9643=ORIENTED_EDGE('',*,*,#6986,.F.);
#9644=ORIENTED_EDGE('',*,*,#6984,.F.);
#9645=ORIENTED_EDGE('',*,*,#6987,.F.);
#9646=ORIENTED_EDGE('',*,*,#6988,.F.);
#9647=ORIENTED_EDGE('',*,*,#6989,.T.);
#9648=ORIENTED_EDGE('',*,*,#6990,.F.);
#9649=ORIENTED_EDGE('',*,*,#6989,.F.);
#9650=ORIENTED_EDGE('',*,*,#6982,.T.);
#9651=ORIENTED_EDGE('',*,*,#6983,.T.);
#9652=ORIENTED_EDGE('',*,*,#6991,.T.);
#9653=ORIENTED_EDGE('',*,*,#6992,.T.);
#9654=ORIENTED_EDGE('',*,*,#6991,.F.);
#9655=ORIENTED_EDGE('',*,*,#6987,.T.);
#9656=ORIENTED_EDGE('',*,*,#6988,.T.);
#9657=ORIENTED_EDGE('',*,*,#6993,.T.);
#9658=ORIENTED_EDGE('',*,*,#6985,.T.);
#9659=ORIENTED_EDGE('',*,*,#6986,.T.);
#9660=ORIENTED_EDGE('',*,*,#6993,.F.);
#9661=ORIENTED_EDGE('',*,*,#6990,.T.);
#9662=ORIENTED_EDGE('',*,*,#6994,.T.);
#9663=ORIENTED_EDGE('',*,*,#6995,.F.);
#9664=ORIENTED_EDGE('',*,*,#6994,.F.);
#9665=ORIENTED_EDGE('',*,*,#6981,.F.);
#9666=ORIENTED_EDGE('',*,*,#6996,.T.);
#9667=ORIENTED_EDGE('',*,*,#6997,.T.);
#9668=ORIENTED_EDGE('',*,*,#6996,.F.);
#9669=ORIENTED_EDGE('',*,*,#6998,.F.);
#9670=ORIENTED_EDGE('',*,*,#6999,.T.);
#9671=ORIENTED_EDGE('',*,*,#6979,.T.);
#9672=ORIENTED_EDGE('',*,*,#6999,.F.);
#9673=ORIENTED_EDGE('',*,*,#6998,.T.);
#9674=ORIENTED_EDGE('',*,*,#6992,.F.);
#9675=ORIENTED_EDGE('',*,*,#6997,.F.);
#9676=ORIENTED_EDGE('',*,*,#6995,.T.);
#9677=ORIENTED_EDGE('',*,*,#7000,.T.);
#9678=ORIENTED_EDGE('',*,*,#7000,.F.);
#9679=ORIENTED_EDGE('',*,*,#7001,.T.);
#9680=ORIENTED_EDGE('',*,*,#7001,.F.);
#9681=ORIENTED_EDGE('',*,*,#7002,.T.);
#9682=ORIENTED_EDGE('',*,*,#7002,.F.);
#9683=ORIENTED_EDGE('',*,*,#7003,.T.);
#9684=ORIENTED_EDGE('',*,*,#7003,.F.);
#9685=ORIENTED_EDGE('',*,*,#7004,.T.);
#9686=ORIENTED_EDGE('',*,*,#7004,.F.);
#9687=ORIENTED_EDGE('',*,*,#7005,.T.);
#9688=ORIENTED_EDGE('',*,*,#7005,.F.);
#9689=ORIENTED_EDGE('',*,*,#7006,.T.);
#9690=ORIENTED_EDGE('',*,*,#7006,.F.);
#9691=ORIENTED_EDGE('',*,*,#7007,.F.);
#9692=ORIENTED_EDGE('',*,*,#7008,.T.);
#9693=ORIENTED_EDGE('',*,*,#7009,.F.);
#9694=ORIENTED_EDGE('',*,*,#7010,.F.);
#9695=ORIENTED_EDGE('',*,*,#7008,.F.);
#9696=ORIENTED_EDGE('',*,*,#7011,.F.);
#9697=ORIENTED_EDGE('',*,*,#7012,.T.);
#9698=ORIENTED_EDGE('',*,*,#7013,.F.);
#9699=ORIENTED_EDGE('',*,*,#7012,.F.);
#9700=ORIENTED_EDGE('',*,*,#7014,.F.);
#9701=ORIENTED_EDGE('',*,*,#7015,.T.);
#9702=ORIENTED_EDGE('',*,*,#7016,.F.);
#9703=ORIENTED_EDGE('',*,*,#7015,.F.);
#9704=ORIENTED_EDGE('',*,*,#7017,.F.);
#9705=ORIENTED_EDGE('',*,*,#7018,.F.);
#9706=ORIENTED_EDGE('',*,*,#7019,.T.);
#9707=ORIENTED_EDGE('',*,*,#7020,.F.);
#9708=ORIENTED_EDGE('',*,*,#7019,.F.);
#9709=ORIENTED_EDGE('',*,*,#7021,.F.);
#9710=ORIENTED_EDGE('',*,*,#7022,.T.);
#9711=ORIENTED_EDGE('',*,*,#7023,.T.);
#9712=ORIENTED_EDGE('',*,*,#7022,.F.);
#9713=ORIENTED_EDGE('',*,*,#7024,.F.);
#9714=ORIENTED_EDGE('',*,*,#7025,.T.);
#9715=ORIENTED_EDGE('',*,*,#7009,.T.);
#9716=ORIENTED_EDGE('',*,*,#7010,.T.);
#9717=ORIENTED_EDGE('',*,*,#7025,.F.);
#9718=ORIENTED_EDGE('',*,*,#7017,.T.);
#9719=ORIENTED_EDGE('',*,*,#7018,.T.);
#9720=ORIENTED_EDGE('',*,*,#7026,.T.);
#9721=ORIENTED_EDGE('',*,*,#7027,.T.);
#9722=ORIENTED_EDGE('',*,*,#7026,.F.);
#9723=ORIENTED_EDGE('',*,*,#7027,.F.);
#9724=ORIENTED_EDGE('',*,*,#7028,.T.);
#9725=ORIENTED_EDGE('',*,*,#7029,.T.);
#9726=ORIENTED_EDGE('',*,*,#7028,.F.);
#9727=ORIENTED_EDGE('',*,*,#7029,.F.);
#9728=ORIENTED_EDGE('',*,*,#7030,.T.);
#9729=ORIENTED_EDGE('',*,*,#7011,.T.);
#9730=ORIENTED_EDGE('',*,*,#7030,.F.);
#9731=ORIENTED_EDGE('',*,*,#7016,.T.);
#9732=ORIENTED_EDGE('',*,*,#7031,.T.);
#9733=ORIENTED_EDGE('',*,*,#7032,.T.);
#9734=ORIENTED_EDGE('',*,*,#7031,.F.);
#9735=ORIENTED_EDGE('',*,*,#7033,.F.);
#9736=ORIENTED_EDGE('',*,*,#7034,.T.);
#9737=ORIENTED_EDGE('',*,*,#7035,.T.);
#9738=ORIENTED_EDGE('',*,*,#7034,.F.);
#9739=ORIENTED_EDGE('',*,*,#7036,.F.);
#9740=ORIENTED_EDGE('',*,*,#7037,.T.);
#9741=ORIENTED_EDGE('',*,*,#7038,.T.);
#9742=ORIENTED_EDGE('',*,*,#7037,.F.);
#9743=ORIENTED_EDGE('',*,*,#7039,.T.);
#9744=ORIENTED_EDGE('',*,*,#7040,.T.);
#9745=ORIENTED_EDGE('',*,*,#7041,.F.);
#9746=ORIENTED_EDGE('',*,*,#7040,.F.);
#9747=ORIENTED_EDGE('',*,*,#7042,.T.);
#9748=ORIENTED_EDGE('',*,*,#7039,.F.);
#9749=ORIENTED_EDGE('',*,*,#7043,.T.);
#9750=ORIENTED_EDGE('',*,*,#7036,.T.);
#9751=ORIENTED_EDGE('',*,*,#7043,.F.);
#9752=ORIENTED_EDGE('',*,*,#7042,.F.);
#9753=ORIENTED_EDGE('',*,*,#7041,.T.);
#9754=ORIENTED_EDGE('',*,*,#7007,.T.);
#9755=ORIENTED_EDGE('',*,*,#7038,.F.);
#9756=ORIENTED_EDGE('',*,*,#7014,.T.);
#9757=ORIENTED_EDGE('',*,*,#7035,.F.);
#9758=ORIENTED_EDGE('',*,*,#7020,.T.);
#9759=ORIENTED_EDGE('',*,*,#7033,.T.);
#9760=ORIENTED_EDGE('',*,*,#7032,.F.);
#9761=ORIENTED_EDGE('',*,*,#7023,.F.);
#9762=ORIENTED_EDGE('',*,*,#7024,.T.);
#9763=ORIENTED_EDGE('',*,*,#7021,.T.);
#9764=ORIENTED_EDGE('',*,*,#7013,.T.);
#9765=ORIENTED_EDGE('',*,*,#7044,.F.);
#9766=ORIENTED_EDGE('',*,*,#7045,.T.);
#9767=ORIENTED_EDGE('',*,*,#7046,.T.);
#9768=ORIENTED_EDGE('',*,*,#7045,.F.);
#9769=ORIENTED_EDGE('',*,*,#7047,.F.);
#9770=ORIENTED_EDGE('',*,*,#7048,.T.);
#9771=ORIENTED_EDGE('',*,*,#7049,.T.);
#9772=ORIENTED_EDGE('',*,*,#7050,.T.);
#9773=ORIENTED_EDGE('',*,*,#7051,.F.);
#9774=ORIENTED_EDGE('',*,*,#7052,.T.);
#9775=ORIENTED_EDGE('',*,*,#7053,.T.);
#9776=ORIENTED_EDGE('',*,*,#7054,.T.);
#9777=ORIENTED_EDGE('',*,*,#7055,.T.);
#9778=ORIENTED_EDGE('',*,*,#7056,.T.);
#9779=ORIENTED_EDGE('',*,*,#7057,.T.);
#9780=ORIENTED_EDGE('',*,*,#7058,.T.);
#9781=ORIENTED_EDGE('',*,*,#7059,.F.);
#9782=ORIENTED_EDGE('',*,*,#7060,.T.);
#9783=ORIENTED_EDGE('',*,*,#7061,.T.);
#9784=ORIENTED_EDGE('',*,*,#7056,.F.);
#9785=ORIENTED_EDGE('',*,*,#7062,.T.);
#9786=ORIENTED_EDGE('',*,*,#7063,.T.);
#9787=ORIENTED_EDGE('',*,*,#7064,.F.);
#9788=ORIENTED_EDGE('',*,*,#7065,.T.);
#9789=ORIENTED_EDGE('',*,*,#7066,.F.);
#9790=ORIENTED_EDGE('',*,*,#7067,.T.);
#9791=ORIENTED_EDGE('',*,*,#7068,.F.);
#9792=ORIENTED_EDGE('',*,*,#7069,.T.);
#9793=ORIENTED_EDGE('',*,*,#7070,.T.);
#9794=ORIENTED_EDGE('',*,*,#7069,.F.);
#9795=ORIENTED_EDGE('',*,*,#7071,.F.);
#9796=ORIENTED_EDGE('',*,*,#7072,.T.);
#9797=ORIENTED_EDGE('',*,*,#7073,.T.);
#9798=ORIENTED_EDGE('',*,*,#7074,.T.);
#9799=ORIENTED_EDGE('',*,*,#7075,.F.);
#9800=ORIENTED_EDGE('',*,*,#7076,.T.);
#9801=ORIENTED_EDGE('',*,*,#7077,.T.);
#9802=ORIENTED_EDGE('',*,*,#7078,.T.);
#9803=ORIENTED_EDGE('',*,*,#7079,.T.);
#9804=ORIENTED_EDGE('',*,*,#7080,.T.);
#9805=ORIENTED_EDGE('',*,*,#7081,.T.);
#9806=ORIENTED_EDGE('',*,*,#7082,.T.);
#9807=ORIENTED_EDGE('',*,*,#7083,.F.);
#9808=ORIENTED_EDGE('',*,*,#7084,.T.);
#9809=ORIENTED_EDGE('',*,*,#7085,.T.);
#9810=ORIENTED_EDGE('',*,*,#7080,.F.);
#9811=ORIENTED_EDGE('',*,*,#7086,.T.);
#9812=ORIENTED_EDGE('',*,*,#7087,.T.);
#9813=ORIENTED_EDGE('',*,*,#7088,.F.);
#9814=ORIENTED_EDGE('',*,*,#7089,.T.);
#9815=ORIENTED_EDGE('',*,*,#7090,.F.);
#9816=ORIENTED_EDGE('',*,*,#7091,.T.);
#9817=ORIENTED_EDGE('',*,*,#7092,.F.);
#9818=ORIENTED_EDGE('',*,*,#7093,.T.);
#9819=ORIENTED_EDGE('',*,*,#7094,.T.);
#9820=ORIENTED_EDGE('',*,*,#7093,.F.);
#9821=ORIENTED_EDGE('',*,*,#7095,.F.);
#9822=ORIENTED_EDGE('',*,*,#7096,.T.);
#9823=ORIENTED_EDGE('',*,*,#7097,.T.);
#9824=ORIENTED_EDGE('',*,*,#7098,.T.);
#9825=ORIENTED_EDGE('',*,*,#7099,.F.);
#9826=ORIENTED_EDGE('',*,*,#7100,.T.);
#9827=ORIENTED_EDGE('',*,*,#7101,.T.);
#9828=ORIENTED_EDGE('',*,*,#7102,.T.);
#9829=ORIENTED_EDGE('',*,*,#7103,.T.);
#9830=ORIENTED_EDGE('',*,*,#7104,.T.);
#9831=ORIENTED_EDGE('',*,*,#7105,.T.);
#9832=ORIENTED_EDGE('',*,*,#7106,.T.);
#9833=ORIENTED_EDGE('',*,*,#7107,.F.);
#9834=ORIENTED_EDGE('',*,*,#7108,.T.);
#9835=ORIENTED_EDGE('',*,*,#7109,.T.);
#9836=ORIENTED_EDGE('',*,*,#7104,.F.);
#9837=ORIENTED_EDGE('',*,*,#7110,.T.);
#9838=ORIENTED_EDGE('',*,*,#7111,.T.);
#9839=ORIENTED_EDGE('',*,*,#7112,.F.);
#9840=ORIENTED_EDGE('',*,*,#7113,.T.);
#9841=ORIENTED_EDGE('',*,*,#7114,.F.);
#9842=ORIENTED_EDGE('',*,*,#7115,.T.);
#9843=ORIENTED_EDGE('',*,*,#7116,.F.);
#9844=ORIENTED_EDGE('',*,*,#7117,.T.);
#9845=ORIENTED_EDGE('',*,*,#7118,.T.);
#9846=ORIENTED_EDGE('',*,*,#7117,.F.);
#9847=ORIENTED_EDGE('',*,*,#7119,.F.);
#9848=ORIENTED_EDGE('',*,*,#7120,.T.);
#9849=ORIENTED_EDGE('',*,*,#7121,.T.);
#9850=ORIENTED_EDGE('',*,*,#7122,.T.);
#9851=ORIENTED_EDGE('',*,*,#7123,.F.);
#9852=ORIENTED_EDGE('',*,*,#7124,.T.);
#9853=ORIENTED_EDGE('',*,*,#7125,.T.);
#9854=ORIENTED_EDGE('',*,*,#7126,.T.);
#9855=ORIENTED_EDGE('',*,*,#7127,.T.);
#9856=ORIENTED_EDGE('',*,*,#7128,.T.);
#9857=ORIENTED_EDGE('',*,*,#7129,.T.);
#9858=ORIENTED_EDGE('',*,*,#7130,.T.);
#9859=ORIENTED_EDGE('',*,*,#7131,.F.);
#9860=ORIENTED_EDGE('',*,*,#7132,.T.);
#9861=ORIENTED_EDGE('',*,*,#7133,.T.);
#9862=ORIENTED_EDGE('',*,*,#7128,.F.);
#9863=ORIENTED_EDGE('',*,*,#7134,.T.);
#9864=ORIENTED_EDGE('',*,*,#7135,.T.);
#9865=ORIENTED_EDGE('',*,*,#7136,.F.);
#9866=ORIENTED_EDGE('',*,*,#7137,.T.);
#9867=ORIENTED_EDGE('',*,*,#7138,.F.);
#9868=ORIENTED_EDGE('',*,*,#7139,.T.);
#9869=ORIENTED_EDGE('',*,*,#7140,.F.);
#9870=ORIENTED_EDGE('',*,*,#7141,.T.);
#9871=ORIENTED_EDGE('',*,*,#7142,.T.);
#9872=ORIENTED_EDGE('',*,*,#7141,.F.);
#9873=ORIENTED_EDGE('',*,*,#7143,.F.);
#9874=ORIENTED_EDGE('',*,*,#7144,.T.);
#9875=ORIENTED_EDGE('',*,*,#7145,.T.);
#9876=ORIENTED_EDGE('',*,*,#7146,.T.);
#9877=ORIENTED_EDGE('',*,*,#7147,.F.);
#9878=ORIENTED_EDGE('',*,*,#7148,.T.);
#9879=ORIENTED_EDGE('',*,*,#7149,.T.);
#9880=ORIENTED_EDGE('',*,*,#7150,.T.);
#9881=ORIENTED_EDGE('',*,*,#7151,.T.);
#9882=ORIENTED_EDGE('',*,*,#7152,.T.);
#9883=ORIENTED_EDGE('',*,*,#7153,.T.);
#9884=ORIENTED_EDGE('',*,*,#7154,.T.);
#9885=ORIENTED_EDGE('',*,*,#7155,.F.);
#9886=ORIENTED_EDGE('',*,*,#7156,.T.);
#9887=ORIENTED_EDGE('',*,*,#7157,.T.);
#9888=ORIENTED_EDGE('',*,*,#7152,.F.);
#9889=ORIENTED_EDGE('',*,*,#7158,.T.);
#9890=ORIENTED_EDGE('',*,*,#7159,.T.);
#9891=ORIENTED_EDGE('',*,*,#7160,.F.);
#9892=ORIENTED_EDGE('',*,*,#7161,.T.);
#9893=ORIENTED_EDGE('',*,*,#7162,.F.);
#9894=ORIENTED_EDGE('',*,*,#7163,.T.);
#9895=ORIENTED_EDGE('',*,*,#7164,.F.);
#9896=ORIENTED_EDGE('',*,*,#7165,.T.);
#9897=ORIENTED_EDGE('',*,*,#7166,.T.);
#9898=ORIENTED_EDGE('',*,*,#7165,.F.);
#9899=ORIENTED_EDGE('',*,*,#7167,.F.);
#9900=ORIENTED_EDGE('',*,*,#7168,.T.);
#9901=ORIENTED_EDGE('',*,*,#7169,.F.);
#9902=ORIENTED_EDGE('',*,*,#7170,.F.);
#9903=ORIENTED_EDGE('',*,*,#7171,.F.);
#9904=ORIENTED_EDGE('',*,*,#7172,.T.);
#9905=ORIENTED_EDGE('',*,*,#7173,.T.);
#9906=ORIENTED_EDGE('',*,*,#7174,.T.);
#9907=ORIENTED_EDGE('',*,*,#7175,.F.);
#9908=ORIENTED_EDGE('',*,*,#7176,.F.);
#9909=ORIENTED_EDGE('',*,*,#7177,.T.);
#9910=ORIENTED_EDGE('',*,*,#7178,.F.);
#9911=ORIENTED_EDGE('',*,*,#7179,.F.);
#9912=ORIENTED_EDGE('',*,*,#7180,.T.);
#9913=ORIENTED_EDGE('',*,*,#7181,.T.);
#9914=ORIENTED_EDGE('',*,*,#7182,.T.);
#9915=ORIENTED_EDGE('',*,*,#7183,.F.);
#9916=ORIENTED_EDGE('',*,*,#7184,.T.);
#9917=ORIENTED_EDGE('',*,*,#7185,.T.);
#9918=ORIENTED_EDGE('',*,*,#7180,.F.);
#9919=ORIENTED_EDGE('',*,*,#7186,.F.);
#9920=ORIENTED_EDGE('',*,*,#7187,.T.);
#9921=ORIENTED_EDGE('',*,*,#7188,.T.);
#9922=ORIENTED_EDGE('',*,*,#7189,.T.);
#9923=ORIENTED_EDGE('',*,*,#7190,.T.);
#9924=ORIENTED_EDGE('',*,*,#7191,.T.);
#9925=ORIENTED_EDGE('',*,*,#7192,.F.);
#9926=ORIENTED_EDGE('',*,*,#7193,.T.);
#9927=ORIENTED_EDGE('',*,*,#7194,.T.);
#9928=ORIENTED_EDGE('',*,*,#7189,.F.);
#9929=ORIENTED_EDGE('',*,*,#7195,.T.);
#9930=ORIENTED_EDGE('',*,*,#7196,.T.);
#9931=ORIENTED_EDGE('',*,*,#7197,.F.);
#9932=ORIENTED_EDGE('',*,*,#7198,.T.);
#9933=ORIENTED_EDGE('',*,*,#7199,.F.);
#9934=ORIENTED_EDGE('',*,*,#7200,.T.);
#9935=ORIENTED_EDGE('',*,*,#7201,.F.);
#9936=ORIENTED_EDGE('',*,*,#7202,.T.);
#9937=ORIENTED_EDGE('',*,*,#7203,.T.);
#9938=ORIENTED_EDGE('',*,*,#7202,.F.);
#9939=ORIENTED_EDGE('',*,*,#7204,.F.);
#9940=ORIENTED_EDGE('',*,*,#7205,.T.);
#9941=ORIENTED_EDGE('',*,*,#7206,.T.);
#9942=ORIENTED_EDGE('',*,*,#7207,.T.);
#9943=ORIENTED_EDGE('',*,*,#7208,.F.);
#9944=ORIENTED_EDGE('',*,*,#7209,.T.);
#9945=ORIENTED_EDGE('',*,*,#7210,.T.);
#9946=ORIENTED_EDGE('',*,*,#7211,.T.);
#9947=ORIENTED_EDGE('',*,*,#7212,.T.);
#9948=ORIENTED_EDGE('',*,*,#7169,.T.);
#9949=ORIENTED_EDGE('',*,*,#7213,.F.);
#9950=ORIENTED_EDGE('',*,*,#7211,.F.);
#9951=ORIENTED_EDGE('',*,*,#7214,.F.);
#9952=ORIENTED_EDGE('',*,*,#7167,.T.);
#9953=ORIENTED_EDGE('',*,*,#7215,.T.);
#9954=ORIENTED_EDGE('',*,*,#7209,.F.);
#9955=ORIENTED_EDGE('',*,*,#7168,.F.);
#9956=ORIENTED_EDGE('',*,*,#7214,.T.);
#9957=ORIENTED_EDGE('',*,*,#7208,.T.);
#9958=ORIENTED_EDGE('',*,*,#7213,.T.);
#9959=ORIENTED_EDGE('',*,*,#7215,.F.);
#9960=ORIENTED_EDGE('',*,*,#7170,.T.);
#9961=ORIENTED_EDGE('',*,*,#7212,.F.);
#9962=ORIENTED_EDGE('',*,*,#7210,.F.);
#9963=ORIENTED_EDGE('',*,*,#7201,.T.);
#9964=ORIENTED_EDGE('',*,*,#7200,.F.);
#9965=ORIENTED_EDGE('',*,*,#7203,.F.);
#9966=ORIENTED_EDGE('',*,*,#7199,.T.);
#9967=ORIENTED_EDGE('',*,*,#7216,.T.);
#9968=ORIENTED_EDGE('',*,*,#7192,.T.);
#9969=ORIENTED_EDGE('',*,*,#7217,.T.);
#9970=ORIENTED_EDGE('',*,*,#7197,.T.);
#9971=ORIENTED_EDGE('',*,*,#7194,.F.);
#9972=ORIENTED_EDGE('',*,*,#7218,.F.);
#9973=ORIENTED_EDGE('',*,*,#7195,.F.);
#9974=ORIENTED_EDGE('',*,*,#7188,.F.);
#9975=ORIENTED_EDGE('',*,*,#7219,.F.);
#9976=ORIENTED_EDGE('',*,*,#7190,.F.);
#9977=ORIENTED_EDGE('',*,*,#7191,.F.);
#9978=ORIENTED_EDGE('',*,*,#7219,.T.);
#9979=ORIENTED_EDGE('',*,*,#7198,.F.);
#9980=ORIENTED_EDGE('',*,*,#7217,.F.);
#9981=ORIENTED_EDGE('',*,*,#7193,.F.);
#9982=ORIENTED_EDGE('',*,*,#7216,.F.);
#9983=ORIENTED_EDGE('',*,*,#7196,.F.);
#9984=ORIENTED_EDGE('',*,*,#7218,.T.);
#9985=ORIENTED_EDGE('',*,*,#7166,.F.);
#9986=ORIENTED_EDGE('',*,*,#7186,.T.);
#9987=ORIENTED_EDGE('',*,*,#7164,.T.);
#9988=ORIENTED_EDGE('',*,*,#7187,.F.);
#9989=ORIENTED_EDGE('',*,*,#7145,.F.);
#9990=ORIENTED_EDGE('',*,*,#7220,.F.);
#9991=ORIENTED_EDGE('',*,*,#7173,.F.);
#9992=ORIENTED_EDGE('',*,*,#7221,.F.);
#9993=ORIENTED_EDGE('',*,*,#7222,.T.);
#9994=ORIENTED_EDGE('',*,*,#7143,.T.);
#9995=ORIENTED_EDGE('',*,*,#7223,.T.);
#9996=ORIENTED_EDGE('',*,*,#7171,.T.);
#9997=ORIENTED_EDGE('',*,*,#7146,.F.);
#9998=ORIENTED_EDGE('',*,*,#7221,.T.);
#9999=ORIENTED_EDGE('',*,*,#7172,.F.);
#10000=ORIENTED_EDGE('',*,*,#7223,.F.);
#10001=ORIENTED_EDGE('',*,*,#7144,.F.);
#10002=ORIENTED_EDGE('',*,*,#7222,.F.);
#10003=ORIENTED_EDGE('',*,*,#7174,.F.);
#10004=ORIENTED_EDGE('',*,*,#7220,.T.);
#10005=ORIENTED_EDGE('',*,*,#7156,.F.);
#10006=ORIENTED_EDGE('',*,*,#7224,.F.);
#10007=ORIENTED_EDGE('',*,*,#7159,.F.);
#10008=ORIENTED_EDGE('',*,*,#7225,.T.);
#10009=ORIENTED_EDGE('',*,*,#7154,.F.);
#10010=ORIENTED_EDGE('',*,*,#7226,.T.);
#10011=ORIENTED_EDGE('',*,*,#7161,.F.);
#10012=ORIENTED_EDGE('',*,*,#7227,.F.);
#10013=ORIENTED_EDGE('',*,*,#7157,.F.);
#10014=ORIENTED_EDGE('',*,*,#7225,.F.);
#10015=ORIENTED_EDGE('',*,*,#7158,.F.);
#10016=ORIENTED_EDGE('',*,*,#7151,.F.);
#10017=ORIENTED_EDGE('',*,*,#7226,.F.);
#10018=ORIENTED_EDGE('',*,*,#7153,.F.);
#10019=ORIENTED_EDGE('',*,*,#7224,.T.);
#10020=ORIENTED_EDGE('',*,*,#7155,.T.);
#10021=ORIENTED_EDGE('',*,*,#7227,.T.);
#10022=ORIENTED_EDGE('',*,*,#7160,.T.);
#10023=ORIENTED_EDGE('',*,*,#7142,.F.);
#10024=ORIENTED_EDGE('',*,*,#7162,.T.);
#10025=ORIENTED_EDGE('',*,*,#7140,.T.);
#10026=ORIENTED_EDGE('',*,*,#7163,.F.);
#10027=ORIENTED_EDGE('',*,*,#7121,.F.);
#10028=ORIENTED_EDGE('',*,*,#7228,.F.);
#10029=ORIENTED_EDGE('',*,*,#7149,.F.);
#10030=ORIENTED_EDGE('',*,*,#7229,.F.);
#10031=ORIENTED_EDGE('',*,*,#7230,.T.);
#10032=ORIENTED_EDGE('',*,*,#7119,.T.);
#10033=ORIENTED_EDGE('',*,*,#7231,.T.);
#10034=ORIENTED_EDGE('',*,*,#7147,.T.);
#10035=ORIENTED_EDGE('',*,*,#7122,.F.);
#10036=ORIENTED_EDGE('',*,*,#7229,.T.);
#10037=ORIENTED_EDGE('',*,*,#7148,.F.);
#10038=ORIENTED_EDGE('',*,*,#7231,.F.);
#10039=ORIENTED_EDGE('',*,*,#7120,.F.);
#10040=ORIENTED_EDGE('',*,*,#7230,.F.);
#10041=ORIENTED_EDGE('',*,*,#7150,.F.);
#10042=ORIENTED_EDGE('',*,*,#7228,.T.);
#10043=ORIENTED_EDGE('',*,*,#7132,.F.);
#10044=ORIENTED_EDGE('',*,*,#7232,.F.);
#10045=ORIENTED_EDGE('',*,*,#7135,.F.);
#10046=ORIENTED_EDGE('',*,*,#7233,.T.);
#10047=ORIENTED_EDGE('',*,*,#7130,.F.);
#10048=ORIENTED_EDGE('',*,*,#7234,.T.);
#10049=ORIENTED_EDGE('',*,*,#7137,.F.);
#10050=ORIENTED_EDGE('',*,*,#7235,.F.);
#10051=ORIENTED_EDGE('',*,*,#7133,.F.);
#10052=ORIENTED_EDGE('',*,*,#7233,.F.);
#10053=ORIENTED_EDGE('',*,*,#7134,.F.);
#10054=ORIENTED_EDGE('',*,*,#7127,.F.);
#10055=ORIENTED_EDGE('',*,*,#7234,.F.);
#10056=ORIENTED_EDGE('',*,*,#7129,.F.);
#10057=ORIENTED_EDGE('',*,*,#7232,.T.);
#10058=ORIENTED_EDGE('',*,*,#7131,.T.);
#10059=ORIENTED_EDGE('',*,*,#7235,.T.);
#10060=ORIENTED_EDGE('',*,*,#7136,.T.);
#10061=ORIENTED_EDGE('',*,*,#7118,.F.);
#10062=ORIENTED_EDGE('',*,*,#7138,.T.);
#10063=ORIENTED_EDGE('',*,*,#7116,.T.);
#10064=ORIENTED_EDGE('',*,*,#7139,.F.);
#10065=ORIENTED_EDGE('',*,*,#7097,.F.);
#10066=ORIENTED_EDGE('',*,*,#7236,.F.);
#10067=ORIENTED_EDGE('',*,*,#7125,.F.);
#10068=ORIENTED_EDGE('',*,*,#7237,.F.);
#10069=ORIENTED_EDGE('',*,*,#7238,.T.);
#10070=ORIENTED_EDGE('',*,*,#7095,.T.);
#10071=ORIENTED_EDGE('',*,*,#7239,.T.);
#10072=ORIENTED_EDGE('',*,*,#7123,.T.);
#10073=ORIENTED_EDGE('',*,*,#7098,.F.);
#10074=ORIENTED_EDGE('',*,*,#7237,.T.);
#10075=ORIENTED_EDGE('',*,*,#7124,.F.);
#10076=ORIENTED_EDGE('',*,*,#7239,.F.);
#10077=ORIENTED_EDGE('',*,*,#7096,.F.);
#10078=ORIENTED_EDGE('',*,*,#7238,.F.);
#10079=ORIENTED_EDGE('',*,*,#7126,.F.);
#10080=ORIENTED_EDGE('',*,*,#7236,.T.);
#10081=ORIENTED_EDGE('',*,*,#7108,.F.);
#10082=ORIENTED_EDGE('',*,*,#7240,.F.);
#10083=ORIENTED_EDGE('',*,*,#7111,.F.);
#10084=ORIENTED_EDGE('',*,*,#7241,.T.);
#10085=ORIENTED_EDGE('',*,*,#7106,.F.);
#10086=ORIENTED_EDGE('',*,*,#7242,.T.);
#10087=ORIENTED_EDGE('',*,*,#7113,.F.);
#10088=ORIENTED_EDGE('',*,*,#7243,.F.);
#10089=ORIENTED_EDGE('',*,*,#7109,.F.);
#10090=ORIENTED_EDGE('',*,*,#7241,.F.);
#10091=ORIENTED_EDGE('',*,*,#7110,.F.);
#10092=ORIENTED_EDGE('',*,*,#7103,.F.);
#10093=ORIENTED_EDGE('',*,*,#7242,.F.);
#10094=ORIENTED_EDGE('',*,*,#7105,.F.);
#10095=ORIENTED_EDGE('',*,*,#7240,.T.);
#10096=ORIENTED_EDGE('',*,*,#7107,.T.);
#10097=ORIENTED_EDGE('',*,*,#7243,.T.);
#10098=ORIENTED_EDGE('',*,*,#7112,.T.);
#10099=ORIENTED_EDGE('',*,*,#7094,.F.);
#10100=ORIENTED_EDGE('',*,*,#7114,.T.);
#10101=ORIENTED_EDGE('',*,*,#7092,.T.);
#10102=ORIENTED_EDGE('',*,*,#7115,.F.);
#10103=ORIENTED_EDGE('',*,*,#7073,.F.);
#10104=ORIENTED_EDGE('',*,*,#7244,.F.);
#10105=ORIENTED_EDGE('',*,*,#7101,.F.);
#10106=ORIENTED_EDGE('',*,*,#7245,.F.);
#10107=ORIENTED_EDGE('',*,*,#7246,.T.);
#10108=ORIENTED_EDGE('',*,*,#7071,.T.);
#10109=ORIENTED_EDGE('',*,*,#7247,.T.);
#10110=ORIENTED_EDGE('',*,*,#7099,.T.);
#10111=ORIENTED_EDGE('',*,*,#7074,.F.);
#10112=ORIENTED_EDGE('',*,*,#7245,.T.);
#10113=ORIENTED_EDGE('',*,*,#7100,.F.);
#10114=ORIENTED_EDGE('',*,*,#7247,.F.);
#10115=ORIENTED_EDGE('',*,*,#7072,.F.);
#10116=ORIENTED_EDGE('',*,*,#7246,.F.);
#10117=ORIENTED_EDGE('',*,*,#7102,.F.);
#10118=ORIENTED_EDGE('',*,*,#7244,.T.);
#10119=ORIENTED_EDGE('',*,*,#7084,.F.);
#10120=ORIENTED_EDGE('',*,*,#7248,.F.);
#10121=ORIENTED_EDGE('',*,*,#7087,.F.);
#10122=ORIENTED_EDGE('',*,*,#7249,.T.);
#10123=ORIENTED_EDGE('',*,*,#7082,.F.);
#10124=ORIENTED_EDGE('',*,*,#7250,.T.);
#10125=ORIENTED_EDGE('',*,*,#7089,.F.);
#10126=ORIENTED_EDGE('',*,*,#7251,.F.);
#10127=ORIENTED_EDGE('',*,*,#7085,.F.);
#10128=ORIENTED_EDGE('',*,*,#7249,.F.);
#10129=ORIENTED_EDGE('',*,*,#7086,.F.);
#10130=ORIENTED_EDGE('',*,*,#7079,.F.);
#10131=ORIENTED_EDGE('',*,*,#7250,.F.);
#10132=ORIENTED_EDGE('',*,*,#7081,.F.);
#10133=ORIENTED_EDGE('',*,*,#7248,.T.);
#10134=ORIENTED_EDGE('',*,*,#7083,.T.);
#10135=ORIENTED_EDGE('',*,*,#7251,.T.);
#10136=ORIENTED_EDGE('',*,*,#7088,.T.);
#10137=ORIENTED_EDGE('',*,*,#7070,.F.);
#10138=ORIENTED_EDGE('',*,*,#7090,.T.);
#10139=ORIENTED_EDGE('',*,*,#7068,.T.);
#10140=ORIENTED_EDGE('',*,*,#7091,.F.);
#10141=ORIENTED_EDGE('',*,*,#7049,.F.);
#10142=ORIENTED_EDGE('',*,*,#7252,.F.);
#10143=ORIENTED_EDGE('',*,*,#7077,.F.);
#10144=ORIENTED_EDGE('',*,*,#7253,.F.);
#10145=ORIENTED_EDGE('',*,*,#7254,.T.);
#10146=ORIENTED_EDGE('',*,*,#7047,.T.);
#10147=ORIENTED_EDGE('',*,*,#7255,.T.);
#10148=ORIENTED_EDGE('',*,*,#7075,.T.);
#10149=ORIENTED_EDGE('',*,*,#7050,.F.);
#10150=ORIENTED_EDGE('',*,*,#7253,.T.);
#10151=ORIENTED_EDGE('',*,*,#7076,.F.);
#10152=ORIENTED_EDGE('',*,*,#7255,.F.);
#10153=ORIENTED_EDGE('',*,*,#7048,.F.);
#10154=ORIENTED_EDGE('',*,*,#7254,.F.);
#10155=ORIENTED_EDGE('',*,*,#7078,.F.);
#10156=ORIENTED_EDGE('',*,*,#7252,.T.);
#10157=ORIENTED_EDGE('',*,*,#7060,.F.);
#10158=ORIENTED_EDGE('',*,*,#7256,.F.);
#10159=ORIENTED_EDGE('',*,*,#7063,.F.);
#10160=ORIENTED_EDGE('',*,*,#7257,.T.);
#10161=ORIENTED_EDGE('',*,*,#7058,.F.);
#10162=ORIENTED_EDGE('',*,*,#7258,.T.);
#10163=ORIENTED_EDGE('',*,*,#7065,.F.);
#10164=ORIENTED_EDGE('',*,*,#7259,.F.);
#10165=ORIENTED_EDGE('',*,*,#7061,.F.);
#10166=ORIENTED_EDGE('',*,*,#7257,.F.);
#10167=ORIENTED_EDGE('',*,*,#7062,.F.);
#10168=ORIENTED_EDGE('',*,*,#7055,.F.);
#10169=ORIENTED_EDGE('',*,*,#7258,.F.);
#10170=ORIENTED_EDGE('',*,*,#7057,.F.);
#10171=ORIENTED_EDGE('',*,*,#7256,.T.);
#10172=ORIENTED_EDGE('',*,*,#7059,.T.);
#10173=ORIENTED_EDGE('',*,*,#7259,.T.);
#10174=ORIENTED_EDGE('',*,*,#7064,.T.);
#10175=ORIENTED_EDGE('',*,*,#7046,.F.);
#10176=ORIENTED_EDGE('',*,*,#7066,.T.);
#10177=ORIENTED_EDGE('',*,*,#7044,.T.);
#10178=ORIENTED_EDGE('',*,*,#7067,.F.);
#10179=ORIENTED_EDGE('',*,*,#7206,.F.);
#10180=ORIENTED_EDGE('',*,*,#7260,.F.);
#10181=ORIENTED_EDGE('',*,*,#7053,.F.);
#10182=ORIENTED_EDGE('',*,*,#7261,.F.);
#10183=ORIENTED_EDGE('',*,*,#7262,.T.);
#10184=ORIENTED_EDGE('',*,*,#7204,.T.);
#10185=ORIENTED_EDGE('',*,*,#7263,.T.);
#10186=ORIENTED_EDGE('',*,*,#7051,.T.);
#10187=ORIENTED_EDGE('',*,*,#7207,.F.);
#10188=ORIENTED_EDGE('',*,*,#7261,.T.);
#10189=ORIENTED_EDGE('',*,*,#7052,.F.);
#10190=ORIENTED_EDGE('',*,*,#7263,.F.);
#10191=ORIENTED_EDGE('',*,*,#7205,.F.);
#10192=ORIENTED_EDGE('',*,*,#7262,.F.);
#10193=ORIENTED_EDGE('',*,*,#7054,.F.);
#10194=ORIENTED_EDGE('',*,*,#7260,.T.);
#10195=ORIENTED_EDGE('',*,*,#7177,.F.);
#10196=ORIENTED_EDGE('',*,*,#7264,.T.);
#10197=ORIENTED_EDGE('',*,*,#7183,.T.);
#10198=ORIENTED_EDGE('',*,*,#7265,.T.);
#10199=ORIENTED_EDGE('',*,*,#7266,.F.);
#10200=ORIENTED_EDGE('',*,*,#7175,.T.);
#10201=ORIENTED_EDGE('',*,*,#7179,.T.);
#10202=ORIENTED_EDGE('',*,*,#7267,.F.);
#10203=ORIENTED_EDGE('',*,*,#7181,.F.);
#10204=ORIENTED_EDGE('',*,*,#7185,.F.);
#10205=ORIENTED_EDGE('',*,*,#7267,.T.);
#10206=ORIENTED_EDGE('',*,*,#7178,.T.);
#10207=ORIENTED_EDGE('',*,*,#7265,.F.);
#10208=ORIENTED_EDGE('',*,*,#7182,.F.);
#10209=ORIENTED_EDGE('',*,*,#7264,.F.);
#10210=ORIENTED_EDGE('',*,*,#7176,.T.);
#10211=ORIENTED_EDGE('',*,*,#7266,.T.);
#10212=ORIENTED_EDGE('',*,*,#7184,.F.);
#10213=ORIENTED_EDGE('',*,*,#7268,.F.);
#10214=ORIENTED_EDGE('',*,*,#7269,.T.);
#10215=ORIENTED_EDGE('',*,*,#7270,.T.);
#10216=ORIENTED_EDGE('',*,*,#7269,.F.);
#10217=ORIENTED_EDGE('',*,*,#7271,.F.);
#10218=ORIENTED_EDGE('',*,*,#7272,.F.);
#10219=ORIENTED_EDGE('',*,*,#7273,.T.);
#10220=ORIENTED_EDGE('',*,*,#7274,.F.);
#10221=ORIENTED_EDGE('',*,*,#7275,.F.);
#10222=ORIENTED_EDGE('',*,*,#7273,.F.);
#10223=ORIENTED_EDGE('',*,*,#7276,.F.);
#10224=ORIENTED_EDGE('',*,*,#7277,.F.);
#10225=ORIENTED_EDGE('',*,*,#7278,.T.);
#10226=ORIENTED_EDGE('',*,*,#7279,.F.);
#10227=ORIENTED_EDGE('',*,*,#7278,.F.);
#10228=ORIENTED_EDGE('',*,*,#7271,.T.);
#10229=ORIENTED_EDGE('',*,*,#7272,.T.);
#10230=ORIENTED_EDGE('',*,*,#7280,.T.);
#10231=ORIENTED_EDGE('',*,*,#7281,.T.);
#10232=ORIENTED_EDGE('',*,*,#7280,.F.);
#10233=ORIENTED_EDGE('',*,*,#7276,.T.);
#10234=ORIENTED_EDGE('',*,*,#7277,.T.);
#10235=ORIENTED_EDGE('',*,*,#7282,.T.);
#10236=ORIENTED_EDGE('',*,*,#7274,.T.);
#10237=ORIENTED_EDGE('',*,*,#7275,.T.);
#10238=ORIENTED_EDGE('',*,*,#7282,.F.);
#10239=ORIENTED_EDGE('',*,*,#7279,.T.);
#10240=ORIENTED_EDGE('',*,*,#7283,.T.);
#10241=ORIENTED_EDGE('',*,*,#7284,.F.);
#10242=ORIENTED_EDGE('',*,*,#7283,.F.);
#10243=ORIENTED_EDGE('',*,*,#7270,.F.);
#10244=ORIENTED_EDGE('',*,*,#7285,.T.);
#10245=ORIENTED_EDGE('',*,*,#7286,.T.);
#10246=ORIENTED_EDGE('',*,*,#7285,.F.);
#10247=ORIENTED_EDGE('',*,*,#7287,.F.);
#10248=ORIENTED_EDGE('',*,*,#7288,.T.);
#10249=ORIENTED_EDGE('',*,*,#7268,.T.);
#10250=ORIENTED_EDGE('',*,*,#7288,.F.);
#10251=ORIENTED_EDGE('',*,*,#7287,.T.);
#10252=ORIENTED_EDGE('',*,*,#7281,.F.);
#10253=ORIENTED_EDGE('',*,*,#7286,.F.);
#10254=ORIENTED_EDGE('',*,*,#7284,.T.);
#10255=ORIENTED_EDGE('',*,*,#7289,.T.);
#10256=ORIENTED_EDGE('',*,*,#7289,.F.);
#10257=ORIENTED_EDGE('',*,*,#7290,.T.);
#10258=ORIENTED_EDGE('',*,*,#7290,.F.);
#10259=ORIENTED_EDGE('',*,*,#7291,.T.);
#10260=ORIENTED_EDGE('',*,*,#7291,.F.);
#10261=ORIENTED_EDGE('',*,*,#7292,.T.);
#10262=ORIENTED_EDGE('',*,*,#7292,.F.);
#10263=ORIENTED_EDGE('',*,*,#7293,.T.);
#10264=ORIENTED_EDGE('',*,*,#7293,.F.);
#10265=ORIENTED_EDGE('',*,*,#7294,.T.);
#10266=ORIENTED_EDGE('',*,*,#7294,.F.);
#10267=ORIENTED_EDGE('',*,*,#7295,.T.);
#10268=ORIENTED_EDGE('',*,*,#7295,.F.);
#10269=ORIENTED_EDGE('',*,*,#7296,.F.);
#10270=ORIENTED_EDGE('',*,*,#7297,.T.);
#10271=ORIENTED_EDGE('',*,*,#7298,.F.);
#10272=ORIENTED_EDGE('',*,*,#7299,.F.);
#10273=ORIENTED_EDGE('',*,*,#7297,.F.);
#10274=ORIENTED_EDGE('',*,*,#7300,.F.);
#10275=ORIENTED_EDGE('',*,*,#7301,.T.);
#10276=ORIENTED_EDGE('',*,*,#7302,.F.);
#10277=ORIENTED_EDGE('',*,*,#7301,.F.);
#10278=ORIENTED_EDGE('',*,*,#7303,.F.);
#10279=ORIENTED_EDGE('',*,*,#7304,.T.);
#10280=ORIENTED_EDGE('',*,*,#7305,.F.);
#10281=ORIENTED_EDGE('',*,*,#7304,.F.);
#10282=ORIENTED_EDGE('',*,*,#7306,.F.);
#10283=ORIENTED_EDGE('',*,*,#7307,.F.);
#10284=ORIENTED_EDGE('',*,*,#7308,.T.);
#10285=ORIENTED_EDGE('',*,*,#7309,.F.);
#10286=ORIENTED_EDGE('',*,*,#7308,.F.);
#10287=ORIENTED_EDGE('',*,*,#7310,.F.);
#10288=ORIENTED_EDGE('',*,*,#7311,.T.);
#10289=ORIENTED_EDGE('',*,*,#7312,.T.);
#10290=ORIENTED_EDGE('',*,*,#7311,.F.);
#10291=ORIENTED_EDGE('',*,*,#7313,.F.);
#10292=ORIENTED_EDGE('',*,*,#7314,.T.);
#10293=ORIENTED_EDGE('',*,*,#7298,.T.);
#10294=ORIENTED_EDGE('',*,*,#7299,.T.);
#10295=ORIENTED_EDGE('',*,*,#7314,.F.);
#10296=ORIENTED_EDGE('',*,*,#7306,.T.);
#10297=ORIENTED_EDGE('',*,*,#7307,.T.);
#10298=ORIENTED_EDGE('',*,*,#7315,.T.);
#10299=ORIENTED_EDGE('',*,*,#7316,.T.);
#10300=ORIENTED_EDGE('',*,*,#7315,.F.);
#10301=ORIENTED_EDGE('',*,*,#7316,.F.);
#10302=ORIENTED_EDGE('',*,*,#7317,.T.);
#10303=ORIENTED_EDGE('',*,*,#7318,.T.);
#10304=ORIENTED_EDGE('',*,*,#7317,.F.);
#10305=ORIENTED_EDGE('',*,*,#7318,.F.);
#10306=ORIENTED_EDGE('',*,*,#7319,.T.);
#10307=ORIENTED_EDGE('',*,*,#7300,.T.);
#10308=ORIENTED_EDGE('',*,*,#7319,.F.);
#10309=ORIENTED_EDGE('',*,*,#7305,.T.);
#10310=ORIENTED_EDGE('',*,*,#7320,.T.);
#10311=ORIENTED_EDGE('',*,*,#7321,.T.);
#10312=ORIENTED_EDGE('',*,*,#7320,.F.);
#10313=ORIENTED_EDGE('',*,*,#7322,.F.);
#10314=ORIENTED_EDGE('',*,*,#7323,.T.);
#10315=ORIENTED_EDGE('',*,*,#7324,.T.);
#10316=ORIENTED_EDGE('',*,*,#7323,.F.);
#10317=ORIENTED_EDGE('',*,*,#7325,.F.);
#10318=ORIENTED_EDGE('',*,*,#7326,.T.);
#10319=ORIENTED_EDGE('',*,*,#7327,.T.);
#10320=ORIENTED_EDGE('',*,*,#7326,.F.);
#10321=ORIENTED_EDGE('',*,*,#7328,.T.);
#10322=ORIENTED_EDGE('',*,*,#7329,.T.);
#10323=ORIENTED_EDGE('',*,*,#7330,.F.);
#10324=ORIENTED_EDGE('',*,*,#7329,.F.);
#10325=ORIENTED_EDGE('',*,*,#7331,.T.);
#10326=ORIENTED_EDGE('',*,*,#7328,.F.);
#10327=ORIENTED_EDGE('',*,*,#7332,.T.);
#10328=ORIENTED_EDGE('',*,*,#7325,.T.);
#10329=ORIENTED_EDGE('',*,*,#7332,.F.);
#10330=ORIENTED_EDGE('',*,*,#7331,.F.);
#10331=ORIENTED_EDGE('',*,*,#7330,.T.);
#10332=ORIENTED_EDGE('',*,*,#7296,.T.);
#10333=ORIENTED_EDGE('',*,*,#7327,.F.);
#10334=ORIENTED_EDGE('',*,*,#7303,.T.);
#10335=ORIENTED_EDGE('',*,*,#7324,.F.);
#10336=ORIENTED_EDGE('',*,*,#7309,.T.);
#10337=ORIENTED_EDGE('',*,*,#7322,.T.);
#10338=ORIENTED_EDGE('',*,*,#7321,.F.);
#10339=ORIENTED_EDGE('',*,*,#7312,.F.);
#10340=ORIENTED_EDGE('',*,*,#7313,.T.);
#10341=ORIENTED_EDGE('',*,*,#7310,.T.);
#10342=ORIENTED_EDGE('',*,*,#7302,.T.);
#10343=ORIENTED_EDGE('',*,*,#7333,.F.);
#10344=ORIENTED_EDGE('',*,*,#7334,.T.);
#10345=ORIENTED_EDGE('',*,*,#7335,.T.);
#10346=ORIENTED_EDGE('',*,*,#7334,.F.);
#10347=ORIENTED_EDGE('',*,*,#7336,.F.);
#10348=ORIENTED_EDGE('',*,*,#7337,.T.);
#10349=ORIENTED_EDGE('',*,*,#7338,.T.);
#10350=ORIENTED_EDGE('',*,*,#7339,.T.);
#10351=ORIENTED_EDGE('',*,*,#7340,.F.);
#10352=ORIENTED_EDGE('',*,*,#7341,.T.);
#10353=ORIENTED_EDGE('',*,*,#7342,.T.);
#10354=ORIENTED_EDGE('',*,*,#7343,.T.);
#10355=ORIENTED_EDGE('',*,*,#7344,.T.);
#10356=ORIENTED_EDGE('',*,*,#7345,.T.);
#10357=ORIENTED_EDGE('',*,*,#7346,.T.);
#10358=ORIENTED_EDGE('',*,*,#7347,.T.);
#10359=ORIENTED_EDGE('',*,*,#7348,.F.);
#10360=ORIENTED_EDGE('',*,*,#7349,.T.);
#10361=ORIENTED_EDGE('',*,*,#7350,.T.);
#10362=ORIENTED_EDGE('',*,*,#7345,.F.);
#10363=ORIENTED_EDGE('',*,*,#7351,.T.);
#10364=ORIENTED_EDGE('',*,*,#7352,.T.);
#10365=ORIENTED_EDGE('',*,*,#7353,.F.);
#10366=ORIENTED_EDGE('',*,*,#7354,.T.);
#10367=ORIENTED_EDGE('',*,*,#7355,.F.);
#10368=ORIENTED_EDGE('',*,*,#7356,.T.);
#10369=ORIENTED_EDGE('',*,*,#7357,.F.);
#10370=ORIENTED_EDGE('',*,*,#7358,.T.);
#10371=ORIENTED_EDGE('',*,*,#7359,.T.);
#10372=ORIENTED_EDGE('',*,*,#7358,.F.);
#10373=ORIENTED_EDGE('',*,*,#7360,.F.);
#10374=ORIENTED_EDGE('',*,*,#7361,.T.);
#10375=ORIENTED_EDGE('',*,*,#7362,.T.);
#10376=ORIENTED_EDGE('',*,*,#7363,.T.);
#10377=ORIENTED_EDGE('',*,*,#7364,.F.);
#10378=ORIENTED_EDGE('',*,*,#7365,.T.);
#10379=ORIENTED_EDGE('',*,*,#7366,.T.);
#10380=ORIENTED_EDGE('',*,*,#7367,.T.);
#10381=ORIENTED_EDGE('',*,*,#7368,.T.);
#10382=ORIENTED_EDGE('',*,*,#7369,.T.);
#10383=ORIENTED_EDGE('',*,*,#7370,.T.);
#10384=ORIENTED_EDGE('',*,*,#7371,.T.);
#10385=ORIENTED_EDGE('',*,*,#7372,.F.);
#10386=ORIENTED_EDGE('',*,*,#7373,.T.);
#10387=ORIENTED_EDGE('',*,*,#7374,.T.);
#10388=ORIENTED_EDGE('',*,*,#7369,.F.);
#10389=ORIENTED_EDGE('',*,*,#7375,.T.);
#10390=ORIENTED_EDGE('',*,*,#7376,.T.);
#10391=ORIENTED_EDGE('',*,*,#7377,.F.);
#10392=ORIENTED_EDGE('',*,*,#7378,.T.);
#10393=ORIENTED_EDGE('',*,*,#7379,.F.);
#10394=ORIENTED_EDGE('',*,*,#7380,.T.);
#10395=ORIENTED_EDGE('',*,*,#7381,.F.);
#10396=ORIENTED_EDGE('',*,*,#7382,.T.);
#10397=ORIENTED_EDGE('',*,*,#7383,.T.);
#10398=ORIENTED_EDGE('',*,*,#7382,.F.);
#10399=ORIENTED_EDGE('',*,*,#7384,.F.);
#10400=ORIENTED_EDGE('',*,*,#7385,.T.);
#10401=ORIENTED_EDGE('',*,*,#7386,.T.);
#10402=ORIENTED_EDGE('',*,*,#7387,.T.);
#10403=ORIENTED_EDGE('',*,*,#7388,.F.);
#10404=ORIENTED_EDGE('',*,*,#7389,.T.);
#10405=ORIENTED_EDGE('',*,*,#7390,.T.);
#10406=ORIENTED_EDGE('',*,*,#7391,.T.);
#10407=ORIENTED_EDGE('',*,*,#7392,.T.);
#10408=ORIENTED_EDGE('',*,*,#7393,.T.);
#10409=ORIENTED_EDGE('',*,*,#7394,.T.);
#10410=ORIENTED_EDGE('',*,*,#7395,.T.);
#10411=ORIENTED_EDGE('',*,*,#7396,.F.);
#10412=ORIENTED_EDGE('',*,*,#7397,.T.);
#10413=ORIENTED_EDGE('',*,*,#7398,.T.);
#10414=ORIENTED_EDGE('',*,*,#7393,.F.);
#10415=ORIENTED_EDGE('',*,*,#7399,.T.);
#10416=ORIENTED_EDGE('',*,*,#7400,.T.);
#10417=ORIENTED_EDGE('',*,*,#7401,.F.);
#10418=ORIENTED_EDGE('',*,*,#7402,.T.);
#10419=ORIENTED_EDGE('',*,*,#7403,.F.);
#10420=ORIENTED_EDGE('',*,*,#7404,.T.);
#10421=ORIENTED_EDGE('',*,*,#7405,.F.);
#10422=ORIENTED_EDGE('',*,*,#7406,.T.);
#10423=ORIENTED_EDGE('',*,*,#7407,.T.);
#10424=ORIENTED_EDGE('',*,*,#7406,.F.);
#10425=ORIENTED_EDGE('',*,*,#7408,.F.);
#10426=ORIENTED_EDGE('',*,*,#7409,.T.);
#10427=ORIENTED_EDGE('',*,*,#7410,.T.);
#10428=ORIENTED_EDGE('',*,*,#7411,.T.);
#10429=ORIENTED_EDGE('',*,*,#7412,.F.);
#10430=ORIENTED_EDGE('',*,*,#7413,.T.);
#10431=ORIENTED_EDGE('',*,*,#7414,.T.);
#10432=ORIENTED_EDGE('',*,*,#7415,.T.);
#10433=ORIENTED_EDGE('',*,*,#7416,.T.);
#10434=ORIENTED_EDGE('',*,*,#7417,.T.);
#10435=ORIENTED_EDGE('',*,*,#7418,.T.);
#10436=ORIENTED_EDGE('',*,*,#7419,.T.);
#10437=ORIENTED_EDGE('',*,*,#7420,.F.);
#10438=ORIENTED_EDGE('',*,*,#7421,.T.);
#10439=ORIENTED_EDGE('',*,*,#7422,.T.);
#10440=ORIENTED_EDGE('',*,*,#7417,.F.);
#10441=ORIENTED_EDGE('',*,*,#7423,.T.);
#10442=ORIENTED_EDGE('',*,*,#7424,.T.);
#10443=ORIENTED_EDGE('',*,*,#7425,.F.);
#10444=ORIENTED_EDGE('',*,*,#7426,.T.);
#10445=ORIENTED_EDGE('',*,*,#7427,.F.);
#10446=ORIENTED_EDGE('',*,*,#7428,.T.);
#10447=ORIENTED_EDGE('',*,*,#7429,.F.);
#10448=ORIENTED_EDGE('',*,*,#7430,.T.);
#10449=ORIENTED_EDGE('',*,*,#7431,.T.);
#10450=ORIENTED_EDGE('',*,*,#7430,.F.);
#10451=ORIENTED_EDGE('',*,*,#7432,.F.);
#10452=ORIENTED_EDGE('',*,*,#7433,.T.);
#10453=ORIENTED_EDGE('',*,*,#7434,.T.);
#10454=ORIENTED_EDGE('',*,*,#7435,.T.);
#10455=ORIENTED_EDGE('',*,*,#7436,.F.);
#10456=ORIENTED_EDGE('',*,*,#7437,.T.);
#10457=ORIENTED_EDGE('',*,*,#7438,.T.);
#10458=ORIENTED_EDGE('',*,*,#7439,.T.);
#10459=ORIENTED_EDGE('',*,*,#7440,.T.);
#10460=ORIENTED_EDGE('',*,*,#7441,.T.);
#10461=ORIENTED_EDGE('',*,*,#7442,.T.);
#10462=ORIENTED_EDGE('',*,*,#7443,.T.);
#10463=ORIENTED_EDGE('',*,*,#7444,.F.);
#10464=ORIENTED_EDGE('',*,*,#7445,.T.);
#10465=ORIENTED_EDGE('',*,*,#7446,.T.);
#10466=ORIENTED_EDGE('',*,*,#7441,.F.);
#10467=ORIENTED_EDGE('',*,*,#7447,.T.);
#10468=ORIENTED_EDGE('',*,*,#7448,.T.);
#10469=ORIENTED_EDGE('',*,*,#7449,.F.);
#10470=ORIENTED_EDGE('',*,*,#7450,.T.);
#10471=ORIENTED_EDGE('',*,*,#7451,.F.);
#10472=ORIENTED_EDGE('',*,*,#7452,.T.);
#10473=ORIENTED_EDGE('',*,*,#7453,.F.);
#10474=ORIENTED_EDGE('',*,*,#7454,.T.);
#10475=ORIENTED_EDGE('',*,*,#7455,.T.);
#10476=ORIENTED_EDGE('',*,*,#7454,.F.);
#10477=ORIENTED_EDGE('',*,*,#7456,.F.);
#10478=ORIENTED_EDGE('',*,*,#7457,.T.);
#10479=ORIENTED_EDGE('',*,*,#7458,.F.);
#10480=ORIENTED_EDGE('',*,*,#7459,.F.);
#10481=ORIENTED_EDGE('',*,*,#7460,.F.);
#10482=ORIENTED_EDGE('',*,*,#7461,.T.);
#10483=ORIENTED_EDGE('',*,*,#7462,.T.);
#10484=ORIENTED_EDGE('',*,*,#7463,.T.);
#10485=ORIENTED_EDGE('',*,*,#7464,.F.);
#10486=ORIENTED_EDGE('',*,*,#7465,.F.);
#10487=ORIENTED_EDGE('',*,*,#7466,.T.);
#10488=ORIENTED_EDGE('',*,*,#7467,.F.);
#10489=ORIENTED_EDGE('',*,*,#7468,.F.);
#10490=ORIENTED_EDGE('',*,*,#7469,.T.);
#10491=ORIENTED_EDGE('',*,*,#7470,.T.);
#10492=ORIENTED_EDGE('',*,*,#7471,.T.);
#10493=ORIENTED_EDGE('',*,*,#7472,.F.);
#10494=ORIENTED_EDGE('',*,*,#7473,.T.);
#10495=ORIENTED_EDGE('',*,*,#7474,.T.);
#10496=ORIENTED_EDGE('',*,*,#7469,.F.);
#10497=ORIENTED_EDGE('',*,*,#7475,.F.);
#10498=ORIENTED_EDGE('',*,*,#7476,.T.);
#10499=ORIENTED_EDGE('',*,*,#7477,.T.);
#10500=ORIENTED_EDGE('',*,*,#7478,.T.);
#10501=ORIENTED_EDGE('',*,*,#7479,.T.);
#10502=ORIENTED_EDGE('',*,*,#7480,.T.);
#10503=ORIENTED_EDGE('',*,*,#7481,.F.);
#10504=ORIENTED_EDGE('',*,*,#7482,.T.);
#10505=ORIENTED_EDGE('',*,*,#7483,.T.);
#10506=ORIENTED_EDGE('',*,*,#7478,.F.);
#10507=ORIENTED_EDGE('',*,*,#7484,.T.);
#10508=ORIENTED_EDGE('',*,*,#7485,.T.);
#10509=ORIENTED_EDGE('',*,*,#7486,.F.);
#10510=ORIENTED_EDGE('',*,*,#7487,.T.);
#10511=ORIENTED_EDGE('',*,*,#7488,.F.);
#10512=ORIENTED_EDGE('',*,*,#7489,.T.);
#10513=ORIENTED_EDGE('',*,*,#7490,.F.);
#10514=ORIENTED_EDGE('',*,*,#7491,.T.);
#10515=ORIENTED_EDGE('',*,*,#7492,.T.);
#10516=ORIENTED_EDGE('',*,*,#7491,.F.);
#10517=ORIENTED_EDGE('',*,*,#7493,.F.);
#10518=ORIENTED_EDGE('',*,*,#7494,.T.);
#10519=ORIENTED_EDGE('',*,*,#7495,.T.);
#10520=ORIENTED_EDGE('',*,*,#7496,.T.);
#10521=ORIENTED_EDGE('',*,*,#7497,.F.);
#10522=ORIENTED_EDGE('',*,*,#7498,.T.);
#10523=ORIENTED_EDGE('',*,*,#7499,.T.);
#10524=ORIENTED_EDGE('',*,*,#7500,.T.);
#10525=ORIENTED_EDGE('',*,*,#7501,.T.);
#10526=ORIENTED_EDGE('',*,*,#7458,.T.);
#10527=ORIENTED_EDGE('',*,*,#7502,.F.);
#10528=ORIENTED_EDGE('',*,*,#7500,.F.);
#10529=ORIENTED_EDGE('',*,*,#7503,.F.);
#10530=ORIENTED_EDGE('',*,*,#7456,.T.);
#10531=ORIENTED_EDGE('',*,*,#7504,.T.);
#10532=ORIENTED_EDGE('',*,*,#7498,.F.);
#10533=ORIENTED_EDGE('',*,*,#7457,.F.);
#10534=ORIENTED_EDGE('',*,*,#7503,.T.);
#10535=ORIENTED_EDGE('',*,*,#7497,.T.);
#10536=ORIENTED_EDGE('',*,*,#7502,.T.);
#10537=ORIENTED_EDGE('',*,*,#7504,.F.);
#10538=ORIENTED_EDGE('',*,*,#7459,.T.);
#10539=ORIENTED_EDGE('',*,*,#7501,.F.);
#10540=ORIENTED_EDGE('',*,*,#7499,.F.);
#10541=ORIENTED_EDGE('',*,*,#7490,.T.);
#10542=ORIENTED_EDGE('',*,*,#7489,.F.);
#10543=ORIENTED_EDGE('',*,*,#7492,.F.);
#10544=ORIENTED_EDGE('',*,*,#7488,.T.);
#10545=ORIENTED_EDGE('',*,*,#7505,.T.);
#10546=ORIENTED_EDGE('',*,*,#7481,.T.);
#10547=ORIENTED_EDGE('',*,*,#7506,.T.);
#10548=ORIENTED_EDGE('',*,*,#7486,.T.);
#10549=ORIENTED_EDGE('',*,*,#7483,.F.);
#10550=ORIENTED_EDGE('',*,*,#7507,.F.);
#10551=ORIENTED_EDGE('',*,*,#7484,.F.);
#10552=ORIENTED_EDGE('',*,*,#7477,.F.);
#10553=ORIENTED_EDGE('',*,*,#7508,.F.);
#10554=ORIENTED_EDGE('',*,*,#7479,.F.);
#10555=ORIENTED_EDGE('',*,*,#7480,.F.);
#10556=ORIENTED_EDGE('',*,*,#7508,.T.);
#10557=ORIENTED_EDGE('',*,*,#7487,.F.);
#10558=ORIENTED_EDGE('',*,*,#7506,.F.);
#10559=ORIENTED_EDGE('',*,*,#7482,.F.);
#10560=ORIENTED_EDGE('',*,*,#7505,.F.);
#10561=ORIENTED_EDGE('',*,*,#7485,.F.);
#10562=ORIENTED_EDGE('',*,*,#7507,.T.);
#10563=ORIENTED_EDGE('',*,*,#7455,.F.);
#10564=ORIENTED_EDGE('',*,*,#7475,.T.);
#10565=ORIENTED_EDGE('',*,*,#7453,.T.);
#10566=ORIENTED_EDGE('',*,*,#7476,.F.);
#10567=ORIENTED_EDGE('',*,*,#7434,.F.);
#10568=ORIENTED_EDGE('',*,*,#7509,.F.);
#10569=ORIENTED_EDGE('',*,*,#7462,.F.);
#10570=ORIENTED_EDGE('',*,*,#7510,.F.);
#10571=ORIENTED_EDGE('',*,*,#7511,.T.);
#10572=ORIENTED_EDGE('',*,*,#7432,.T.);
#10573=ORIENTED_EDGE('',*,*,#7512,.T.);
#10574=ORIENTED_EDGE('',*,*,#7460,.T.);
#10575=ORIENTED_EDGE('',*,*,#7435,.F.);
#10576=ORIENTED_EDGE('',*,*,#7510,.T.);
#10577=ORIENTED_EDGE('',*,*,#7461,.F.);
#10578=ORIENTED_EDGE('',*,*,#7512,.F.);
#10579=ORIENTED_EDGE('',*,*,#7433,.F.);
#10580=ORIENTED_EDGE('',*,*,#7511,.F.);
#10581=ORIENTED_EDGE('',*,*,#7463,.F.);
#10582=ORIENTED_EDGE('',*,*,#7509,.T.);
#10583=ORIENTED_EDGE('',*,*,#7445,.F.);
#10584=ORIENTED_EDGE('',*,*,#7513,.F.);
#10585=ORIENTED_EDGE('',*,*,#7448,.F.);
#10586=ORIENTED_EDGE('',*,*,#7514,.T.);
#10587=ORIENTED_EDGE('',*,*,#7443,.F.);
#10588=ORIENTED_EDGE('',*,*,#7515,.T.);
#10589=ORIENTED_EDGE('',*,*,#7450,.F.);
#10590=ORIENTED_EDGE('',*,*,#7516,.F.);
#10591=ORIENTED_EDGE('',*,*,#7446,.F.);
#10592=ORIENTED_EDGE('',*,*,#7514,.F.);
#10593=ORIENTED_EDGE('',*,*,#7447,.F.);
#10594=ORIENTED_EDGE('',*,*,#7440,.F.);
#10595=ORIENTED_EDGE('',*,*,#7515,.F.);
#10596=ORIENTED_EDGE('',*,*,#7442,.F.);
#10597=ORIENTED_EDGE('',*,*,#7513,.T.);
#10598=ORIENTED_EDGE('',*,*,#7444,.T.);
#10599=ORIENTED_EDGE('',*,*,#7516,.T.);
#10600=ORIENTED_EDGE('',*,*,#7449,.T.);
#10601=ORIENTED_EDGE('',*,*,#7431,.F.);
#10602=ORIENTED_EDGE('',*,*,#7451,.T.);
#10603=ORIENTED_EDGE('',*,*,#7429,.T.);
#10604=ORIENTED_EDGE('',*,*,#7452,.F.);
#10605=ORIENTED_EDGE('',*,*,#7410,.F.);
#10606=ORIENTED_EDGE('',*,*,#7517,.F.);
#10607=ORIENTED_EDGE('',*,*,#7438,.F.);
#10608=ORIENTED_EDGE('',*,*,#7518,.F.);
#10609=ORIENTED_EDGE('',*,*,#7519,.T.);
#10610=ORIENTED_EDGE('',*,*,#7408,.T.);
#10611=ORIENTED_EDGE('',*,*,#7520,.T.);
#10612=ORIENTED_EDGE('',*,*,#7436,.T.);
#10613=ORIENTED_EDGE('',*,*,#7411,.F.);
#10614=ORIENTED_EDGE('',*,*,#7518,.T.);
#10615=ORIENTED_EDGE('',*,*,#7437,.F.);
#10616=ORIENTED_EDGE('',*,*,#7520,.F.);
#10617=ORIENTED_EDGE('',*,*,#7409,.F.);
#10618=ORIENTED_EDGE('',*,*,#7519,.F.);
#10619=ORIENTED_EDGE('',*,*,#7439,.F.);
#10620=ORIENTED_EDGE('',*,*,#7517,.T.);
#10621=ORIENTED_EDGE('',*,*,#7421,.F.);
#10622=ORIENTED_EDGE('',*,*,#7521,.F.);
#10623=ORIENTED_EDGE('',*,*,#7424,.F.);
#10624=ORIENTED_EDGE('',*,*,#7522,.T.);
#10625=ORIENTED_EDGE('',*,*,#7419,.F.);
#10626=ORIENTED_EDGE('',*,*,#7523,.T.);
#10627=ORIENTED_EDGE('',*,*,#7426,.F.);
#10628=ORIENTED_EDGE('',*,*,#7524,.F.);
#10629=ORIENTED_EDGE('',*,*,#7422,.F.);
#10630=ORIENTED_EDGE('',*,*,#7522,.F.);
#10631=ORIENTED_EDGE('',*,*,#7423,.F.);
#10632=ORIENTED_EDGE('',*,*,#7416,.F.);
#10633=ORIENTED_EDGE('',*,*,#7523,.F.);
#10634=ORIENTED_EDGE('',*,*,#7418,.F.);
#10635=ORIENTED_EDGE('',*,*,#7521,.T.);
#10636=ORIENTED_EDGE('',*,*,#7420,.T.);
#10637=ORIENTED_EDGE('',*,*,#7524,.T.);
#10638=ORIENTED_EDGE('',*,*,#7425,.T.);
#10639=ORIENTED_EDGE('',*,*,#7407,.F.);
#10640=ORIENTED_EDGE('',*,*,#7427,.T.);
#10641=ORIENTED_EDGE('',*,*,#7405,.T.);
#10642=ORIENTED_EDGE('',*,*,#7428,.F.);
#10643=ORIENTED_EDGE('',*,*,#7386,.F.);
#10644=ORIENTED_EDGE('',*,*,#7525,.F.);
#10645=ORIENTED_EDGE('',*,*,#7414,.F.);
#10646=ORIENTED_EDGE('',*,*,#7526,.F.);
#10647=ORIENTED_EDGE('',*,*,#7527,.T.);
#10648=ORIENTED_EDGE('',*,*,#7384,.T.);
#10649=ORIENTED_EDGE('',*,*,#7528,.T.);
#10650=ORIENTED_EDGE('',*,*,#7412,.T.);
#10651=ORIENTED_EDGE('',*,*,#7387,.F.);
#10652=ORIENTED_EDGE('',*,*,#7526,.T.);
#10653=ORIENTED_EDGE('',*,*,#7413,.F.);
#10654=ORIENTED_EDGE('',*,*,#7528,.F.);
#10655=ORIENTED_EDGE('',*,*,#7385,.F.);
#10656=ORIENTED_EDGE('',*,*,#7527,.F.);
#10657=ORIENTED_EDGE('',*,*,#7415,.F.);
#10658=ORIENTED_EDGE('',*,*,#7525,.T.);
#10659=ORIENTED_EDGE('',*,*,#7397,.F.);
#10660=ORIENTED_EDGE('',*,*,#7529,.F.);
#10661=ORIENTED_EDGE('',*,*,#7400,.F.);
#10662=ORIENTED_EDGE('',*,*,#7530,.T.);
#10663=ORIENTED_EDGE('',*,*,#7395,.F.);
#10664=ORIENTED_EDGE('',*,*,#7531,.T.);
#10665=ORIENTED_EDGE('',*,*,#7402,.F.);
#10666=ORIENTED_EDGE('',*,*,#7532,.F.);
#10667=ORIENTED_EDGE('',*,*,#7398,.F.);
#10668=ORIENTED_EDGE('',*,*,#7530,.F.);
#10669=ORIENTED_EDGE('',*,*,#7399,.F.);
#10670=ORIENTED_EDGE('',*,*,#7392,.F.);
#10671=ORIENTED_EDGE('',*,*,#7531,.F.);
#10672=ORIENTED_EDGE('',*,*,#7394,.F.);
#10673=ORIENTED_EDGE('',*,*,#7529,.T.);
#10674=ORIENTED_EDGE('',*,*,#7396,.T.);
#10675=ORIENTED_EDGE('',*,*,#7532,.T.);
#10676=ORIENTED_EDGE('',*,*,#7401,.T.);
#10677=ORIENTED_EDGE('',*,*,#7383,.F.);
#10678=ORIENTED_EDGE('',*,*,#7403,.T.);
#10679=ORIENTED_EDGE('',*,*,#7381,.T.);
#10680=ORIENTED_EDGE('',*,*,#7404,.F.);
#10681=ORIENTED_EDGE('',*,*,#7362,.F.);
#10682=ORIENTED_EDGE('',*,*,#7533,.F.);
#10683=ORIENTED_EDGE('',*,*,#7390,.F.);
#10684=ORIENTED_EDGE('',*,*,#7534,.F.);
#10685=ORIENTED_EDGE('',*,*,#7535,.T.);
#10686=ORIENTED_EDGE('',*,*,#7360,.T.);
#10687=ORIENTED_EDGE('',*,*,#7536,.T.);
#10688=ORIENTED_EDGE('',*,*,#7388,.T.);
#10689=ORIENTED_EDGE('',*,*,#7363,.F.);
#10690=ORIENTED_EDGE('',*,*,#7534,.T.);
#10691=ORIENTED_EDGE('',*,*,#7389,.F.);
#10692=ORIENTED_EDGE('',*,*,#7536,.F.);
#10693=ORIENTED_EDGE('',*,*,#7361,.F.);
#10694=ORIENTED_EDGE('',*,*,#7535,.F.);
#10695=ORIENTED_EDGE('',*,*,#7391,.F.);
#10696=ORIENTED_EDGE('',*,*,#7533,.T.);
#10697=ORIENTED_EDGE('',*,*,#7373,.F.);
#10698=ORIENTED_EDGE('',*,*,#7537,.F.);
#10699=ORIENTED_EDGE('',*,*,#7376,.F.);
#10700=ORIENTED_EDGE('',*,*,#7538,.T.);
#10701=ORIENTED_EDGE('',*,*,#7371,.F.);
#10702=ORIENTED_EDGE('',*,*,#7539,.T.);
#10703=ORIENTED_EDGE('',*,*,#7378,.F.);
#10704=ORIENTED_EDGE('',*,*,#7540,.F.);
#10705=ORIENTED_EDGE('',*,*,#7374,.F.);
#10706=ORIENTED_EDGE('',*,*,#7538,.F.);
#10707=ORIENTED_EDGE('',*,*,#7375,.F.);
#10708=ORIENTED_EDGE('',*,*,#7368,.F.);
#10709=ORIENTED_EDGE('',*,*,#7539,.F.);
#10710=ORIENTED_EDGE('',*,*,#7370,.F.);
#10711=ORIENTED_EDGE('',*,*,#7537,.T.);
#10712=ORIENTED_EDGE('',*,*,#7372,.T.);
#10713=ORIENTED_EDGE('',*,*,#7540,.T.);
#10714=ORIENTED_EDGE('',*,*,#7377,.T.);
#10715=ORIENTED_EDGE('',*,*,#7359,.F.);
#10716=ORIENTED_EDGE('',*,*,#7379,.T.);
#10717=ORIENTED_EDGE('',*,*,#7357,.T.);
#10718=ORIENTED_EDGE('',*,*,#7380,.F.);
#10719=ORIENTED_EDGE('',*,*,#7338,.F.);
#10720=ORIENTED_EDGE('',*,*,#7541,.F.);
#10721=ORIENTED_EDGE('',*,*,#7366,.F.);
#10722=ORIENTED_EDGE('',*,*,#7542,.F.);
#10723=ORIENTED_EDGE('',*,*,#7543,.T.);
#10724=ORIENTED_EDGE('',*,*,#7336,.T.);
#10725=ORIENTED_EDGE('',*,*,#7544,.T.);
#10726=ORIENTED_EDGE('',*,*,#7364,.T.);
#10727=ORIENTED_EDGE('',*,*,#7339,.F.);
#10728=ORIENTED_EDGE('',*,*,#7542,.T.);
#10729=ORIENTED_EDGE('',*,*,#7365,.F.);
#10730=ORIENTED_EDGE('',*,*,#7544,.F.);
#10731=ORIENTED_EDGE('',*,*,#7337,.F.);
#10732=ORIENTED_EDGE('',*,*,#7543,.F.);
#10733=ORIENTED_EDGE('',*,*,#7367,.F.);
#10734=ORIENTED_EDGE('',*,*,#7541,.T.);
#10735=ORIENTED_EDGE('',*,*,#7349,.F.);
#10736=ORIENTED_EDGE('',*,*,#7545,.F.);
#10737=ORIENTED_EDGE('',*,*,#7352,.F.);
#10738=ORIENTED_EDGE('',*,*,#7546,.T.);
#10739=ORIENTED_EDGE('',*,*,#7347,.F.);
#10740=ORIENTED_EDGE('',*,*,#7547,.T.);
#10741=ORIENTED_EDGE('',*,*,#7354,.F.);
#10742=ORIENTED_EDGE('',*,*,#7548,.F.);
#10743=ORIENTED_EDGE('',*,*,#7350,.F.);
#10744=ORIENTED_EDGE('',*,*,#7546,.F.);
#10745=ORIENTED_EDGE('',*,*,#7351,.F.);
#10746=ORIENTED_EDGE('',*,*,#7344,.F.);
#10747=ORIENTED_EDGE('',*,*,#7547,.F.);
#10748=ORIENTED_EDGE('',*,*,#7346,.F.);
#10749=ORIENTED_EDGE('',*,*,#7545,.T.);
#10750=ORIENTED_EDGE('',*,*,#7348,.T.);
#10751=ORIENTED_EDGE('',*,*,#7548,.T.);
#10752=ORIENTED_EDGE('',*,*,#7353,.T.);
#10753=ORIENTED_EDGE('',*,*,#7335,.F.);
#10754=ORIENTED_EDGE('',*,*,#7355,.T.);
#10755=ORIENTED_EDGE('',*,*,#7333,.T.);
#10756=ORIENTED_EDGE('',*,*,#7356,.F.);
#10757=ORIENTED_EDGE('',*,*,#7495,.F.);
#10758=ORIENTED_EDGE('',*,*,#7549,.F.);
#10759=ORIENTED_EDGE('',*,*,#7342,.F.);
#10760=ORIENTED_EDGE('',*,*,#7550,.F.);
#10761=ORIENTED_EDGE('',*,*,#7551,.T.);
#10762=ORIENTED_EDGE('',*,*,#7493,.T.);
#10763=ORIENTED_EDGE('',*,*,#7552,.T.);
#10764=ORIENTED_EDGE('',*,*,#7340,.T.);
#10765=ORIENTED_EDGE('',*,*,#7496,.F.);
#10766=ORIENTED_EDGE('',*,*,#7550,.T.);
#10767=ORIENTED_EDGE('',*,*,#7341,.F.);
#10768=ORIENTED_EDGE('',*,*,#7552,.F.);
#10769=ORIENTED_EDGE('',*,*,#7494,.F.);
#10770=ORIENTED_EDGE('',*,*,#7551,.F.);
#10771=ORIENTED_EDGE('',*,*,#7343,.F.);
#10772=ORIENTED_EDGE('',*,*,#7549,.T.);
#10773=ORIENTED_EDGE('',*,*,#7466,.F.);
#10774=ORIENTED_EDGE('',*,*,#7553,.T.);
#10775=ORIENTED_EDGE('',*,*,#7472,.T.);
#10776=ORIENTED_EDGE('',*,*,#7554,.T.);
#10777=ORIENTED_EDGE('',*,*,#7555,.F.);
#10778=ORIENTED_EDGE('',*,*,#7464,.T.);
#10779=ORIENTED_EDGE('',*,*,#7468,.T.);
#10780=ORIENTED_EDGE('',*,*,#7556,.F.);
#10781=ORIENTED_EDGE('',*,*,#7470,.F.);
#10782=ORIENTED_EDGE('',*,*,#7474,.F.);
#10783=ORIENTED_EDGE('',*,*,#7556,.T.);
#10784=ORIENTED_EDGE('',*,*,#7467,.T.);
#10785=ORIENTED_EDGE('',*,*,#7554,.F.);
#10786=ORIENTED_EDGE('',*,*,#7471,.F.);
#10787=ORIENTED_EDGE('',*,*,#7553,.F.);
#10788=ORIENTED_EDGE('',*,*,#7465,.T.);
#10789=ORIENTED_EDGE('',*,*,#7555,.T.);
#10790=ORIENTED_EDGE('',*,*,#7473,.F.);
#10791=ORIENTED_EDGE('',*,*,#7557,.T.);
#10792=ORIENTED_EDGE('',*,*,#7558,.T.);
#10793=ORIENTED_EDGE('',*,*,#7559,.F.);
#10794=ORIENTED_EDGE('',*,*,#7558,.F.);
#10795=ORIENTED_EDGE('',*,*,#7560,.T.);
#10796=ORIENTED_EDGE('',*,*,#7561,.T.);
#10797=ORIENTED_EDGE('',*,*,#7562,.T.);
#10798=ORIENTED_EDGE('',*,*,#7563,.T.);
#10799=ORIENTED_EDGE('',*,*,#7561,.F.);
#10800=ORIENTED_EDGE('',*,*,#7564,.T.);
#10801=ORIENTED_EDGE('',*,*,#7565,.T.);
#10802=ORIENTED_EDGE('',*,*,#7566,.T.);
#10803=ORIENTED_EDGE('',*,*,#7567,.T.);
#10804=ORIENTED_EDGE('',*,*,#7566,.F.);
#10805=ORIENTED_EDGE('',*,*,#7568,.T.);
#10806=ORIENTED_EDGE('',*,*,#7560,.F.);
#10807=ORIENTED_EDGE('',*,*,#7569,.T.);
#10808=ORIENTED_EDGE('',*,*,#7570,.F.);
#10809=ORIENTED_EDGE('',*,*,#7569,.F.);
#10810=ORIENTED_EDGE('',*,*,#7564,.F.);
#10811=ORIENTED_EDGE('',*,*,#7563,.F.);
#10812=ORIENTED_EDGE('',*,*,#7571,.T.);
#10813=ORIENTED_EDGE('',*,*,#7568,.F.);
#10814=ORIENTED_EDGE('',*,*,#7565,.F.);
#10815=ORIENTED_EDGE('',*,*,#7571,.F.);
#10816=ORIENTED_EDGE('',*,*,#7562,.F.);
#10817=ORIENTED_EDGE('',*,*,#7567,.F.);
#10818=ORIENTED_EDGE('',*,*,#7572,.T.);
#10819=ORIENTED_EDGE('',*,*,#7573,.T.);
#10820=ORIENTED_EDGE('',*,*,#7572,.F.);
#10821=ORIENTED_EDGE('',*,*,#7574,.F.);
#10822=ORIENTED_EDGE('',*,*,#7575,.T.);
#10823=ORIENTED_EDGE('',*,*,#7559,.T.);
#10824=ORIENTED_EDGE('',*,*,#7575,.F.);
#10825=ORIENTED_EDGE('',*,*,#7557,.F.);
#10826=ORIENTED_EDGE('',*,*,#7576,.T.);
#10827=ORIENTED_EDGE('',*,*,#7577,.T.);
#10828=ORIENTED_EDGE('',*,*,#7576,.F.);
#10829=ORIENTED_EDGE('',*,*,#7577,.F.);
#10830=ORIENTED_EDGE('',*,*,#7570,.T.);
#10831=ORIENTED_EDGE('',*,*,#7574,.T.);
#10832=ORIENTED_EDGE('',*,*,#7573,.F.);
#10833=ORIENTED_EDGE('',*,*,#7578,.T.);
#10834=ORIENTED_EDGE('',*,*,#7578,.F.);
#10835=ORIENTED_EDGE('',*,*,#7579,.T.);
#10836=ORIENTED_EDGE('',*,*,#7579,.F.);
#10837=ORIENTED_EDGE('',*,*,#7580,.T.);
#10838=ORIENTED_EDGE('',*,*,#7580,.F.);
#10839=ORIENTED_EDGE('',*,*,#7581,.T.);
#10840=ORIENTED_EDGE('',*,*,#7581,.F.);
#10841=ORIENTED_EDGE('',*,*,#7582,.T.);
#10842=ORIENTED_EDGE('',*,*,#7582,.F.);
#10843=ORIENTED_EDGE('',*,*,#7583,.T.);
#10844=ORIENTED_EDGE('',*,*,#7583,.F.);
#10845=ORIENTED_EDGE('',*,*,#7584,.T.);
#10846=ORIENTED_EDGE('',*,*,#7584,.F.);
#10847=ORIENTED_EDGE('',*,*,#7585,.T.);
#10848=ORIENTED_EDGE('',*,*,#7586,.T.);
#10849=ORIENTED_EDGE('',*,*,#7587,.T.);
#10850=ORIENTED_EDGE('',*,*,#7588,.T.);
#10851=ORIENTED_EDGE('',*,*,#7586,.F.);
#10852=ORIENTED_EDGE('',*,*,#7589,.T.);
#10853=ORIENTED_EDGE('',*,*,#7590,.T.);
#10854=ORIENTED_EDGE('',*,*,#7591,.T.);
#10855=ORIENTED_EDGE('',*,*,#7590,.F.);
#10856=ORIENTED_EDGE('',*,*,#7592,.T.);
#10857=ORIENTED_EDGE('',*,*,#7593,.T.);
#10858=ORIENTED_EDGE('',*,*,#7594,.T.);
#10859=ORIENTED_EDGE('',*,*,#7593,.F.);
#10860=ORIENTED_EDGE('',*,*,#7595,.T.);
#10861=ORIENTED_EDGE('',*,*,#7596,.T.);
#10862=ORIENTED_EDGE('',*,*,#7597,.T.);
#10863=ORIENTED_EDGE('',*,*,#7596,.F.);
#10864=ORIENTED_EDGE('',*,*,#7598,.T.);
#10865=ORIENTED_EDGE('',*,*,#7599,.F.);
#10866=ORIENTED_EDGE('',*,*,#7600,.T.);
#10867=ORIENTED_EDGE('',*,*,#7601,.T.);
#10868=ORIENTED_EDGE('',*,*,#7600,.F.);
#10869=ORIENTED_EDGE('',*,*,#7588,.F.);
#10870=ORIENTED_EDGE('',*,*,#7602,.T.);
#10871=ORIENTED_EDGE('',*,*,#7603,.T.);
#10872=ORIENTED_EDGE('',*,*,#7602,.F.);
#10873=ORIENTED_EDGE('',*,*,#7587,.F.);
#10874=ORIENTED_EDGE('',*,*,#7604,.F.);
#10875=ORIENTED_EDGE('',*,*,#7605,.T.);
#10876=ORIENTED_EDGE('',*,*,#7598,.F.);
#10877=ORIENTED_EDGE('',*,*,#7595,.F.);
#10878=ORIENTED_EDGE('',*,*,#7605,.F.);
#10879=ORIENTED_EDGE('',*,*,#7604,.T.);
#10880=ORIENTED_EDGE('',*,*,#7606,.T.);
#10881=ORIENTED_EDGE('',*,*,#7607,.F.);
#10882=ORIENTED_EDGE('',*,*,#7606,.F.);
#10883=ORIENTED_EDGE('',*,*,#7589,.F.);
#10884=ORIENTED_EDGE('',*,*,#7608,.T.);
#10885=ORIENTED_EDGE('',*,*,#7607,.T.);
#10886=ORIENTED_EDGE('',*,*,#7608,.F.);
#10887=ORIENTED_EDGE('',*,*,#7609,.F.);
#10888=ORIENTED_EDGE('',*,*,#7610,.T.);
#10889=ORIENTED_EDGE('',*,*,#7594,.F.);
#10890=ORIENTED_EDGE('',*,*,#7610,.F.);
#10891=ORIENTED_EDGE('',*,*,#7611,.F.);
#10892=ORIENTED_EDGE('',*,*,#7612,.T.);
#10893=ORIENTED_EDGE('',*,*,#7613,.T.);
#10894=ORIENTED_EDGE('',*,*,#7612,.F.);
#10895=ORIENTED_EDGE('',*,*,#7614,.T.);
#10896=ORIENTED_EDGE('',*,*,#7615,.T.);
#10897=ORIENTED_EDGE('',*,*,#7616,.F.);
#10898=ORIENTED_EDGE('',*,*,#7615,.F.);
#10899=ORIENTED_EDGE('',*,*,#7617,.F.);
#10900=ORIENTED_EDGE('',*,*,#7618,.F.);
#10901=ORIENTED_EDGE('',*,*,#7619,.T.);
#10902=ORIENTED_EDGE('',*,*,#7620,.T.);
#10903=ORIENTED_EDGE('',*,*,#7619,.F.);
#10904=ORIENTED_EDGE('',*,*,#7614,.F.);
#10905=ORIENTED_EDGE('',*,*,#7621,.T.);
#10906=ORIENTED_EDGE('',*,*,#7617,.T.);
#10907=ORIENTED_EDGE('',*,*,#7618,.T.);
#10908=ORIENTED_EDGE('',*,*,#7621,.F.);
#10909=ORIENTED_EDGE('',*,*,#7620,.F.);
#10910=ORIENTED_EDGE('',*,*,#7585,.F.);
#10911=ORIENTED_EDGE('',*,*,#7616,.T.);
#10912=ORIENTED_EDGE('',*,*,#7592,.F.);
#10913=ORIENTED_EDGE('',*,*,#7611,.T.);
#10914=ORIENTED_EDGE('',*,*,#7597,.F.);
#10915=ORIENTED_EDGE('',*,*,#7613,.F.);
#10916=ORIENTED_EDGE('',*,*,#7609,.T.);
#10917=ORIENTED_EDGE('',*,*,#7599,.T.);
#10918=ORIENTED_EDGE('',*,*,#7603,.F.);
#10919=ORIENTED_EDGE('',*,*,#7601,.F.);
#10920=ORIENTED_EDGE('',*,*,#7591,.F.);
#10921=ORIENTED_EDGE('',*,*,#7622,.T.);
#10922=ORIENTED_EDGE('',*,*,#7623,.T.);
#10923=ORIENTED_EDGE('',*,*,#7624,.F.);
#10924=ORIENTED_EDGE('',*,*,#7623,.F.);
#10925=ORIENTED_EDGE('',*,*,#7625,.T.);
#10926=ORIENTED_EDGE('',*,*,#7626,.F.);
#10927=ORIENTED_EDGE('',*,*,#7627,.F.);
#10928=ORIENTED_EDGE('',*,*,#7628,.F.);
#10929=ORIENTED_EDGE('',*,*,#7629,.T.);
#10930=ORIENTED_EDGE('',*,*,#7630,.F.);
#10931=ORIENTED_EDGE('',*,*,#7631,.F.);
#10932=ORIENTED_EDGE('',*,*,#7632,.F.);
#10933=ORIENTED_EDGE('',*,*,#7633,.F.);
#10934=ORIENTED_EDGE('',*,*,#7634,.F.);
#10935=ORIENTED_EDGE('',*,*,#7635,.T.);
#10936=ORIENTED_EDGE('',*,*,#7636,.F.);
#10937=ORIENTED_EDGE('',*,*,#7637,.F.);
#10938=ORIENTED_EDGE('',*,*,#7638,.T.);
#10939=ORIENTED_EDGE('',*,*,#7639,.F.);
#10940=ORIENTED_EDGE('',*,*,#7640,.F.);
#10941=ORIENTED_EDGE('',*,*,#7641,.T.);
#10942=ORIENTED_EDGE('',*,*,#7642,.F.);
#10943=ORIENTED_EDGE('',*,*,#7643,.F.);
#10944=ORIENTED_EDGE('',*,*,#7638,.F.);
#10945=ORIENTED_EDGE('',*,*,#7644,.T.);
#10946=ORIENTED_EDGE('',*,*,#7645,.F.);
#10947=ORIENTED_EDGE('',*,*,#7646,.T.);
#10948=ORIENTED_EDGE('',*,*,#7647,.T.);
#10949=ORIENTED_EDGE('',*,*,#7648,.F.);
#10950=ORIENTED_EDGE('',*,*,#7647,.F.);
#10951=ORIENTED_EDGE('',*,*,#7649,.T.);
#10952=ORIENTED_EDGE('',*,*,#7650,.F.);
#10953=ORIENTED_EDGE('',*,*,#7651,.F.);
#10954=ORIENTED_EDGE('',*,*,#7652,.F.);
#10955=ORIENTED_EDGE('',*,*,#7653,.T.);
#10956=ORIENTED_EDGE('',*,*,#7654,.F.);
#10957=ORIENTED_EDGE('',*,*,#7655,.F.);
#10958=ORIENTED_EDGE('',*,*,#7656,.F.);
#10959=ORIENTED_EDGE('',*,*,#7657,.F.);
#10960=ORIENTED_EDGE('',*,*,#7658,.F.);
#10961=ORIENTED_EDGE('',*,*,#7659,.T.);
#10962=ORIENTED_EDGE('',*,*,#7660,.F.);
#10963=ORIENTED_EDGE('',*,*,#7661,.F.);
#10964=ORIENTED_EDGE('',*,*,#7662,.T.);
#10965=ORIENTED_EDGE('',*,*,#7663,.F.);
#10966=ORIENTED_EDGE('',*,*,#7664,.F.);
#10967=ORIENTED_EDGE('',*,*,#7665,.T.);
#10968=ORIENTED_EDGE('',*,*,#7666,.F.);
#10969=ORIENTED_EDGE('',*,*,#7667,.F.);
#10970=ORIENTED_EDGE('',*,*,#7662,.F.);
#10971=ORIENTED_EDGE('',*,*,#7668,.T.);
#10972=ORIENTED_EDGE('',*,*,#7669,.F.);
#10973=ORIENTED_EDGE('',*,*,#7670,.T.);
#10974=ORIENTED_EDGE('',*,*,#7671,.T.);
#10975=ORIENTED_EDGE('',*,*,#7672,.F.);
#10976=ORIENTED_EDGE('',*,*,#7671,.F.);
#10977=ORIENTED_EDGE('',*,*,#7673,.T.);
#10978=ORIENTED_EDGE('',*,*,#7674,.F.);
#10979=ORIENTED_EDGE('',*,*,#7675,.F.);
#10980=ORIENTED_EDGE('',*,*,#7676,.F.);
#10981=ORIENTED_EDGE('',*,*,#7677,.T.);
#10982=ORIENTED_EDGE('',*,*,#7678,.F.);
#10983=ORIENTED_EDGE('',*,*,#7679,.F.);
#10984=ORIENTED_EDGE('',*,*,#7680,.F.);
#10985=ORIENTED_EDGE('',*,*,#7681,.F.);
#10986=ORIENTED_EDGE('',*,*,#7682,.F.);
#10987=ORIENTED_EDGE('',*,*,#7683,.T.);
#10988=ORIENTED_EDGE('',*,*,#7684,.F.);
#10989=ORIENTED_EDGE('',*,*,#7685,.F.);
#10990=ORIENTED_EDGE('',*,*,#7686,.T.);
#10991=ORIENTED_EDGE('',*,*,#7687,.F.);
#10992=ORIENTED_EDGE('',*,*,#7688,.F.);
#10993=ORIENTED_EDGE('',*,*,#7689,.T.);
#10994=ORIENTED_EDGE('',*,*,#7690,.F.);
#10995=ORIENTED_EDGE('',*,*,#7691,.F.);
#10996=ORIENTED_EDGE('',*,*,#7686,.F.);
#10997=ORIENTED_EDGE('',*,*,#7692,.T.);
#10998=ORIENTED_EDGE('',*,*,#7693,.F.);
#10999=ORIENTED_EDGE('',*,*,#7694,.T.);
#11000=ORIENTED_EDGE('',*,*,#7695,.T.);
#11001=ORIENTED_EDGE('',*,*,#7696,.F.);
#11002=ORIENTED_EDGE('',*,*,#7695,.F.);
#11003=ORIENTED_EDGE('',*,*,#7697,.T.);
#11004=ORIENTED_EDGE('',*,*,#7698,.F.);
#11005=ORIENTED_EDGE('',*,*,#7699,.F.);
#11006=ORIENTED_EDGE('',*,*,#7700,.F.);
#11007=ORIENTED_EDGE('',*,*,#7701,.T.);
#11008=ORIENTED_EDGE('',*,*,#7702,.F.);
#11009=ORIENTED_EDGE('',*,*,#7703,.F.);
#11010=ORIENTED_EDGE('',*,*,#7704,.F.);
#11011=ORIENTED_EDGE('',*,*,#7705,.F.);
#11012=ORIENTED_EDGE('',*,*,#7706,.F.);
#11013=ORIENTED_EDGE('',*,*,#7707,.T.);
#11014=ORIENTED_EDGE('',*,*,#7708,.F.);
#11015=ORIENTED_EDGE('',*,*,#7709,.F.);
#11016=ORIENTED_EDGE('',*,*,#7710,.T.);
#11017=ORIENTED_EDGE('',*,*,#7711,.F.);
#11018=ORIENTED_EDGE('',*,*,#7712,.F.);
#11019=ORIENTED_EDGE('',*,*,#7713,.T.);
#11020=ORIENTED_EDGE('',*,*,#7714,.F.);
#11021=ORIENTED_EDGE('',*,*,#7715,.F.);
#11022=ORIENTED_EDGE('',*,*,#7710,.F.);
#11023=ORIENTED_EDGE('',*,*,#7716,.T.);
#11024=ORIENTED_EDGE('',*,*,#7717,.F.);
#11025=ORIENTED_EDGE('',*,*,#7718,.T.);
#11026=ORIENTED_EDGE('',*,*,#7719,.T.);
#11027=ORIENTED_EDGE('',*,*,#7720,.F.);
#11028=ORIENTED_EDGE('',*,*,#7719,.F.);
#11029=ORIENTED_EDGE('',*,*,#7721,.T.);
#11030=ORIENTED_EDGE('',*,*,#7722,.F.);
#11031=ORIENTED_EDGE('',*,*,#7723,.F.);
#11032=ORIENTED_EDGE('',*,*,#7724,.F.);
#11033=ORIENTED_EDGE('',*,*,#7725,.T.);
#11034=ORIENTED_EDGE('',*,*,#7726,.F.);
#11035=ORIENTED_EDGE('',*,*,#7727,.F.);
#11036=ORIENTED_EDGE('',*,*,#7728,.F.);
#11037=ORIENTED_EDGE('',*,*,#7729,.F.);
#11038=ORIENTED_EDGE('',*,*,#7730,.F.);
#11039=ORIENTED_EDGE('',*,*,#7731,.T.);
#11040=ORIENTED_EDGE('',*,*,#7732,.F.);
#11041=ORIENTED_EDGE('',*,*,#7733,.F.);
#11042=ORIENTED_EDGE('',*,*,#7734,.T.);
#11043=ORIENTED_EDGE('',*,*,#7735,.F.);
#11044=ORIENTED_EDGE('',*,*,#7736,.F.);
#11045=ORIENTED_EDGE('',*,*,#7737,.T.);
#11046=ORIENTED_EDGE('',*,*,#7738,.F.);
#11047=ORIENTED_EDGE('',*,*,#7739,.F.);
#11048=ORIENTED_EDGE('',*,*,#7734,.F.);
#11049=ORIENTED_EDGE('',*,*,#7740,.T.);
#11050=ORIENTED_EDGE('',*,*,#7741,.F.);
#11051=ORIENTED_EDGE('',*,*,#7742,.T.);
#11052=ORIENTED_EDGE('',*,*,#7743,.T.);
#11053=ORIENTED_EDGE('',*,*,#7744,.F.);
#11054=ORIENTED_EDGE('',*,*,#7743,.F.);
#11055=ORIENTED_EDGE('',*,*,#7745,.T.);
#11056=ORIENTED_EDGE('',*,*,#7746,.T.);
#11057=ORIENTED_EDGE('',*,*,#7747,.T.);
#11058=ORIENTED_EDGE('',*,*,#7748,.F.);
#11059=ORIENTED_EDGE('',*,*,#7749,.T.);
#11060=ORIENTED_EDGE('',*,*,#7750,.F.);
#11061=ORIENTED_EDGE('',*,*,#7751,.F.);
#11062=ORIENTED_EDGE('',*,*,#7752,.F.);
#11063=ORIENTED_EDGE('',*,*,#7753,.T.);
#11064=ORIENTED_EDGE('',*,*,#7754,.T.);
#11065=ORIENTED_EDGE('',*,*,#7755,.F.);
#11066=ORIENTED_EDGE('',*,*,#7756,.F.);
#11067=ORIENTED_EDGE('',*,*,#7757,.T.);
#11068=ORIENTED_EDGE('',*,*,#7758,.F.);
#11069=ORIENTED_EDGE('',*,*,#7759,.F.);
#11070=ORIENTED_EDGE('',*,*,#7754,.F.);
#11071=ORIENTED_EDGE('',*,*,#7760,.T.);
#11072=ORIENTED_EDGE('',*,*,#7761,.T.);
#11073=ORIENTED_EDGE('',*,*,#7762,.F.);
#11074=ORIENTED_EDGE('',*,*,#7763,.T.);
#11075=ORIENTED_EDGE('',*,*,#7764,.T.);
#11076=ORIENTED_EDGE('',*,*,#7765,.F.);
#11077=ORIENTED_EDGE('',*,*,#7766,.F.);
#11078=ORIENTED_EDGE('',*,*,#7767,.F.);
#11079=ORIENTED_EDGE('',*,*,#7768,.T.);
#11080=ORIENTED_EDGE('',*,*,#7769,.F.);
#11081=ORIENTED_EDGE('',*,*,#7770,.F.);
#11082=ORIENTED_EDGE('',*,*,#7771,.T.);
#11083=ORIENTED_EDGE('',*,*,#7772,.F.);
#11084=ORIENTED_EDGE('',*,*,#7773,.F.);
#11085=ORIENTED_EDGE('',*,*,#7774,.T.);
#11086=ORIENTED_EDGE('',*,*,#7775,.F.);
#11087=ORIENTED_EDGE('',*,*,#7776,.F.);
#11088=ORIENTED_EDGE('',*,*,#7771,.F.);
#11089=ORIENTED_EDGE('',*,*,#7777,.T.);
#11090=ORIENTED_EDGE('',*,*,#7778,.F.);
#11091=ORIENTED_EDGE('',*,*,#7779,.T.);
#11092=ORIENTED_EDGE('',*,*,#7780,.T.);
#11093=ORIENTED_EDGE('',*,*,#7781,.F.);
#11094=ORIENTED_EDGE('',*,*,#7780,.F.);
#11095=ORIENTED_EDGE('',*,*,#7782,.T.);
#11096=ORIENTED_EDGE('',*,*,#7783,.F.);
#11097=ORIENTED_EDGE('',*,*,#7784,.F.);
#11098=ORIENTED_EDGE('',*,*,#7785,.F.);
#11099=ORIENTED_EDGE('',*,*,#7786,.T.);
#11100=ORIENTED_EDGE('',*,*,#7787,.F.);
#11101=ORIENTED_EDGE('',*,*,#7788,.F.);
#11102=ORIENTED_EDGE('',*,*,#7789,.F.);
#11103=ORIENTED_EDGE('',*,*,#7790,.F.);
#11104=ORIENTED_EDGE('',*,*,#7787,.T.);
#11105=ORIENTED_EDGE('',*,*,#7791,.T.);
#11106=ORIENTED_EDGE('',*,*,#7747,.F.);
#11107=ORIENTED_EDGE('',*,*,#7792,.T.);
#11108=ORIENTED_EDGE('',*,*,#7789,.T.);
#11109=ORIENTED_EDGE('',*,*,#7793,.F.);
#11110=ORIENTED_EDGE('',*,*,#7745,.F.);
#11111=ORIENTED_EDGE('',*,*,#7748,.T.);
#11112=ORIENTED_EDGE('',*,*,#7791,.F.);
#11113=ORIENTED_EDGE('',*,*,#7786,.F.);
#11114=ORIENTED_EDGE('',*,*,#7792,.F.);
#11115=ORIENTED_EDGE('',*,*,#7793,.T.);
#11116=ORIENTED_EDGE('',*,*,#7788,.T.);
#11117=ORIENTED_EDGE('',*,*,#7790,.T.);
#11118=ORIENTED_EDGE('',*,*,#7746,.F.);
#11119=ORIENTED_EDGE('',*,*,#7779,.F.);
#11120=ORIENTED_EDGE('',*,*,#7778,.T.);
#11121=ORIENTED_EDGE('',*,*,#7781,.T.);
#11122=ORIENTED_EDGE('',*,*,#7777,.F.);
#11123=ORIENTED_EDGE('',*,*,#7794,.F.);
#11124=ORIENTED_EDGE('',*,*,#7768,.F.);
#11125=ORIENTED_EDGE('',*,*,#7795,.F.);
#11126=ORIENTED_EDGE('',*,*,#7774,.F.);
#11127=ORIENTED_EDGE('',*,*,#7772,.T.);
#11128=ORIENTED_EDGE('',*,*,#7776,.T.);
#11129=ORIENTED_EDGE('',*,*,#7796,.T.);
#11130=ORIENTED_EDGE('',*,*,#7766,.T.);
#11131=ORIENTED_EDGE('',*,*,#7770,.T.);
#11132=ORIENTED_EDGE('',*,*,#7797,.T.);
#11133=ORIENTED_EDGE('',*,*,#7775,.T.);
#11134=ORIENTED_EDGE('',*,*,#7795,.T.);
#11135=ORIENTED_EDGE('',*,*,#7767,.T.);
#11136=ORIENTED_EDGE('',*,*,#7796,.F.);
#11137=ORIENTED_EDGE('',*,*,#7773,.T.);
#11138=ORIENTED_EDGE('',*,*,#7797,.F.);
#11139=ORIENTED_EDGE('',*,*,#7769,.T.);
#11140=ORIENTED_EDGE('',*,*,#7794,.T.);
#11141=ORIENTED_EDGE('',*,*,#7744,.T.);
#11142=ORIENTED_EDGE('',*,*,#7764,.F.);
#11143=ORIENTED_EDGE('',*,*,#7742,.F.);
#11144=ORIENTED_EDGE('',*,*,#7765,.T.);
#11145=ORIENTED_EDGE('',*,*,#7723,.T.);
#11146=ORIENTED_EDGE('',*,*,#7798,.T.);
#11147=ORIENTED_EDGE('',*,*,#7751,.T.);
#11148=ORIENTED_EDGE('',*,*,#7799,.T.);
#11149=ORIENTED_EDGE('',*,*,#7800,.F.);
#11150=ORIENTED_EDGE('',*,*,#7749,.F.);
#11151=ORIENTED_EDGE('',*,*,#7801,.F.);
#11152=ORIENTED_EDGE('',*,*,#7721,.F.);
#11153=ORIENTED_EDGE('',*,*,#7722,.T.);
#11154=ORIENTED_EDGE('',*,*,#7801,.T.);
#11155=ORIENTED_EDGE('',*,*,#7752,.T.);
#11156=ORIENTED_EDGE('',*,*,#7798,.F.);
#11157=ORIENTED_EDGE('',*,*,#7724,.T.);
#11158=ORIENTED_EDGE('',*,*,#7799,.F.);
#11159=ORIENTED_EDGE('',*,*,#7750,.T.);
#11160=ORIENTED_EDGE('',*,*,#7800,.T.);
#11161=ORIENTED_EDGE('',*,*,#7736,.T.);
#11162=ORIENTED_EDGE('',*,*,#7802,.F.);
#11163=ORIENTED_EDGE('',*,*,#7732,.T.);
#11164=ORIENTED_EDGE('',*,*,#7803,.T.);
#11165=ORIENTED_EDGE('',*,*,#7738,.T.);
#11166=ORIENTED_EDGE('',*,*,#7804,.T.);
#11167=ORIENTED_EDGE('',*,*,#7730,.T.);
#11168=ORIENTED_EDGE('',*,*,#7805,.F.);
#11169=ORIENTED_EDGE('',*,*,#7735,.T.);
#11170=ORIENTED_EDGE('',*,*,#7739,.T.);
#11171=ORIENTED_EDGE('',*,*,#7805,.T.);
#11172=ORIENTED_EDGE('',*,*,#7729,.T.);
#11173=ORIENTED_EDGE('',*,*,#7733,.T.);
#11174=ORIENTED_EDGE('',*,*,#7802,.T.);
#11175=ORIENTED_EDGE('',*,*,#7803,.F.);
#11176=ORIENTED_EDGE('',*,*,#7731,.F.);
#11177=ORIENTED_EDGE('',*,*,#7804,.F.);
#11178=ORIENTED_EDGE('',*,*,#7737,.F.);
#11179=ORIENTED_EDGE('',*,*,#7720,.T.);
#11180=ORIENTED_EDGE('',*,*,#7740,.F.);
#11181=ORIENTED_EDGE('',*,*,#7718,.F.);
#11182=ORIENTED_EDGE('',*,*,#7741,.T.);
#11183=ORIENTED_EDGE('',*,*,#7699,.T.);
#11184=ORIENTED_EDGE('',*,*,#7806,.T.);
#11185=ORIENTED_EDGE('',*,*,#7727,.T.);
#11186=ORIENTED_EDGE('',*,*,#7807,.T.);
#11187=ORIENTED_EDGE('',*,*,#7808,.F.);
#11188=ORIENTED_EDGE('',*,*,#7725,.F.);
#11189=ORIENTED_EDGE('',*,*,#7809,.F.);
#11190=ORIENTED_EDGE('',*,*,#7697,.F.);
#11191=ORIENTED_EDGE('',*,*,#7698,.T.);
#11192=ORIENTED_EDGE('',*,*,#7809,.T.);
#11193=ORIENTED_EDGE('',*,*,#7728,.T.);
#11194=ORIENTED_EDGE('',*,*,#7806,.F.);
#11195=ORIENTED_EDGE('',*,*,#7700,.T.);
#11196=ORIENTED_EDGE('',*,*,#7807,.F.);
#11197=ORIENTED_EDGE('',*,*,#7726,.T.);
#11198=ORIENTED_EDGE('',*,*,#7808,.T.);
#11199=ORIENTED_EDGE('',*,*,#7712,.T.);
#11200=ORIENTED_EDGE('',*,*,#7810,.F.);
#11201=ORIENTED_EDGE('',*,*,#7708,.T.);
#11202=ORIENTED_EDGE('',*,*,#7811,.T.);
#11203=ORIENTED_EDGE('',*,*,#7714,.T.);
#11204=ORIENTED_EDGE('',*,*,#7812,.T.);
#11205=ORIENTED_EDGE('',*,*,#7706,.T.);
#11206=ORIENTED_EDGE('',*,*,#7813,.F.);
#11207=ORIENTED_EDGE('',*,*,#7711,.T.);
#11208=ORIENTED_EDGE('',*,*,#7715,.T.);
#11209=ORIENTED_EDGE('',*,*,#7813,.T.);
#11210=ORIENTED_EDGE('',*,*,#7705,.T.);
#11211=ORIENTED_EDGE('',*,*,#7709,.T.);
#11212=ORIENTED_EDGE('',*,*,#7810,.T.);
#11213=ORIENTED_EDGE('',*,*,#7811,.F.);
#11214=ORIENTED_EDGE('',*,*,#7707,.F.);
#11215=ORIENTED_EDGE('',*,*,#7812,.F.);
#11216=ORIENTED_EDGE('',*,*,#7713,.F.);
#11217=ORIENTED_EDGE('',*,*,#7696,.T.);
#11218=ORIENTED_EDGE('',*,*,#7716,.F.);
#11219=ORIENTED_EDGE('',*,*,#7694,.F.);
#11220=ORIENTED_EDGE('',*,*,#7717,.T.);
#11221=ORIENTED_EDGE('',*,*,#7675,.T.);
#11222=ORIENTED_EDGE('',*,*,#7814,.T.);
#11223=ORIENTED_EDGE('',*,*,#7703,.T.);
#11224=ORIENTED_EDGE('',*,*,#7815,.T.);
#11225=ORIENTED_EDGE('',*,*,#7816,.F.);
#11226=ORIENTED_EDGE('',*,*,#7701,.F.);
#11227=ORIENTED_EDGE('',*,*,#7817,.F.);
#11228=ORIENTED_EDGE('',*,*,#7673,.F.);
#11229=ORIENTED_EDGE('',*,*,#7674,.T.);
#11230=ORIENTED_EDGE('',*,*,#7817,.T.);
#11231=ORIENTED_EDGE('',*,*,#7704,.T.);
#11232=ORIENTED_EDGE('',*,*,#7814,.F.);
#11233=ORIENTED_EDGE('',*,*,#7676,.T.);
#11234=ORIENTED_EDGE('',*,*,#7815,.F.);
#11235=ORIENTED_EDGE('',*,*,#7702,.T.);
#11236=ORIENTED_EDGE('',*,*,#7816,.T.);
#11237=ORIENTED_EDGE('',*,*,#7688,.T.);
#11238=ORIENTED_EDGE('',*,*,#7818,.F.);
#11239=ORIENTED_EDGE('',*,*,#7684,.T.);
#11240=ORIENTED_EDGE('',*,*,#7819,.T.);
#11241=ORIENTED_EDGE('',*,*,#7690,.T.);
#11242=ORIENTED_EDGE('',*,*,#7820,.T.);
#11243=ORIENTED_EDGE('',*,*,#7682,.T.);
#11244=ORIENTED_EDGE('',*,*,#7821,.F.);
#11245=ORIENTED_EDGE('',*,*,#7687,.T.);
#11246=ORIENTED_EDGE('',*,*,#7691,.T.);
#11247=ORIENTED_EDGE('',*,*,#7821,.T.);
#11248=ORIENTED_EDGE('',*,*,#7681,.T.);
#11249=ORIENTED_EDGE('',*,*,#7685,.T.);
#11250=ORIENTED_EDGE('',*,*,#7818,.T.);
#11251=ORIENTED_EDGE('',*,*,#7819,.F.);
#11252=ORIENTED_EDGE('',*,*,#7683,.F.);
#11253=ORIENTED_EDGE('',*,*,#7820,.F.);
#11254=ORIENTED_EDGE('',*,*,#7689,.F.);
#11255=ORIENTED_EDGE('',*,*,#7672,.T.);
#11256=ORIENTED_EDGE('',*,*,#7692,.F.);
#11257=ORIENTED_EDGE('',*,*,#7670,.F.);
#11258=ORIENTED_EDGE('',*,*,#7693,.T.);
#11259=ORIENTED_EDGE('',*,*,#7651,.T.);
#11260=ORIENTED_EDGE('',*,*,#7822,.T.);
#11261=ORIENTED_EDGE('',*,*,#7679,.T.);
#11262=ORIENTED_EDGE('',*,*,#7823,.T.);
#11263=ORIENTED_EDGE('',*,*,#7824,.F.);
#11264=ORIENTED_EDGE('',*,*,#7677,.F.);
#11265=ORIENTED_EDGE('',*,*,#7825,.F.);
#11266=ORIENTED_EDGE('',*,*,#7649,.F.);
#11267=ORIENTED_EDGE('',*,*,#7650,.T.);
#11268=ORIENTED_EDGE('',*,*,#7825,.T.);
#11269=ORIENTED_EDGE('',*,*,#7680,.T.);
#11270=ORIENTED_EDGE('',*,*,#7822,.F.);
#11271=ORIENTED_EDGE('',*,*,#7652,.T.);
#11272=ORIENTED_EDGE('',*,*,#7823,.F.);
#11273=ORIENTED_EDGE('',*,*,#7678,.T.);
#11274=ORIENTED_EDGE('',*,*,#7824,.T.);
#11275=ORIENTED_EDGE('',*,*,#7664,.T.);
#11276=ORIENTED_EDGE('',*,*,#7826,.F.);
#11277=ORIENTED_EDGE('',*,*,#7660,.T.);
#11278=ORIENTED_EDGE('',*,*,#7827,.T.);
#11279=ORIENTED_EDGE('',*,*,#7666,.T.);
#11280=ORIENTED_EDGE('',*,*,#7828,.T.);
#11281=ORIENTED_EDGE('',*,*,#7658,.T.);
#11282=ORIENTED_EDGE('',*,*,#7829,.F.);
#11283=ORIENTED_EDGE('',*,*,#7663,.T.);
#11284=ORIENTED_EDGE('',*,*,#7667,.T.);
#11285=ORIENTED_EDGE('',*,*,#7829,.T.);
#11286=ORIENTED_EDGE('',*,*,#7657,.T.);
#11287=ORIENTED_EDGE('',*,*,#7661,.T.);
#11288=ORIENTED_EDGE('',*,*,#7826,.T.);
#11289=ORIENTED_EDGE('',*,*,#7827,.F.);
#11290=ORIENTED_EDGE('',*,*,#7659,.F.);
#11291=ORIENTED_EDGE('',*,*,#7828,.F.);
#11292=ORIENTED_EDGE('',*,*,#7665,.F.);
#11293=ORIENTED_EDGE('',*,*,#7648,.T.);
#11294=ORIENTED_EDGE('',*,*,#7668,.F.);
#11295=ORIENTED_EDGE('',*,*,#7646,.F.);
#11296=ORIENTED_EDGE('',*,*,#7669,.T.);
#11297=ORIENTED_EDGE('',*,*,#7627,.T.);
#11298=ORIENTED_EDGE('',*,*,#7830,.T.);
#11299=ORIENTED_EDGE('',*,*,#7655,.T.);
#11300=ORIENTED_EDGE('',*,*,#7831,.T.);
#11301=ORIENTED_EDGE('',*,*,#7832,.F.);
#11302=ORIENTED_EDGE('',*,*,#7653,.F.);
#11303=ORIENTED_EDGE('',*,*,#7833,.F.);
#11304=ORIENTED_EDGE('',*,*,#7625,.F.);
#11305=ORIENTED_EDGE('',*,*,#7626,.T.);
#11306=ORIENTED_EDGE('',*,*,#7833,.T.);
#11307=ORIENTED_EDGE('',*,*,#7656,.T.);
#11308=ORIENTED_EDGE('',*,*,#7830,.F.);
#11309=ORIENTED_EDGE('',*,*,#7628,.T.);
#11310=ORIENTED_EDGE('',*,*,#7831,.F.);
#11311=ORIENTED_EDGE('',*,*,#7654,.T.);
#11312=ORIENTED_EDGE('',*,*,#7832,.T.);
#11313=ORIENTED_EDGE('',*,*,#7640,.T.);
#11314=ORIENTED_EDGE('',*,*,#7834,.F.);
#11315=ORIENTED_EDGE('',*,*,#7636,.T.);
#11316=ORIENTED_EDGE('',*,*,#7835,.T.);
#11317=ORIENTED_EDGE('',*,*,#7642,.T.);
#11318=ORIENTED_EDGE('',*,*,#7836,.T.);
#11319=ORIENTED_EDGE('',*,*,#7634,.T.);
#11320=ORIENTED_EDGE('',*,*,#7837,.F.);
#11321=ORIENTED_EDGE('',*,*,#7639,.T.);
#11322=ORIENTED_EDGE('',*,*,#7643,.T.);
#11323=ORIENTED_EDGE('',*,*,#7837,.T.);
#11324=ORIENTED_EDGE('',*,*,#7633,.T.);
#11325=ORIENTED_EDGE('',*,*,#7637,.T.);
#11326=ORIENTED_EDGE('',*,*,#7834,.T.);
#11327=ORIENTED_EDGE('',*,*,#7835,.F.);
#11328=ORIENTED_EDGE('',*,*,#7635,.F.);
#11329=ORIENTED_EDGE('',*,*,#7836,.F.);
#11330=ORIENTED_EDGE('',*,*,#7641,.F.);
#11331=ORIENTED_EDGE('',*,*,#7624,.T.);
#11332=ORIENTED_EDGE('',*,*,#7644,.F.);
#11333=ORIENTED_EDGE('',*,*,#7622,.F.);
#11334=ORIENTED_EDGE('',*,*,#7645,.T.);
#11335=ORIENTED_EDGE('',*,*,#7784,.T.);
#11336=ORIENTED_EDGE('',*,*,#7838,.T.);
#11337=ORIENTED_EDGE('',*,*,#7631,.T.);
#11338=ORIENTED_EDGE('',*,*,#7839,.T.);
#11339=ORIENTED_EDGE('',*,*,#7840,.F.);
#11340=ORIENTED_EDGE('',*,*,#7629,.F.);
#11341=ORIENTED_EDGE('',*,*,#7841,.F.);
#11342=ORIENTED_EDGE('',*,*,#7782,.F.);
#11343=ORIENTED_EDGE('',*,*,#7783,.T.);
#11344=ORIENTED_EDGE('',*,*,#7841,.T.);
#11345=ORIENTED_EDGE('',*,*,#7632,.T.);
#11346=ORIENTED_EDGE('',*,*,#7838,.F.);
#11347=ORIENTED_EDGE('',*,*,#7785,.T.);
#11348=ORIENTED_EDGE('',*,*,#7839,.F.);
#11349=ORIENTED_EDGE('',*,*,#7630,.T.);
#11350=ORIENTED_EDGE('',*,*,#7840,.T.);
#11351=ORIENTED_EDGE('',*,*,#7762,.T.);
#11352=ORIENTED_EDGE('',*,*,#7842,.F.);
#11353=ORIENTED_EDGE('',*,*,#7757,.F.);
#11354=ORIENTED_EDGE('',*,*,#7843,.F.);
#11355=ORIENTED_EDGE('',*,*,#7844,.T.);
#11356=ORIENTED_EDGE('',*,*,#7755,.T.);
#11357=ORIENTED_EDGE('',*,*,#7759,.T.);
#11358=ORIENTED_EDGE('',*,*,#7845,.T.);
#11359=ORIENTED_EDGE('',*,*,#7760,.F.);
#11360=ORIENTED_EDGE('',*,*,#7753,.F.);
#11361=ORIENTED_EDGE('',*,*,#7845,.F.);
#11362=ORIENTED_EDGE('',*,*,#7758,.T.);
#11363=ORIENTED_EDGE('',*,*,#7842,.T.);
#11364=ORIENTED_EDGE('',*,*,#7761,.F.);
#11365=ORIENTED_EDGE('',*,*,#7843,.T.);
#11366=ORIENTED_EDGE('',*,*,#7756,.T.);
#11367=ORIENTED_EDGE('',*,*,#7844,.F.);
#11368=ORIENTED_EDGE('',*,*,#7763,.F.);
#11369=ORIENTED_EDGE('',*,*,#7846,.T.);
#11370=ORIENTED_EDGE('',*,*,#7847,.T.);
#11371=ORIENTED_EDGE('',*,*,#7848,.F.);
#11372=ORIENTED_EDGE('',*,*,#7847,.F.);
#11373=ORIENTED_EDGE('',*,*,#7849,.T.);
#11374=ORIENTED_EDGE('',*,*,#7850,.T.);
#11375=ORIENTED_EDGE('',*,*,#7851,.T.);
#11376=ORIENTED_EDGE('',*,*,#7852,.T.);
#11377=ORIENTED_EDGE('',*,*,#7850,.F.);
#11378=ORIENTED_EDGE('',*,*,#7853,.T.);
#11379=ORIENTED_EDGE('',*,*,#7854,.T.);
#11380=ORIENTED_EDGE('',*,*,#7855,.T.);
#11381=ORIENTED_EDGE('',*,*,#7856,.T.);
#11382=ORIENTED_EDGE('',*,*,#7855,.F.);
#11383=ORIENTED_EDGE('',*,*,#7857,.T.);
#11384=ORIENTED_EDGE('',*,*,#7849,.F.);
#11385=ORIENTED_EDGE('',*,*,#7858,.T.);
#11386=ORIENTED_EDGE('',*,*,#7859,.F.);
#11387=ORIENTED_EDGE('',*,*,#7858,.F.);
#11388=ORIENTED_EDGE('',*,*,#7853,.F.);
#11389=ORIENTED_EDGE('',*,*,#7852,.F.);
#11390=ORIENTED_EDGE('',*,*,#7860,.T.);
#11391=ORIENTED_EDGE('',*,*,#7857,.F.);
#11392=ORIENTED_EDGE('',*,*,#7854,.F.);
#11393=ORIENTED_EDGE('',*,*,#7860,.F.);
#11394=ORIENTED_EDGE('',*,*,#7851,.F.);
#11395=ORIENTED_EDGE('',*,*,#7856,.F.);
#11396=ORIENTED_EDGE('',*,*,#7861,.T.);
#11397=ORIENTED_EDGE('',*,*,#7862,.T.);
#11398=ORIENTED_EDGE('',*,*,#7861,.F.);
#11399=ORIENTED_EDGE('',*,*,#7863,.F.);
#11400=ORIENTED_EDGE('',*,*,#7864,.T.);
#11401=ORIENTED_EDGE('',*,*,#7848,.T.);
#11402=ORIENTED_EDGE('',*,*,#7864,.F.);
#11403=ORIENTED_EDGE('',*,*,#7846,.F.);
#11404=ORIENTED_EDGE('',*,*,#7865,.T.);
#11405=ORIENTED_EDGE('',*,*,#7866,.T.);
#11406=ORIENTED_EDGE('',*,*,#7865,.F.);
#11407=ORIENTED_EDGE('',*,*,#7866,.F.);
#11408=ORIENTED_EDGE('',*,*,#7859,.T.);
#11409=ORIENTED_EDGE('',*,*,#7863,.T.);
#11410=ORIENTED_EDGE('',*,*,#7862,.F.);
#11411=ORIENTED_EDGE('',*,*,#7867,.T.);
#11412=ORIENTED_EDGE('',*,*,#7867,.F.);
#11413=ORIENTED_EDGE('',*,*,#7868,.T.);
#11414=ORIENTED_EDGE('',*,*,#7868,.F.);
#11415=ORIENTED_EDGE('',*,*,#7869,.T.);
#11416=ORIENTED_EDGE('',*,*,#7869,.F.);
#11417=ORIENTED_EDGE('',*,*,#7870,.T.);
#11418=ORIENTED_EDGE('',*,*,#7870,.F.);
#11419=ORIENTED_EDGE('',*,*,#7871,.T.);
#11420=ORIENTED_EDGE('',*,*,#7871,.F.);
#11421=ORIENTED_EDGE('',*,*,#7872,.T.);
#11422=ORIENTED_EDGE('',*,*,#7872,.F.);
#11423=ORIENTED_EDGE('',*,*,#7873,.T.);
#11424=ORIENTED_EDGE('',*,*,#7873,.F.);
#11425=ORIENTED_EDGE('',*,*,#7874,.T.);
#11426=ORIENTED_EDGE('',*,*,#7875,.T.);
#11427=ORIENTED_EDGE('',*,*,#7876,.T.);
#11428=ORIENTED_EDGE('',*,*,#7877,.T.);
#11429=ORIENTED_EDGE('',*,*,#7875,.F.);
#11430=ORIENTED_EDGE('',*,*,#7878,.T.);
#11431=ORIENTED_EDGE('',*,*,#7879,.T.);
#11432=ORIENTED_EDGE('',*,*,#7880,.T.);
#11433=ORIENTED_EDGE('',*,*,#7879,.F.);
#11434=ORIENTED_EDGE('',*,*,#7881,.T.);
#11435=ORIENTED_EDGE('',*,*,#7882,.T.);
#11436=ORIENTED_EDGE('',*,*,#7883,.T.);
#11437=ORIENTED_EDGE('',*,*,#7882,.F.);
#11438=ORIENTED_EDGE('',*,*,#7884,.T.);
#11439=ORIENTED_EDGE('',*,*,#7885,.T.);
#11440=ORIENTED_EDGE('',*,*,#7886,.T.);
#11441=ORIENTED_EDGE('',*,*,#7885,.F.);
#11442=ORIENTED_EDGE('',*,*,#7887,.T.);
#11443=ORIENTED_EDGE('',*,*,#7888,.F.);
#11444=ORIENTED_EDGE('',*,*,#7889,.T.);
#11445=ORIENTED_EDGE('',*,*,#7890,.T.);
#11446=ORIENTED_EDGE('',*,*,#7889,.F.);
#11447=ORIENTED_EDGE('',*,*,#7877,.F.);
#11448=ORIENTED_EDGE('',*,*,#7891,.T.);
#11449=ORIENTED_EDGE('',*,*,#7892,.T.);
#11450=ORIENTED_EDGE('',*,*,#7891,.F.);
#11451=ORIENTED_EDGE('',*,*,#7876,.F.);
#11452=ORIENTED_EDGE('',*,*,#7893,.F.);
#11453=ORIENTED_EDGE('',*,*,#7894,.T.);
#11454=ORIENTED_EDGE('',*,*,#7887,.F.);
#11455=ORIENTED_EDGE('',*,*,#7884,.F.);
#11456=ORIENTED_EDGE('',*,*,#7894,.F.);
#11457=ORIENTED_EDGE('',*,*,#7893,.T.);
#11458=ORIENTED_EDGE('',*,*,#7895,.T.);
#11459=ORIENTED_EDGE('',*,*,#7896,.F.);
#11460=ORIENTED_EDGE('',*,*,#7895,.F.);
#11461=ORIENTED_EDGE('',*,*,#7878,.F.);
#11462=ORIENTED_EDGE('',*,*,#7897,.T.);
#11463=ORIENTED_EDGE('',*,*,#7896,.T.);
#11464=ORIENTED_EDGE('',*,*,#7897,.F.);
#11465=ORIENTED_EDGE('',*,*,#7898,.F.);
#11466=ORIENTED_EDGE('',*,*,#7899,.T.);
#11467=ORIENTED_EDGE('',*,*,#7883,.F.);
#11468=ORIENTED_EDGE('',*,*,#7899,.F.);
#11469=ORIENTED_EDGE('',*,*,#7900,.F.);
#11470=ORIENTED_EDGE('',*,*,#7901,.T.);
#11471=ORIENTED_EDGE('',*,*,#7902,.T.);
#11472=ORIENTED_EDGE('',*,*,#7901,.F.);
#11473=ORIENTED_EDGE('',*,*,#7903,.T.);
#11474=ORIENTED_EDGE('',*,*,#7904,.T.);
#11475=ORIENTED_EDGE('',*,*,#7905,.F.);
#11476=ORIENTED_EDGE('',*,*,#7904,.F.);
#11477=ORIENTED_EDGE('',*,*,#7906,.F.);
#11478=ORIENTED_EDGE('',*,*,#7907,.F.);
#11479=ORIENTED_EDGE('',*,*,#7908,.T.);
#11480=ORIENTED_EDGE('',*,*,#7909,.T.);
#11481=ORIENTED_EDGE('',*,*,#7908,.F.);
#11482=ORIENTED_EDGE('',*,*,#7903,.F.);
#11483=ORIENTED_EDGE('',*,*,#7910,.T.);
#11484=ORIENTED_EDGE('',*,*,#7906,.T.);
#11485=ORIENTED_EDGE('',*,*,#7907,.T.);
#11486=ORIENTED_EDGE('',*,*,#7910,.F.);
#11487=ORIENTED_EDGE('',*,*,#7909,.F.);
#11488=ORIENTED_EDGE('',*,*,#7874,.F.);
#11489=ORIENTED_EDGE('',*,*,#7905,.T.);
#11490=ORIENTED_EDGE('',*,*,#7881,.F.);
#11491=ORIENTED_EDGE('',*,*,#7900,.T.);
#11492=ORIENTED_EDGE('',*,*,#7886,.F.);
#11493=ORIENTED_EDGE('',*,*,#7902,.F.);
#11494=ORIENTED_EDGE('',*,*,#7898,.T.);
#11495=ORIENTED_EDGE('',*,*,#7888,.T.);
#11496=ORIENTED_EDGE('',*,*,#7892,.F.);
#11497=ORIENTED_EDGE('',*,*,#7890,.F.);
#11498=ORIENTED_EDGE('',*,*,#7880,.F.);
#11499=ORIENTED_EDGE('',*,*,#7911,.T.);
#11500=ORIENTED_EDGE('',*,*,#7912,.T.);
#11501=ORIENTED_EDGE('',*,*,#7913,.F.);
#11502=ORIENTED_EDGE('',*,*,#7912,.F.);
#11503=ORIENTED_EDGE('',*,*,#7914,.T.);
#11504=ORIENTED_EDGE('',*,*,#7915,.F.);
#11505=ORIENTED_EDGE('',*,*,#7916,.F.);
#11506=ORIENTED_EDGE('',*,*,#7917,.F.);
#11507=ORIENTED_EDGE('',*,*,#7918,.T.);
#11508=ORIENTED_EDGE('',*,*,#7919,.F.);
#11509=ORIENTED_EDGE('',*,*,#7920,.F.);
#11510=ORIENTED_EDGE('',*,*,#7921,.F.);
#11511=ORIENTED_EDGE('',*,*,#7922,.F.);
#11512=ORIENTED_EDGE('',*,*,#7923,.F.);
#11513=ORIENTED_EDGE('',*,*,#7924,.T.);
#11514=ORIENTED_EDGE('',*,*,#7925,.F.);
#11515=ORIENTED_EDGE('',*,*,#7926,.F.);
#11516=ORIENTED_EDGE('',*,*,#7927,.T.);
#11517=ORIENTED_EDGE('',*,*,#7928,.F.);
#11518=ORIENTED_EDGE('',*,*,#7929,.F.);
#11519=ORIENTED_EDGE('',*,*,#7930,.T.);
#11520=ORIENTED_EDGE('',*,*,#7931,.F.);
#11521=ORIENTED_EDGE('',*,*,#7932,.F.);
#11522=ORIENTED_EDGE('',*,*,#7927,.F.);
#11523=ORIENTED_EDGE('',*,*,#7933,.T.);
#11524=ORIENTED_EDGE('',*,*,#7934,.F.);
#11525=ORIENTED_EDGE('',*,*,#7935,.T.);
#11526=ORIENTED_EDGE('',*,*,#7936,.T.);
#11527=ORIENTED_EDGE('',*,*,#7937,.F.);
#11528=ORIENTED_EDGE('',*,*,#7936,.F.);
#11529=ORIENTED_EDGE('',*,*,#7938,.T.);
#11530=ORIENTED_EDGE('',*,*,#7939,.F.);
#11531=ORIENTED_EDGE('',*,*,#7940,.F.);
#11532=ORIENTED_EDGE('',*,*,#7941,.F.);
#11533=ORIENTED_EDGE('',*,*,#7942,.T.);
#11534=ORIENTED_EDGE('',*,*,#7943,.F.);
#11535=ORIENTED_EDGE('',*,*,#7944,.F.);
#11536=ORIENTED_EDGE('',*,*,#7945,.F.);
#11537=ORIENTED_EDGE('',*,*,#7946,.F.);
#11538=ORIENTED_EDGE('',*,*,#7947,.F.);
#11539=ORIENTED_EDGE('',*,*,#7948,.T.);
#11540=ORIENTED_EDGE('',*,*,#7949,.F.);
#11541=ORIENTED_EDGE('',*,*,#7950,.F.);
#11542=ORIENTED_EDGE('',*,*,#7951,.T.);
#11543=ORIENTED_EDGE('',*,*,#7952,.F.);
#11544=ORIENTED_EDGE('',*,*,#7953,.F.);
#11545=ORIENTED_EDGE('',*,*,#7954,.T.);
#11546=ORIENTED_EDGE('',*,*,#7955,.F.);
#11547=ORIENTED_EDGE('',*,*,#7956,.F.);
#11548=ORIENTED_EDGE('',*,*,#7951,.F.);
#11549=ORIENTED_EDGE('',*,*,#7957,.T.);
#11550=ORIENTED_EDGE('',*,*,#7958,.F.);
#11551=ORIENTED_EDGE('',*,*,#7959,.T.);
#11552=ORIENTED_EDGE('',*,*,#7960,.T.);
#11553=ORIENTED_EDGE('',*,*,#7961,.F.);
#11554=ORIENTED_EDGE('',*,*,#7960,.F.);
#11555=ORIENTED_EDGE('',*,*,#7962,.T.);
#11556=ORIENTED_EDGE('',*,*,#7963,.F.);
#11557=ORIENTED_EDGE('',*,*,#7964,.F.);
#11558=ORIENTED_EDGE('',*,*,#7965,.F.);
#11559=ORIENTED_EDGE('',*,*,#7966,.T.);
#11560=ORIENTED_EDGE('',*,*,#7967,.F.);
#11561=ORIENTED_EDGE('',*,*,#7968,.F.);
#11562=ORIENTED_EDGE('',*,*,#7969,.F.);
#11563=ORIENTED_EDGE('',*,*,#7970,.F.);
#11564=ORIENTED_EDGE('',*,*,#7971,.F.);
#11565=ORIENTED_EDGE('',*,*,#7972,.T.);
#11566=ORIENTED_EDGE('',*,*,#7973,.F.);
#11567=ORIENTED_EDGE('',*,*,#7974,.F.);
#11568=ORIENTED_EDGE('',*,*,#7975,.T.);
#11569=ORIENTED_EDGE('',*,*,#7976,.F.);
#11570=ORIENTED_EDGE('',*,*,#7977,.F.);
#11571=ORIENTED_EDGE('',*,*,#7978,.T.);
#11572=ORIENTED_EDGE('',*,*,#7979,.F.);
#11573=ORIENTED_EDGE('',*,*,#7980,.F.);
#11574=ORIENTED_EDGE('',*,*,#7975,.F.);
#11575=ORIENTED_EDGE('',*,*,#7981,.T.);
#11576=ORIENTED_EDGE('',*,*,#7982,.F.);
#11577=ORIENTED_EDGE('',*,*,#7983,.T.);
#11578=ORIENTED_EDGE('',*,*,#7984,.T.);
#11579=ORIENTED_EDGE('',*,*,#7985,.F.);
#11580=ORIENTED_EDGE('',*,*,#7984,.F.);
#11581=ORIENTED_EDGE('',*,*,#7986,.T.);
#11582=ORIENTED_EDGE('',*,*,#7987,.F.);
#11583=ORIENTED_EDGE('',*,*,#7988,.F.);
#11584=ORIENTED_EDGE('',*,*,#7989,.F.);
#11585=ORIENTED_EDGE('',*,*,#7990,.T.);
#11586=ORIENTED_EDGE('',*,*,#7991,.F.);
#11587=ORIENTED_EDGE('',*,*,#7992,.F.);
#11588=ORIENTED_EDGE('',*,*,#7993,.F.);
#11589=ORIENTED_EDGE('',*,*,#7994,.F.);
#11590=ORIENTED_EDGE('',*,*,#7995,.F.);
#11591=ORIENTED_EDGE('',*,*,#7996,.T.);
#11592=ORIENTED_EDGE('',*,*,#7997,.F.);
#11593=ORIENTED_EDGE('',*,*,#7998,.F.);
#11594=ORIENTED_EDGE('',*,*,#7999,.T.);
#11595=ORIENTED_EDGE('',*,*,#8000,.F.);
#11596=ORIENTED_EDGE('',*,*,#8001,.F.);
#11597=ORIENTED_EDGE('',*,*,#8002,.T.);
#11598=ORIENTED_EDGE('',*,*,#8003,.F.);
#11599=ORIENTED_EDGE('',*,*,#8004,.F.);
#11600=ORIENTED_EDGE('',*,*,#7999,.F.);
#11601=ORIENTED_EDGE('',*,*,#8005,.T.);
#11602=ORIENTED_EDGE('',*,*,#8006,.F.);
#11603=ORIENTED_EDGE('',*,*,#8007,.T.);
#11604=ORIENTED_EDGE('',*,*,#8008,.T.);
#11605=ORIENTED_EDGE('',*,*,#8009,.F.);
#11606=ORIENTED_EDGE('',*,*,#8008,.F.);
#11607=ORIENTED_EDGE('',*,*,#8010,.T.);
#11608=ORIENTED_EDGE('',*,*,#8011,.F.);
#11609=ORIENTED_EDGE('',*,*,#8012,.F.);
#11610=ORIENTED_EDGE('',*,*,#8013,.F.);
#11611=ORIENTED_EDGE('',*,*,#8014,.T.);
#11612=ORIENTED_EDGE('',*,*,#8015,.F.);
#11613=ORIENTED_EDGE('',*,*,#8016,.F.);
#11614=ORIENTED_EDGE('',*,*,#8017,.F.);
#11615=ORIENTED_EDGE('',*,*,#8018,.F.);
#11616=ORIENTED_EDGE('',*,*,#8019,.F.);
#11617=ORIENTED_EDGE('',*,*,#8020,.T.);
#11618=ORIENTED_EDGE('',*,*,#8021,.F.);
#11619=ORIENTED_EDGE('',*,*,#8022,.F.);
#11620=ORIENTED_EDGE('',*,*,#8023,.T.);
#11621=ORIENTED_EDGE('',*,*,#8024,.F.);
#11622=ORIENTED_EDGE('',*,*,#8025,.F.);
#11623=ORIENTED_EDGE('',*,*,#8026,.T.);
#11624=ORIENTED_EDGE('',*,*,#8027,.F.);
#11625=ORIENTED_EDGE('',*,*,#8028,.F.);
#11626=ORIENTED_EDGE('',*,*,#8023,.F.);
#11627=ORIENTED_EDGE('',*,*,#8029,.T.);
#11628=ORIENTED_EDGE('',*,*,#8030,.F.);
#11629=ORIENTED_EDGE('',*,*,#8031,.T.);
#11630=ORIENTED_EDGE('',*,*,#8032,.T.);
#11631=ORIENTED_EDGE('',*,*,#8033,.F.);
#11632=ORIENTED_EDGE('',*,*,#8032,.F.);
#11633=ORIENTED_EDGE('',*,*,#8034,.T.);
#11634=ORIENTED_EDGE('',*,*,#8035,.T.);
#11635=ORIENTED_EDGE('',*,*,#8036,.T.);
#11636=ORIENTED_EDGE('',*,*,#8037,.F.);
#11637=ORIENTED_EDGE('',*,*,#8038,.T.);
#11638=ORIENTED_EDGE('',*,*,#8039,.F.);
#11639=ORIENTED_EDGE('',*,*,#8040,.F.);
#11640=ORIENTED_EDGE('',*,*,#8041,.F.);
#11641=ORIENTED_EDGE('',*,*,#8042,.T.);
#11642=ORIENTED_EDGE('',*,*,#8043,.T.);
#11643=ORIENTED_EDGE('',*,*,#8044,.F.);
#11644=ORIENTED_EDGE('',*,*,#8045,.F.);
#11645=ORIENTED_EDGE('',*,*,#8046,.T.);
#11646=ORIENTED_EDGE('',*,*,#8047,.F.);
#11647=ORIENTED_EDGE('',*,*,#8048,.F.);
#11648=ORIENTED_EDGE('',*,*,#8043,.F.);
#11649=ORIENTED_EDGE('',*,*,#8049,.T.);
#11650=ORIENTED_EDGE('',*,*,#8050,.T.);
#11651=ORIENTED_EDGE('',*,*,#8051,.F.);
#11652=ORIENTED_EDGE('',*,*,#8052,.T.);
#11653=ORIENTED_EDGE('',*,*,#8053,.T.);
#11654=ORIENTED_EDGE('',*,*,#8054,.F.);
#11655=ORIENTED_EDGE('',*,*,#8055,.F.);
#11656=ORIENTED_EDGE('',*,*,#8056,.F.);
#11657=ORIENTED_EDGE('',*,*,#8057,.T.);
#11658=ORIENTED_EDGE('',*,*,#8058,.F.);
#11659=ORIENTED_EDGE('',*,*,#8059,.F.);
#11660=ORIENTED_EDGE('',*,*,#8060,.T.);
#11661=ORIENTED_EDGE('',*,*,#8061,.F.);
#11662=ORIENTED_EDGE('',*,*,#8062,.F.);
#11663=ORIENTED_EDGE('',*,*,#8063,.T.);
#11664=ORIENTED_EDGE('',*,*,#8064,.F.);
#11665=ORIENTED_EDGE('',*,*,#8065,.F.);
#11666=ORIENTED_EDGE('',*,*,#8060,.F.);
#11667=ORIENTED_EDGE('',*,*,#8066,.T.);
#11668=ORIENTED_EDGE('',*,*,#8067,.F.);
#11669=ORIENTED_EDGE('',*,*,#8068,.T.);
#11670=ORIENTED_EDGE('',*,*,#8069,.T.);
#11671=ORIENTED_EDGE('',*,*,#8070,.F.);
#11672=ORIENTED_EDGE('',*,*,#8069,.F.);
#11673=ORIENTED_EDGE('',*,*,#8071,.T.);
#11674=ORIENTED_EDGE('',*,*,#8072,.F.);
#11675=ORIENTED_EDGE('',*,*,#8073,.F.);
#11676=ORIENTED_EDGE('',*,*,#8074,.F.);
#11677=ORIENTED_EDGE('',*,*,#8075,.T.);
#11678=ORIENTED_EDGE('',*,*,#8076,.F.);
#11679=ORIENTED_EDGE('',*,*,#8077,.F.);
#11680=ORIENTED_EDGE('',*,*,#8078,.F.);
#11681=ORIENTED_EDGE('',*,*,#8079,.F.);
#11682=ORIENTED_EDGE('',*,*,#8076,.T.);
#11683=ORIENTED_EDGE('',*,*,#8080,.T.);
#11684=ORIENTED_EDGE('',*,*,#8036,.F.);
#11685=ORIENTED_EDGE('',*,*,#8081,.T.);
#11686=ORIENTED_EDGE('',*,*,#8078,.T.);
#11687=ORIENTED_EDGE('',*,*,#8082,.F.);
#11688=ORIENTED_EDGE('',*,*,#8034,.F.);
#11689=ORIENTED_EDGE('',*,*,#8037,.T.);
#11690=ORIENTED_EDGE('',*,*,#8080,.F.);
#11691=ORIENTED_EDGE('',*,*,#8075,.F.);
#11692=ORIENTED_EDGE('',*,*,#8081,.F.);
#11693=ORIENTED_EDGE('',*,*,#8082,.T.);
#11694=ORIENTED_EDGE('',*,*,#8077,.T.);
#11695=ORIENTED_EDGE('',*,*,#8079,.T.);
#11696=ORIENTED_EDGE('',*,*,#8035,.F.);
#11697=ORIENTED_EDGE('',*,*,#8068,.F.);
#11698=ORIENTED_EDGE('',*,*,#8067,.T.);
#11699=ORIENTED_EDGE('',*,*,#8070,.T.);
#11700=ORIENTED_EDGE('',*,*,#8066,.F.);
#11701=ORIENTED_EDGE('',*,*,#8083,.F.);
#11702=ORIENTED_EDGE('',*,*,#8057,.F.);
#11703=ORIENTED_EDGE('',*,*,#8084,.F.);
#11704=ORIENTED_EDGE('',*,*,#8063,.F.);
#11705=ORIENTED_EDGE('',*,*,#8061,.T.);
#11706=ORIENTED_EDGE('',*,*,#8065,.T.);
#11707=ORIENTED_EDGE('',*,*,#8085,.T.);
#11708=ORIENTED_EDGE('',*,*,#8055,.T.);
#11709=ORIENTED_EDGE('',*,*,#8059,.T.);
#11710=ORIENTED_EDGE('',*,*,#8086,.T.);
#11711=ORIENTED_EDGE('',*,*,#8064,.T.);
#11712=ORIENTED_EDGE('',*,*,#8084,.T.);
#11713=ORIENTED_EDGE('',*,*,#8056,.T.);
#11714=ORIENTED_EDGE('',*,*,#8085,.F.);
#11715=ORIENTED_EDGE('',*,*,#8062,.T.);
#11716=ORIENTED_EDGE('',*,*,#8086,.F.);
#11717=ORIENTED_EDGE('',*,*,#8058,.T.);
#11718=ORIENTED_EDGE('',*,*,#8083,.T.);
#11719=ORIENTED_EDGE('',*,*,#8033,.T.);
#11720=ORIENTED_EDGE('',*,*,#8053,.F.);
#11721=ORIENTED_EDGE('',*,*,#8031,.F.);
#11722=ORIENTED_EDGE('',*,*,#8054,.T.);
#11723=ORIENTED_EDGE('',*,*,#8012,.T.);
#11724=ORIENTED_EDGE('',*,*,#8087,.T.);
#11725=ORIENTED_EDGE('',*,*,#8040,.T.);
#11726=ORIENTED_EDGE('',*,*,#8088,.T.);
#11727=ORIENTED_EDGE('',*,*,#8089,.F.);
#11728=ORIENTED_EDGE('',*,*,#8038,.F.);
#11729=ORIENTED_EDGE('',*,*,#8090,.F.);
#11730=ORIENTED_EDGE('',*,*,#8010,.F.);
#11731=ORIENTED_EDGE('',*,*,#8011,.T.);
#11732=ORIENTED_EDGE('',*,*,#8090,.T.);
#11733=ORIENTED_EDGE('',*,*,#8041,.T.);
#11734=ORIENTED_EDGE('',*,*,#8087,.F.);
#11735=ORIENTED_EDGE('',*,*,#8013,.T.);
#11736=ORIENTED_EDGE('',*,*,#8088,.F.);
#11737=ORIENTED_EDGE('',*,*,#8039,.T.);
#11738=ORIENTED_EDGE('',*,*,#8089,.T.);
#11739=ORIENTED_EDGE('',*,*,#8025,.T.);
#11740=ORIENTED_EDGE('',*,*,#8091,.F.);
#11741=ORIENTED_EDGE('',*,*,#8021,.T.);
#11742=ORIENTED_EDGE('',*,*,#8092,.T.);
#11743=ORIENTED_EDGE('',*,*,#8027,.T.);
#11744=ORIENTED_EDGE('',*,*,#8093,.T.);
#11745=ORIENTED_EDGE('',*,*,#8019,.T.);
#11746=ORIENTED_EDGE('',*,*,#8094,.F.);
#11747=ORIENTED_EDGE('',*,*,#8024,.T.);
#11748=ORIENTED_EDGE('',*,*,#8028,.T.);
#11749=ORIENTED_EDGE('',*,*,#8094,.T.);
#11750=ORIENTED_EDGE('',*,*,#8018,.T.);
#11751=ORIENTED_EDGE('',*,*,#8022,.T.);
#11752=ORIENTED_EDGE('',*,*,#8091,.T.);
#11753=ORIENTED_EDGE('',*,*,#8092,.F.);
#11754=ORIENTED_EDGE('',*,*,#8020,.F.);
#11755=ORIENTED_EDGE('',*,*,#8093,.F.);
#11756=ORIENTED_EDGE('',*,*,#8026,.F.);
#11757=ORIENTED_EDGE('',*,*,#8009,.T.);
#11758=ORIENTED_EDGE('',*,*,#8029,.F.);
#11759=ORIENTED_EDGE('',*,*,#8007,.F.);
#11760=ORIENTED_EDGE('',*,*,#8030,.T.);
#11761=ORIENTED_EDGE('',*,*,#7988,.T.);
#11762=ORIENTED_EDGE('',*,*,#8095,.T.);
#11763=ORIENTED_EDGE('',*,*,#8016,.T.);
#11764=ORIENTED_EDGE('',*,*,#8096,.T.);
#11765=ORIENTED_EDGE('',*,*,#8097,.F.);
#11766=ORIENTED_EDGE('',*,*,#8014,.F.);
#11767=ORIENTED_EDGE('',*,*,#8098,.F.);
#11768=ORIENTED_EDGE('',*,*,#7986,.F.);
#11769=ORIENTED_EDGE('',*,*,#7987,.T.);
#11770=ORIENTED_EDGE('',*,*,#8098,.T.);
#11771=ORIENTED_EDGE('',*,*,#8017,.T.);
#11772=ORIENTED_EDGE('',*,*,#8095,.F.);
#11773=ORIENTED_EDGE('',*,*,#7989,.T.);
#11774=ORIENTED_EDGE('',*,*,#8096,.F.);
#11775=ORIENTED_EDGE('',*,*,#8015,.T.);
#11776=ORIENTED_EDGE('',*,*,#8097,.T.);
#11777=ORIENTED_EDGE('',*,*,#8001,.T.);
#11778=ORIENTED_EDGE('',*,*,#8099,.F.);
#11779=ORIENTED_EDGE('',*,*,#7997,.T.);
#11780=ORIENTED_EDGE('',*,*,#8100,.T.);
#11781=ORIENTED_EDGE('',*,*,#8003,.T.);
#11782=ORIENTED_EDGE('',*,*,#8101,.T.);
#11783=ORIENTED_EDGE('',*,*,#7995,.T.);
#11784=ORIENTED_EDGE('',*,*,#8102,.F.);
#11785=ORIENTED_EDGE('',*,*,#8000,.T.);
#11786=ORIENTED_EDGE('',*,*,#8004,.T.);
#11787=ORIENTED_EDGE('',*,*,#8102,.T.);
#11788=ORIENTED_EDGE('',*,*,#7994,.T.);
#11789=ORIENTED_EDGE('',*,*,#7998,.T.);
#11790=ORIENTED_EDGE('',*,*,#8099,.T.);
#11791=ORIENTED_EDGE('',*,*,#8100,.F.);
#11792=ORIENTED_EDGE('',*,*,#7996,.F.);
#11793=ORIENTED_EDGE('',*,*,#8101,.F.);
#11794=ORIENTED_EDGE('',*,*,#8002,.F.);
#11795=ORIENTED_EDGE('',*,*,#7985,.T.);
#11796=ORIENTED_EDGE('',*,*,#8005,.F.);
#11797=ORIENTED_EDGE('',*,*,#7983,.F.);
#11798=ORIENTED_EDGE('',*,*,#8006,.T.);
#11799=ORIENTED_EDGE('',*,*,#7964,.T.);
#11800=ORIENTED_EDGE('',*,*,#8103,.T.);
#11801=ORIENTED_EDGE('',*,*,#7992,.T.);
#11802=ORIENTED_EDGE('',*,*,#8104,.T.);
#11803=ORIENTED_EDGE('',*,*,#8105,.F.);
#11804=ORIENTED_EDGE('',*,*,#7990,.F.);
#11805=ORIENTED_EDGE('',*,*,#8106,.F.);
#11806=ORIENTED_EDGE('',*,*,#7962,.F.);
#11807=ORIENTED_EDGE('',*,*,#7963,.T.);
#11808=ORIENTED_EDGE('',*,*,#8106,.T.);
#11809=ORIENTED_EDGE('',*,*,#7993,.T.);
#11810=ORIENTED_EDGE('',*,*,#8103,.F.);
#11811=ORIENTED_EDGE('',*,*,#7965,.T.);
#11812=ORIENTED_EDGE('',*,*,#8104,.F.);
#11813=ORIENTED_EDGE('',*,*,#7991,.T.);
#11814=ORIENTED_EDGE('',*,*,#8105,.T.);
#11815=ORIENTED_EDGE('',*,*,#7977,.T.);
#11816=ORIENTED_EDGE('',*,*,#8107,.F.);
#11817=ORIENTED_EDGE('',*,*,#7973,.T.);
#11818=ORIENTED_EDGE('',*,*,#8108,.T.);
#11819=ORIENTED_EDGE('',*,*,#7979,.T.);
#11820=ORIENTED_EDGE('',*,*,#8109,.T.);
#11821=ORIENTED_EDGE('',*,*,#7971,.T.);
#11822=ORIENTED_EDGE('',*,*,#8110,.F.);
#11823=ORIENTED_EDGE('',*,*,#7976,.T.);
#11824=ORIENTED_EDGE('',*,*,#7980,.T.);
#11825=ORIENTED_EDGE('',*,*,#8110,.T.);
#11826=ORIENTED_EDGE('',*,*,#7970,.T.);
#11827=ORIENTED_EDGE('',*,*,#7974,.T.);
#11828=ORIENTED_EDGE('',*,*,#8107,.T.);
#11829=ORIENTED_EDGE('',*,*,#8108,.F.);
#11830=ORIENTED_EDGE('',*,*,#7972,.F.);
#11831=ORIENTED_EDGE('',*,*,#8109,.F.);
#11832=ORIENTED_EDGE('',*,*,#7978,.F.);
#11833=ORIENTED_EDGE('',*,*,#7961,.T.);
#11834=ORIENTED_EDGE('',*,*,#7981,.F.);
#11835=ORIENTED_EDGE('',*,*,#7959,.F.);
#11836=ORIENTED_EDGE('',*,*,#7982,.T.);
#11837=ORIENTED_EDGE('',*,*,#7940,.T.);
#11838=ORIENTED_EDGE('',*,*,#8111,.T.);
#11839=ORIENTED_EDGE('',*,*,#7968,.T.);
#11840=ORIENTED_EDGE('',*,*,#8112,.T.);
#11841=ORIENTED_EDGE('',*,*,#8113,.F.);
#11842=ORIENTED_EDGE('',*,*,#7966,.F.);
#11843=ORIENTED_EDGE('',*,*,#8114,.F.);
#11844=ORIENTED_EDGE('',*,*,#7938,.F.);
#11845=ORIENTED_EDGE('',*,*,#7939,.T.);
#11846=ORIENTED_EDGE('',*,*,#8114,.T.);
#11847=ORIENTED_EDGE('',*,*,#7969,.T.);
#11848=ORIENTED_EDGE('',*,*,#8111,.F.);
#11849=ORIENTED_EDGE('',*,*,#7941,.T.);
#11850=ORIENTED_EDGE('',*,*,#8112,.F.);
#11851=ORIENTED_EDGE('',*,*,#7967,.T.);
#11852=ORIENTED_EDGE('',*,*,#8113,.T.);
#11853=ORIENTED_EDGE('',*,*,#7953,.T.);
#11854=ORIENTED_EDGE('',*,*,#8115,.F.);
#11855=ORIENTED_EDGE('',*,*,#7949,.T.);
#11856=ORIENTED_EDGE('',*,*,#8116,.T.);
#11857=ORIENTED_EDGE('',*,*,#7955,.T.);
#11858=ORIENTED_EDGE('',*,*,#8117,.T.);
#11859=ORIENTED_EDGE('',*,*,#7947,.T.);
#11860=ORIENTED_EDGE('',*,*,#8118,.F.);
#11861=ORIENTED_EDGE('',*,*,#7952,.T.);
#11862=ORIENTED_EDGE('',*,*,#7956,.T.);
#11863=ORIENTED_EDGE('',*,*,#8118,.T.);
#11864=ORIENTED_EDGE('',*,*,#7946,.T.);
#11865=ORIENTED_EDGE('',*,*,#7950,.T.);
#11866=ORIENTED_EDGE('',*,*,#8115,.T.);
#11867=ORIENTED_EDGE('',*,*,#8116,.F.);
#11868=ORIENTED_EDGE('',*,*,#7948,.F.);
#11869=ORIENTED_EDGE('',*,*,#8117,.F.);
#11870=ORIENTED_EDGE('',*,*,#7954,.F.);
#11871=ORIENTED_EDGE('',*,*,#7937,.T.);
#11872=ORIENTED_EDGE('',*,*,#7957,.F.);
#11873=ORIENTED_EDGE('',*,*,#7935,.F.);
#11874=ORIENTED_EDGE('',*,*,#7958,.T.);
#11875=ORIENTED_EDGE('',*,*,#7916,.T.);
#11876=ORIENTED_EDGE('',*,*,#8119,.T.);
#11877=ORIENTED_EDGE('',*,*,#7944,.T.);
#11878=ORIENTED_EDGE('',*,*,#8120,.T.);
#11879=ORIENTED_EDGE('',*,*,#8121,.F.);
#11880=ORIENTED_EDGE('',*,*,#7942,.F.);
#11881=ORIENTED_EDGE('',*,*,#8122,.F.);
#11882=ORIENTED_EDGE('',*,*,#7914,.F.);
#11883=ORIENTED_EDGE('',*,*,#7915,.T.);
#11884=ORIENTED_EDGE('',*,*,#8122,.T.);
#11885=ORIENTED_EDGE('',*,*,#7945,.T.);
#11886=ORIENTED_EDGE('',*,*,#8119,.F.);
#11887=ORIENTED_EDGE('',*,*,#7917,.T.);
#11888=ORIENTED_EDGE('',*,*,#8120,.F.);
#11889=ORIENTED_EDGE('',*,*,#7943,.T.);
#11890=ORIENTED_EDGE('',*,*,#8121,.T.);
#11891=ORIENTED_EDGE('',*,*,#7929,.T.);
#11892=ORIENTED_EDGE('',*,*,#8123,.F.);
#11893=ORIENTED_EDGE('',*,*,#7925,.T.);
#11894=ORIENTED_EDGE('',*,*,#8124,.T.);
#11895=ORIENTED_EDGE('',*,*,#7931,.T.);
#11896=ORIENTED_EDGE('',*,*,#8125,.T.);
#11897=ORIENTED_EDGE('',*,*,#7923,.T.);
#11898=ORIENTED_EDGE('',*,*,#8126,.F.);
#11899=ORIENTED_EDGE('',*,*,#7928,.T.);
#11900=ORIENTED_EDGE('',*,*,#7932,.T.);
#11901=ORIENTED_EDGE('',*,*,#8126,.T.);
#11902=ORIENTED_EDGE('',*,*,#7922,.T.);
#11903=ORIENTED_EDGE('',*,*,#7926,.T.);
#11904=ORIENTED_EDGE('',*,*,#8123,.T.);
#11905=ORIENTED_EDGE('',*,*,#8124,.F.);
#11906=ORIENTED_EDGE('',*,*,#7924,.F.);
#11907=ORIENTED_EDGE('',*,*,#8125,.F.);
#11908=ORIENTED_EDGE('',*,*,#7930,.F.);
#11909=ORIENTED_EDGE('',*,*,#7913,.T.);
#11910=ORIENTED_EDGE('',*,*,#7933,.F.);
#11911=ORIENTED_EDGE('',*,*,#7911,.F.);
#11912=ORIENTED_EDGE('',*,*,#7934,.T.);
#11913=ORIENTED_EDGE('',*,*,#8073,.T.);
#11914=ORIENTED_EDGE('',*,*,#8127,.T.);
#11915=ORIENTED_EDGE('',*,*,#7920,.T.);
#11916=ORIENTED_EDGE('',*,*,#8128,.T.);
#11917=ORIENTED_EDGE('',*,*,#8129,.F.);
#11918=ORIENTED_EDGE('',*,*,#7918,.F.);
#11919=ORIENTED_EDGE('',*,*,#8130,.F.);
#11920=ORIENTED_EDGE('',*,*,#8071,.F.);
#11921=ORIENTED_EDGE('',*,*,#8072,.T.);
#11922=ORIENTED_EDGE('',*,*,#8130,.T.);
#11923=ORIENTED_EDGE('',*,*,#7921,.T.);
#11924=ORIENTED_EDGE('',*,*,#8127,.F.);
#11925=ORIENTED_EDGE('',*,*,#8074,.T.);
#11926=ORIENTED_EDGE('',*,*,#8128,.F.);
#11927=ORIENTED_EDGE('',*,*,#7919,.T.);
#11928=ORIENTED_EDGE('',*,*,#8129,.T.);
#11929=ORIENTED_EDGE('',*,*,#8051,.T.);
#11930=ORIENTED_EDGE('',*,*,#8131,.F.);
#11931=ORIENTED_EDGE('',*,*,#8046,.F.);
#11932=ORIENTED_EDGE('',*,*,#8132,.F.);
#11933=ORIENTED_EDGE('',*,*,#8133,.T.);
#11934=ORIENTED_EDGE('',*,*,#8044,.T.);
#11935=ORIENTED_EDGE('',*,*,#8048,.T.);
#11936=ORIENTED_EDGE('',*,*,#8134,.T.);
#11937=ORIENTED_EDGE('',*,*,#8049,.F.);
#11938=ORIENTED_EDGE('',*,*,#8042,.F.);
#11939=ORIENTED_EDGE('',*,*,#8134,.F.);
#11940=ORIENTED_EDGE('',*,*,#8047,.T.);
#11941=ORIENTED_EDGE('',*,*,#8131,.T.);
#11942=ORIENTED_EDGE('',*,*,#8050,.F.);
#11943=ORIENTED_EDGE('',*,*,#8132,.T.);
#11944=ORIENTED_EDGE('',*,*,#8045,.T.);
#11945=ORIENTED_EDGE('',*,*,#8133,.F.);
#11946=ORIENTED_EDGE('',*,*,#8052,.F.);
#11947=ORIENTED_EDGE('',*,*,#8135,.F.);
#11948=ORIENTED_EDGE('',*,*,#8136,.T.);
#11949=ORIENTED_EDGE('',*,*,#8137,.F.);
#11950=ORIENTED_EDGE('',*,*,#8136,.F.);
#11951=ORIENTED_EDGE('',*,*,#8138,.F.);
#11952=ORIENTED_EDGE('',*,*,#8139,.F.);
#11953=ORIENTED_EDGE('',*,*,#8140,.F.);
#11954=ORIENTED_EDGE('',*,*,#8141,.F.);
#11955=ORIENTED_EDGE('',*,*,#8142,.T.);
#11956=ORIENTED_EDGE('',*,*,#8135,.T.);
#11957=ORIENTED_EDGE('',*,*,#8142,.F.);
#11958=ORIENTED_EDGE('',*,*,#8143,.T.);
#11959=ORIENTED_EDGE('',*,*,#8144,.F.);
#11960=ORIENTED_EDGE('',*,*,#8143,.F.);
#11961=ORIENTED_EDGE('',*,*,#8145,.T.);
#11962=ORIENTED_EDGE('',*,*,#8146,.T.);
#11963=ORIENTED_EDGE('',*,*,#8147,.T.);
#11964=ORIENTED_EDGE('',*,*,#8148,.T.);
#11965=ORIENTED_EDGE('',*,*,#8144,.T.);
#11966=ORIENTED_EDGE('',*,*,#8137,.T.);
#11967=ORIENTED_EDGE('',*,*,#8148,.F.);
#11968=ORIENTED_EDGE('',*,*,#8149,.T.);
#11969=ORIENTED_EDGE('',*,*,#8139,.T.);
#11970=ORIENTED_EDGE('',*,*,#8150,.F.);
#11971=ORIENTED_EDGE('',*,*,#8145,.F.);
#11972=ORIENTED_EDGE('',*,*,#8150,.T.);
#11973=ORIENTED_EDGE('',*,*,#8138,.T.);
#11974=ORIENTED_EDGE('',*,*,#8151,.F.);
#11975=ORIENTED_EDGE('',*,*,#8147,.F.);
#11976=ORIENTED_EDGE('',*,*,#8152,.T.);
#11977=ORIENTED_EDGE('',*,*,#8140,.T.);
#11978=ORIENTED_EDGE('',*,*,#8149,.F.);
#11979=ORIENTED_EDGE('',*,*,#8146,.F.);
#11980=ORIENTED_EDGE('',*,*,#8151,.T.);
#11981=ORIENTED_EDGE('',*,*,#8141,.T.);
#11982=ORIENTED_EDGE('',*,*,#8152,.F.);
#11983=ORIENTED_EDGE('',*,*,#8153,.F.);
#11984=ORIENTED_EDGE('',*,*,#8154,.T.);
#11985=ORIENTED_EDGE('',*,*,#8155,.F.);
#11986=ORIENTED_EDGE('',*,*,#8154,.F.);
#11987=ORIENTED_EDGE('',*,*,#8156,.F.);
#11988=ORIENTED_EDGE('',*,*,#8157,.T.);
#11989=ORIENTED_EDGE('',*,*,#8158,.F.);
#11990=ORIENTED_EDGE('',*,*,#8157,.F.);
#11991=ORIENTED_EDGE('',*,*,#8159,.F.);
#11992=ORIENTED_EDGE('',*,*,#8160,.F.);
#11993=ORIENTED_EDGE('',*,*,#8161,.F.);
#11994=ORIENTED_EDGE('',*,*,#8162,.F.);
#11995=ORIENTED_EDGE('',*,*,#8155,.T.);
#11996=ORIENTED_EDGE('',*,*,#8158,.T.);
#11997=ORIENTED_EDGE('',*,*,#8160,.T.);
#11998=ORIENTED_EDGE('',*,*,#8163,.T.);
#11999=ORIENTED_EDGE('',*,*,#8164,.F.);
#12000=ORIENTED_EDGE('',*,*,#8165,.F.);
#12001=ORIENTED_EDGE('',*,*,#8159,.T.);
#12002=ORIENTED_EDGE('',*,*,#8166,.T.);
#12003=ORIENTED_EDGE('',*,*,#8167,.F.);
#12004=ORIENTED_EDGE('',*,*,#8163,.F.);
#12005=ORIENTED_EDGE('',*,*,#8161,.T.);
#12006=ORIENTED_EDGE('',*,*,#8165,.T.);
#12007=ORIENTED_EDGE('',*,*,#8168,.F.);
#12008=ORIENTED_EDGE('',*,*,#8169,.F.);
#12009=ORIENTED_EDGE('',*,*,#8162,.T.);
#12010=ORIENTED_EDGE('',*,*,#8169,.T.);
#12011=ORIENTED_EDGE('',*,*,#8170,.F.);
#12012=ORIENTED_EDGE('',*,*,#8166,.F.);
#12013=ORIENTED_EDGE('',*,*,#8167,.T.);
#12014=ORIENTED_EDGE('',*,*,#8170,.T.);
#12015=ORIENTED_EDGE('',*,*,#8168,.T.);
#12016=ORIENTED_EDGE('',*,*,#8164,.T.);
#12017=ORIENTED_EDGE('',*,*,#8153,.T.);
#12018=ORIENTED_EDGE('',*,*,#8156,.T.);
#12019=CYLINDRICAL_SURFACE('',#13186,7.5);
#12020=CYLINDRICAL_SURFACE('',#13189,7.5);
#12021=CYLINDRICAL_SURFACE('',#13194,1.);
#12022=CYLINDRICAL_SURFACE('',#13198,1.);
#12023=CYLINDRICAL_SURFACE('',#13202,1.);
#12024=CYLINDRICAL_SURFACE('',#13206,1.);
#12025=CYLINDRICAL_SURFACE('',#13210,1.);
#12026=CYLINDRICAL_SURFACE('',#13214,1.);
#12027=CYLINDRICAL_SURFACE('',#13218,1.);
#12028=CYLINDRICAL_SURFACE('',#13222,1.);
#12029=CYLINDRICAL_SURFACE('',#13226,1.);
#12030=CYLINDRICAL_SURFACE('',#13230,1.);
#12031=CYLINDRICAL_SURFACE('',#13234,1.);
#12032=CYLINDRICAL_SURFACE('',#13238,1.);
#12033=CYLINDRICAL_SURFACE('',#13242,1.);
#12034=CYLINDRICAL_SURFACE('',#13246,1.);
#12035=CYLINDRICAL_SURFACE('',#13250,1.);
#12036=CYLINDRICAL_SURFACE('',#13254,1.);
#12037=CYLINDRICAL_SURFACE('',#13258,1.);
#12038=CYLINDRICAL_SURFACE('',#13262,1.);
#12039=CYLINDRICAL_SURFACE('',#13266,1.);
#12040=CYLINDRICAL_SURFACE('',#13270,1.);
#12041=CYLINDRICAL_SURFACE('',#13274,1.);
#12042=CYLINDRICAL_SURFACE('',#13278,1.);
#12043=CYLINDRICAL_SURFACE('',#13282,1.);
#12044=CYLINDRICAL_SURFACE('',#13286,1.);
#12045=CYLINDRICAL_SURFACE('',#13290,1.);
#12046=CYLINDRICAL_SURFACE('',#13294,1.);
#12047=CYLINDRICAL_SURFACE('',#13298,1.);
#12048=CYLINDRICAL_SURFACE('',#13302,1.);
#12049=CYLINDRICAL_SURFACE('',#13306,1.);
#12050=CYLINDRICAL_SURFACE('',#13310,1.);
#12051=CYLINDRICAL_SURFACE('',#13314,1.);
#12052=CYLINDRICAL_SURFACE('',#13318,1.);
#12053=CYLINDRICAL_SURFACE('',#13322,1.);
#12054=CYLINDRICAL_SURFACE('',#13326,1.);
#12055=CYLINDRICAL_SURFACE('',#13330,1.);
#12056=CYLINDRICAL_SURFACE('',#13334,1.);
#12057=CYLINDRICAL_SURFACE('',#13338,1.);
#12058=CYLINDRICAL_SURFACE('',#13342,1.);
#12059=CYLINDRICAL_SURFACE('',#13346,43.9999999999887);
#12060=CYLINDRICAL_SURFACE('',#13349,43.9999999999887);
#12061=CYLINDRICAL_SURFACE('',#13352,43.9999999999887);
#12062=CYLINDRICAL_SURFACE('',#13355,43.9999999999887);
#12063=CYLINDRICAL_SURFACE('',#13358,43.9999999999887);
#12064=CYLINDRICAL_SURFACE('',#13361,43.9999999999887);
#12065=CYLINDRICAL_SURFACE('',#13364,43.9999999999887);
#12066=CYLINDRICAL_SURFACE('',#13367,43.9999999999887);
#12067=CYLINDRICAL_SURFACE('',#13370,43.9999999999887);
#12068=CYLINDRICAL_SURFACE('',#13373,43.9999999999887);
#12069=CYLINDRICAL_SURFACE('',#13376,43.9999999999887);
#12070=CYLINDRICAL_SURFACE('',#13379,43.9999999999887);
#12071=CYLINDRICAL_SURFACE('',#13382,43.9999999999887);
#12072=CYLINDRICAL_SURFACE('',#13385,43.9999999999887);
#12073=CYLINDRICAL_SURFACE('',#13388,43.9999999999887);
#12074=CYLINDRICAL_SURFACE('',#13391,43.9999999999887);
#12075=CYLINDRICAL_SURFACE('',#13394,43.9999999999887);
#12076=CYLINDRICAL_SURFACE('',#13397,43.9999999999887);
#12077=CYLINDRICAL_SURFACE('',#13400,43.9999999999887);
#12078=CYLINDRICAL_SURFACE('',#13451,35.372);
#12079=CYLINDRICAL_SURFACE('',#13452,35.372);
#12080=CYLINDRICAL_SURFACE('',#13453,35.372);
#12081=CYLINDRICAL_SURFACE('',#13454,35.372);
#12082=CYLINDRICAL_SURFACE('',#13455,35.372);
#12083=CYLINDRICAL_SURFACE('',#13456,35.372);
#12084=CYLINDRICAL_SURFACE('',#13457,35.372);
#12085=CYLINDRICAL_SURFACE('',#13458,35.372);
#12086=CYLINDRICAL_SURFACE('',#13459,35.372);
#12087=CYLINDRICAL_SURFACE('',#13460,35.372);
#12088=CYLINDRICAL_SURFACE('',#13461,35.372);
#12089=CYLINDRICAL_SURFACE('',#13462,35.372);
#12090=CYLINDRICAL_SURFACE('',#13463,35.372);
#12091=CYLINDRICAL_SURFACE('',#13464,35.372);
#12092=CYLINDRICAL_SURFACE('',#13465,35.372);
#12093=CYLINDRICAL_SURFACE('',#13466,35.372);
#12094=CYLINDRICAL_SURFACE('',#13467,35.372);
#12095=CYLINDRICAL_SURFACE('',#13468,35.372);
#12096=CYLINDRICAL_SURFACE('',#13469,35.372);
#12097=CYLINDRICAL_SURFACE('',#13470,1.);
#12098=CYLINDRICAL_SURFACE('',#13472,1.);
#12099=CYLINDRICAL_SURFACE('',#13474,43.9999999999887);
#12100=CYLINDRICAL_SURFACE('',#13475,35.372);
#12101=CYLINDRICAL_SURFACE('',#13477,7.50000000000001);
#12102=CYLINDRICAL_SURFACE('',#13480,7.50000000000001);
#12103=CYLINDRICAL_SURFACE('',#13485,1.);
#12104=CYLINDRICAL_SURFACE('',#13489,1.);
#12105=CYLINDRICAL_SURFACE('',#13493,1.);
#12106=CYLINDRICAL_SURFACE('',#13497,1.);
#12107=CYLINDRICAL_SURFACE('',#13501,1.);
#12108=CYLINDRICAL_SURFACE('',#13505,1.);
#12109=CYLINDRICAL_SURFACE('',#13509,1.);
#12110=CYLINDRICAL_SURFACE('',#13513,1.);
#12111=CYLINDRICAL_SURFACE('',#13517,1.);
#12112=CYLINDRICAL_SURFACE('',#13521,1.);
#12113=CYLINDRICAL_SURFACE('',#13525,1.);
#12114=CYLINDRICAL_SURFACE('',#13529,1.);
#12115=CYLINDRICAL_SURFACE('',#13533,1.);
#12116=CYLINDRICAL_SURFACE('',#13537,1.);
#12117=CYLINDRICAL_SURFACE('',#13541,1.);
#12118=CYLINDRICAL_SURFACE('',#13545,1.);
#12119=CYLINDRICAL_SURFACE('',#13549,1.);
#12120=CYLINDRICAL_SURFACE('',#13553,1.);
#12121=CYLINDRICAL_SURFACE('',#13557,23.9999999999999);
#12122=CYLINDRICAL_SURFACE('',#13560,23.9999999999999);
#12123=CYLINDRICAL_SURFACE('',#13563,23.9999999999999);
#12124=CYLINDRICAL_SURFACE('',#13566,23.9999999999999);
#12125=CYLINDRICAL_SURFACE('',#13569,23.9999999999999);
#12126=CYLINDRICAL_SURFACE('',#13572,23.9999999999999);
#12127=CYLINDRICAL_SURFACE('',#13575,23.9999999999999);
#12128=CYLINDRICAL_SURFACE('',#13578,23.9999999999999);
#12129=CYLINDRICAL_SURFACE('',#13581,23.9999999999999);
#12130=CYLINDRICAL_SURFACE('',#13612,15.372);
#12131=CYLINDRICAL_SURFACE('',#13613,15.372);
#12132=CYLINDRICAL_SURFACE('',#13614,15.372);
#12133=CYLINDRICAL_SURFACE('',#13615,15.372);
#12134=CYLINDRICAL_SURFACE('',#13616,15.372);
#12135=CYLINDRICAL_SURFACE('',#13617,15.372);
#12136=CYLINDRICAL_SURFACE('',#13618,15.372);
#12137=CYLINDRICAL_SURFACE('',#13619,15.372);
#12138=CYLINDRICAL_SURFACE('',#13620,15.372);
#12139=CYLINDRICAL_SURFACE('',#13621,1.);
#12140=CYLINDRICAL_SURFACE('',#13623,1.);
#12141=CYLINDRICAL_SURFACE('',#13625,23.9999999999999);
#12142=CYLINDRICAL_SURFACE('',#13626,15.372);
#12143=CYLINDRICAL_SURFACE('',#13645,7.5);
#12144=CYLINDRICAL_SURFACE('',#13648,12.4653846153846);
#12145=CYLINDRICAL_SURFACE('',#13650,12.4653846153846);
#12146=CYLINDRICAL_SURFACE('',#13686,17.6897435897436);
#12147=CYLINDRICAL_SURFACE('',#13689,16.2686153846154);
#12148=CYLINDRICAL_SURFACE('',#13691,16.0346153846154);
#12149=CYLINDRICAL_SURFACE('',#13696,16.0346153846154);
#12150=CYLINDRICAL_SURFACE('',#13697,16.2686153846154);
#12151=CYLINDRICAL_SURFACE('',#13699,17.6897435897436);
#12152=CYLINDRICAL_SURFACE('',#13709,21.);
#12153=CYLINDRICAL_SURFACE('',#13814,14.25);
#12154=CYLINDRICAL_SURFACE('',#13817,15.1423076923077);
#12155=CYLINDRICAL_SURFACE('',#13830,15.1423076923077);
#12156=CYLINDRICAL_SURFACE('',#13831,14.25);
#12157=CYLINDRICAL_SURFACE('',#13840,15.1423076923077);
#12158=CYLINDRICAL_SURFACE('',#13841,14.25);
#12159=CYLINDRICAL_SURFACE('',#13842,14.25);
#12160=CYLINDRICAL_SURFACE('',#13845,15.1423076923077);
#12161=CYLINDRICAL_SURFACE('',#13858,15.1423076923077);
#12162=CYLINDRICAL_SURFACE('',#13859,14.25);
#12163=CYLINDRICAL_SURFACE('',#13860,14.25);
#12164=CYLINDRICAL_SURFACE('',#13863,15.1423076923077);
#12165=CYLINDRICAL_SURFACE('',#13876,15.1423076923077);
#12166=CYLINDRICAL_SURFACE('',#13877,14.25);
#12167=CYLINDRICAL_SURFACE('',#13878,14.25);
#12168=CYLINDRICAL_SURFACE('',#13881,15.1423076923077);
#12169=CYLINDRICAL_SURFACE('',#13894,15.1423076923077);
#12170=CYLINDRICAL_SURFACE('',#13895,14.25);
#12171=CYLINDRICAL_SURFACE('',#13896,14.25);
#12172=CYLINDRICAL_SURFACE('',#13899,15.1423076923077);
#12173=CYLINDRICAL_SURFACE('',#13912,15.1423076923077);
#12174=CYLINDRICAL_SURFACE('',#13913,14.25);
#12175=CYLINDRICAL_SURFACE('',#13914,14.25);
#12176=CYLINDRICAL_SURFACE('',#13917,15.1423076923077);
#12177=CYLINDRICAL_SURFACE('',#13930,15.1423076923077);
#12178=CYLINDRICAL_SURFACE('',#13931,14.25);
#12179=CYLINDRICAL_SURFACE('',#13938,15.1423076923077);
#12180=CYLINDRICAL_SURFACE('',#13939,14.25);
#12181=CYLINDRICAL_SURFACE('',#13958,7.5);
#12182=CYLINDRICAL_SURFACE('',#13961,12.4653846153846);
#12183=CYLINDRICAL_SURFACE('',#13963,12.4653846153846);
#12184=CYLINDRICAL_SURFACE('',#13999,17.6897435897436);
#12185=CYLINDRICAL_SURFACE('',#14002,16.2686153846154);
#12186=CYLINDRICAL_SURFACE('',#14004,16.0346153846154);
#12187=CYLINDRICAL_SURFACE('',#14009,16.0346153846154);
#12188=CYLINDRICAL_SURFACE('',#14010,16.2686153846154);
#12189=CYLINDRICAL_SURFACE('',#14012,17.6897435897436);
#12190=CYLINDRICAL_SURFACE('',#14022,21.);
#12191=CYLINDRICAL_SURFACE('',#14127,14.25);
#12192=CYLINDRICAL_SURFACE('',#14130,15.1423076923077);
#12193=CYLINDRICAL_SURFACE('',#14143,15.1423076923077);
#12194=CYLINDRICAL_SURFACE('',#14144,14.25);
#12195=CYLINDRICAL_SURFACE('',#14153,15.1423076923077);
#12196=CYLINDRICAL_SURFACE('',#14154,14.25);
#12197=CYLINDRICAL_SURFACE('',#14155,14.25);
#12198=CYLINDRICAL_SURFACE('',#14158,15.1423076923077);
#12199=CYLINDRICAL_SURFACE('',#14171,15.1423076923077);
#12200=CYLINDRICAL_SURFACE('',#14172,14.25);
#12201=CYLINDRICAL_SURFACE('',#14173,14.25);
#12202=CYLINDRICAL_SURFACE('',#14176,15.1423076923077);
#12203=CYLINDRICAL_SURFACE('',#14189,15.1423076923077);
#12204=CYLINDRICAL_SURFACE('',#14190,14.25);
#12205=CYLINDRICAL_SURFACE('',#14191,14.25);
#12206=CYLINDRICAL_SURFACE('',#14194,15.1423076923077);
#12207=CYLINDRICAL_SURFACE('',#14207,15.1423076923077);
#12208=CYLINDRICAL_SURFACE('',#14208,14.25);
#12209=CYLINDRICAL_SURFACE('',#14209,14.25);
#12210=CYLINDRICAL_SURFACE('',#14212,15.1423076923077);
#12211=CYLINDRICAL_SURFACE('',#14225,15.1423076923077);
#12212=CYLINDRICAL_SURFACE('',#14226,14.25);
#12213=CYLINDRICAL_SURFACE('',#14227,14.25);
#12214=CYLINDRICAL_SURFACE('',#14230,15.1423076923077);
#12215=CYLINDRICAL_SURFACE('',#14243,15.1423076923077);
#12216=CYLINDRICAL_SURFACE('',#14244,14.25);
#12217=CYLINDRICAL_SURFACE('',#14251,15.1423076923077);
#12218=CYLINDRICAL_SURFACE('',#14252,14.25);
#12219=CYLINDRICAL_SURFACE('',#14271,7.5);
#12220=CYLINDRICAL_SURFACE('',#14274,12.4653846153846);
#12221=CYLINDRICAL_SURFACE('',#14276,12.4653846153846);
#12222=CYLINDRICAL_SURFACE('',#14312,17.6897435897436);
#12223=CYLINDRICAL_SURFACE('',#14315,16.2686153846154);
#12224=CYLINDRICAL_SURFACE('',#14317,16.0346153846154);
#12225=CYLINDRICAL_SURFACE('',#14322,16.0346153846154);
#12226=CYLINDRICAL_SURFACE('',#14323,16.2686153846154);
#12227=CYLINDRICAL_SURFACE('',#14325,17.6897435897436);
#12228=CYLINDRICAL_SURFACE('',#14335,21.);
#12229=CYLINDRICAL_SURFACE('',#14440,14.25);
#12230=CYLINDRICAL_SURFACE('',#14443,15.1423076923077);
#12231=CYLINDRICAL_SURFACE('',#14456,15.1423076923077);
#12232=CYLINDRICAL_SURFACE('',#14457,14.25);
#12233=CYLINDRICAL_SURFACE('',#14466,15.1423076923077);
#12234=CYLINDRICAL_SURFACE('',#14467,14.25);
#12235=CYLINDRICAL_SURFACE('',#14468,14.25);
#12236=CYLINDRICAL_SURFACE('',#14471,15.1423076923077);
#12237=CYLINDRICAL_SURFACE('',#14484,15.1423076923077);
#12238=CYLINDRICAL_SURFACE('',#14485,14.25);
#12239=CYLINDRICAL_SURFACE('',#14486,14.25);
#12240=CYLINDRICAL_SURFACE('',#14489,15.1423076923077);
#12241=CYLINDRICAL_SURFACE('',#14502,15.1423076923077);
#12242=CYLINDRICAL_SURFACE('',#14503,14.25);
#12243=CYLINDRICAL_SURFACE('',#14504,14.25);
#12244=CYLINDRICAL_SURFACE('',#14507,15.1423076923077);
#12245=CYLINDRICAL_SURFACE('',#14520,15.1423076923077);
#12246=CYLINDRICAL_SURFACE('',#14521,14.25);
#12247=CYLINDRICAL_SURFACE('',#14522,14.25);
#12248=CYLINDRICAL_SURFACE('',#14525,15.1423076923077);
#12249=CYLINDRICAL_SURFACE('',#14538,15.1423076923077);
#12250=CYLINDRICAL_SURFACE('',#14539,14.25);
#12251=CYLINDRICAL_SURFACE('',#14540,14.25);
#12252=CYLINDRICAL_SURFACE('',#14543,15.1423076923077);
#12253=CYLINDRICAL_SURFACE('',#14556,15.1423076923077);
#12254=CYLINDRICAL_SURFACE('',#14557,14.25);
#12255=CYLINDRICAL_SURFACE('',#14564,15.1423076923077);
#12256=CYLINDRICAL_SURFACE('',#14565,14.25);
#12257=CYLINDRICAL_SURFACE('',#14584,7.5);
#12258=CYLINDRICAL_SURFACE('',#14587,12.4653846153846);
#12259=CYLINDRICAL_SURFACE('',#14589,12.4653846153846);
#12260=CYLINDRICAL_SURFACE('',#14625,17.6897435897436);
#12261=CYLINDRICAL_SURFACE('',#14628,16.2686153846154);
#12262=CYLINDRICAL_SURFACE('',#14630,16.0346153846154);
#12263=CYLINDRICAL_SURFACE('',#14635,16.0346153846154);
#12264=CYLINDRICAL_SURFACE('',#14636,16.2686153846154);
#12265=CYLINDRICAL_SURFACE('',#14638,17.6897435897436);
#12266=CYLINDRICAL_SURFACE('',#14648,21.);
#12267=CYLINDRICAL_SURFACE('',#14753,14.25);
#12268=CYLINDRICAL_SURFACE('',#14756,15.1423076923077);
#12269=CYLINDRICAL_SURFACE('',#14769,15.1423076923077);
#12270=CYLINDRICAL_SURFACE('',#14770,14.25);
#12271=CYLINDRICAL_SURFACE('',#14779,15.1423076923077);
#12272=CYLINDRICAL_SURFACE('',#14780,14.25);
#12273=CYLINDRICAL_SURFACE('',#14781,14.25);
#12274=CYLINDRICAL_SURFACE('',#14784,15.1423076923077);
#12275=CYLINDRICAL_SURFACE('',#14797,15.1423076923077);
#12276=CYLINDRICAL_SURFACE('',#14798,14.25);
#12277=CYLINDRICAL_SURFACE('',#14799,14.25);
#12278=CYLINDRICAL_SURFACE('',#14802,15.1423076923077);
#12279=CYLINDRICAL_SURFACE('',#14815,15.1423076923077);
#12280=CYLINDRICAL_SURFACE('',#14816,14.25);
#12281=CYLINDRICAL_SURFACE('',#14817,14.25);
#12282=CYLINDRICAL_SURFACE('',#14820,15.1423076923077);
#12283=CYLINDRICAL_SURFACE('',#14833,15.1423076923077);
#12284=CYLINDRICAL_SURFACE('',#14834,14.25);
#12285=CYLINDRICAL_SURFACE('',#14835,14.25);
#12286=CYLINDRICAL_SURFACE('',#14838,15.1423076923077);
#12287=CYLINDRICAL_SURFACE('',#14851,15.1423076923077);
#12288=CYLINDRICAL_SURFACE('',#14852,14.25);
#12289=CYLINDRICAL_SURFACE('',#14853,14.25);
#12290=CYLINDRICAL_SURFACE('',#14856,15.1423076923077);
#12291=CYLINDRICAL_SURFACE('',#14869,15.1423076923077);
#12292=CYLINDRICAL_SURFACE('',#14870,14.25);
#12293=CYLINDRICAL_SURFACE('',#14877,15.1423076923077);
#12294=CYLINDRICAL_SURFACE('',#14878,14.25);
#12295=CYLINDRICAL_SURFACE('',#14880,21.);
#12296=CYLINDRICAL_SURFACE('',#14885,21.);
#12297=CYLINDRICAL_SURFACE('',#14893,21.);
#12298=CYLINDRICAL_SURFACE('',#14896,21.);
#12299=ADVANCED_FACE('',(#1287),#12019,.T.);
#12300=ADVANCED_FACE('',(#1288),#12020,.T.);
#12301=ADVANCED_FACE('',(#1289),#1007,.F.);
#12302=ADVANCED_FACE('',(#1290),#1008,.T.);
#12303=ADVANCED_FACE('',(#1291),#12021,.F.);
#12304=ADVANCED_FACE('',(#1292),#1009,.T.);
#12305=ADVANCED_FACE('',(#1293),#12022,.F.);
#12306=ADVANCED_FACE('',(#1294),#1010,.T.);
#12307=ADVANCED_FACE('',(#1295),#12023,.F.);
#12308=ADVANCED_FACE('',(#1296),#1011,.T.);
#12309=ADVANCED_FACE('',(#1297),#12024,.F.);
#12310=ADVANCED_FACE('',(#1298),#1012,.T.);
#12311=ADVANCED_FACE('',(#1299),#12025,.F.);
#12312=ADVANCED_FACE('',(#1300),#1013,.T.);
#12313=ADVANCED_FACE('',(#1301),#12026,.F.);
#12314=ADVANCED_FACE('',(#1302),#1014,.T.);
#12315=ADVANCED_FACE('',(#1303),#12027,.F.);
#12316=ADVANCED_FACE('',(#1304),#1015,.T.);
#12317=ADVANCED_FACE('',(#1305),#12028,.F.);
#12318=ADVANCED_FACE('',(#1306),#1016,.T.);
#12319=ADVANCED_FACE('',(#1307),#12029,.F.);
#12320=ADVANCED_FACE('',(#1308),#1017,.T.);
#12321=ADVANCED_FACE('',(#1309),#12030,.F.);
#12322=ADVANCED_FACE('',(#1310),#1018,.T.);
#12323=ADVANCED_FACE('',(#1311),#12031,.F.);
#12324=ADVANCED_FACE('',(#1312),#1019,.T.);
#12325=ADVANCED_FACE('',(#1313),#12032,.F.);
#12326=ADVANCED_FACE('',(#1314),#1020,.T.);
#12327=ADVANCED_FACE('',(#1315),#12033,.F.);
#12328=ADVANCED_FACE('',(#1316),#1021,.T.);
#12329=ADVANCED_FACE('',(#1317),#12034,.F.);
#12330=ADVANCED_FACE('',(#1318),#1022,.T.);
#12331=ADVANCED_FACE('',(#1319),#12035,.F.);
#12332=ADVANCED_FACE('',(#1320),#1023,.T.);
#12333=ADVANCED_FACE('',(#1321),#12036,.F.);
#12334=ADVANCED_FACE('',(#1322),#1024,.T.);
#12335=ADVANCED_FACE('',(#1323),#12037,.F.);
#12336=ADVANCED_FACE('',(#1324),#1025,.T.);
#12337=ADVANCED_FACE('',(#1325),#12038,.F.);
#12338=ADVANCED_FACE('',(#1326),#1026,.T.);
#12339=ADVANCED_FACE('',(#1327),#12039,.F.);
#12340=ADVANCED_FACE('',(#1328),#1027,.T.);
#12341=ADVANCED_FACE('',(#1329),#12040,.F.);
#12342=ADVANCED_FACE('',(#1330),#1028,.T.);
#12343=ADVANCED_FACE('',(#1331),#12041,.F.);
#12344=ADVANCED_FACE('',(#1332),#1029,.T.);
#12345=ADVANCED_FACE('',(#1333),#12042,.F.);
#12346=ADVANCED_FACE('',(#1334),#1030,.T.);
#12347=ADVANCED_FACE('',(#1335),#12043,.F.);
#12348=ADVANCED_FACE('',(#1336),#1031,.T.);
#12349=ADVANCED_FACE('',(#1337),#12044,.F.);
#12350=ADVANCED_FACE('',(#1338),#1032,.T.);
#12351=ADVANCED_FACE('',(#1339),#12045,.F.);
#12352=ADVANCED_FACE('',(#1340),#1033,.T.);
#12353=ADVANCED_FACE('',(#1341),#12046,.F.);
#12354=ADVANCED_FACE('',(#1342),#1034,.T.);
#12355=ADVANCED_FACE('',(#1343),#12047,.F.);
#12356=ADVANCED_FACE('',(#1344),#1035,.T.);
#12357=ADVANCED_FACE('',(#1345),#12048,.F.);
#12358=ADVANCED_FACE('',(#1346),#1036,.T.);
#12359=ADVANCED_FACE('',(#1347),#12049,.F.);
#12360=ADVANCED_FACE('',(#1348),#1037,.T.);
#12361=ADVANCED_FACE('',(#1349),#12050,.F.);
#12362=ADVANCED_FACE('',(#1350),#1038,.T.);
#12363=ADVANCED_FACE('',(#1351),#12051,.F.);
#12364=ADVANCED_FACE('',(#1352),#1039,.T.);
#12365=ADVANCED_FACE('',(#1353),#12052,.F.);
#12366=ADVANCED_FACE('',(#1354),#1040,.T.);
#12367=ADVANCED_FACE('',(#1355),#12053,.F.);
#12368=ADVANCED_FACE('',(#1356),#1041,.T.);
#12369=ADVANCED_FACE('',(#1357),#12054,.F.);
#12370=ADVANCED_FACE('',(#1358),#1042,.T.);
#12371=ADVANCED_FACE('',(#1359),#12055,.F.);
#12372=ADVANCED_FACE('',(#1360),#1043,.T.);
#12373=ADVANCED_FACE('',(#1361),#12056,.F.);
#12374=ADVANCED_FACE('',(#1362),#1044,.T.);
#12375=ADVANCED_FACE('',(#1363),#12057,.F.);
#12376=ADVANCED_FACE('',(#1364),#1045,.T.);
#12377=ADVANCED_FACE('',(#1365),#12058,.F.);
#12378=ADVANCED_FACE('',(#1366),#1046,.T.);
#12379=ADVANCED_FACE('',(#1367),#947,.T.);
#12380=ADVANCED_FACE('',(#1368),#12059,.T.);
#12381=ADVANCED_FACE('',(#1369),#948,.T.);
#12382=ADVANCED_FACE('',(#1370),#949,.T.);
#12383=ADVANCED_FACE('',(#1371),#12060,.T.);
#12384=ADVANCED_FACE('',(#1372),#950,.T.);
#12385=ADVANCED_FACE('',(#1373),#951,.T.);
#12386=ADVANCED_FACE('',(#1374),#12061,.T.);
#12387=ADVANCED_FACE('',(#1375),#952,.T.);
#12388=ADVANCED_FACE('',(#1376),#953,.T.);
#12389=ADVANCED_FACE('',(#1377),#12062,.T.);
#12390=ADVANCED_FACE('',(#1378),#954,.T.);
#12391=ADVANCED_FACE('',(#1379),#955,.T.);
#12392=ADVANCED_FACE('',(#1380),#12063,.T.);
#12393=ADVANCED_FACE('',(#1381),#956,.T.);
#12394=ADVANCED_FACE('',(#1382),#957,.T.);
#12395=ADVANCED_FACE('',(#1383),#12064,.T.);
#12396=ADVANCED_FACE('',(#1384),#958,.T.);
#12397=ADVANCED_FACE('',(#1385),#959,.T.);
#12398=ADVANCED_FACE('',(#1386),#12065,.T.);
#12399=ADVANCED_FACE('',(#1387),#960,.T.);
#12400=ADVANCED_FACE('',(#1388),#961,.T.);
#12401=ADVANCED_FACE('',(#1389),#12066,.T.);
#12402=ADVANCED_FACE('',(#1390),#962,.T.);
#12403=ADVANCED_FACE('',(#1391),#963,.T.);
#12404=ADVANCED_FACE('',(#1392),#12067,.T.);
#12405=ADVANCED_FACE('',(#1393),#964,.T.);
#12406=ADVANCED_FACE('',(#1394),#965,.T.);
#12407=ADVANCED_FACE('',(#1395),#12068,.T.);
#12408=ADVANCED_FACE('',(#1396),#966,.T.);
#12409=ADVANCED_FACE('',(#1397),#967,.T.);
#12410=ADVANCED_FACE('',(#1398),#12069,.T.);
#12411=ADVANCED_FACE('',(#1399),#968,.T.);
#12412=ADVANCED_FACE('',(#1400),#969,.T.);
#12413=ADVANCED_FACE('',(#1401),#12070,.T.);
#12414=ADVANCED_FACE('',(#1402),#970,.T.);
#12415=ADVANCED_FACE('',(#1403),#971,.T.);
#12416=ADVANCED_FACE('',(#1404),#12071,.T.);
#12417=ADVANCED_FACE('',(#1405),#972,.T.);
#12418=ADVANCED_FACE('',(#1406),#973,.T.);
#12419=ADVANCED_FACE('',(#1407),#12072,.T.);
#12420=ADVANCED_FACE('',(#1408),#974,.T.);
#12421=ADVANCED_FACE('',(#1409),#975,.T.);
#12422=ADVANCED_FACE('',(#1410),#12073,.T.);
#12423=ADVANCED_FACE('',(#1411),#976,.T.);
#12424=ADVANCED_FACE('',(#1412),#977,.T.);
#12425=ADVANCED_FACE('',(#1413),#12074,.T.);
#12426=ADVANCED_FACE('',(#1414),#978,.T.);
#12427=ADVANCED_FACE('',(#1415),#979,.T.);
#12428=ADVANCED_FACE('',(#1416),#12075,.T.);
#12429=ADVANCED_FACE('',(#1417),#980,.T.);
#12430=ADVANCED_FACE('',(#1418),#981,.T.);
#12431=ADVANCED_FACE('',(#1419),#12076,.T.);
#12432=ADVANCED_FACE('',(#1420),#982,.T.);
#12433=ADVANCED_FACE('',(#1421),#983,.T.);
#12434=ADVANCED_FACE('',(#1422),#12077,.T.);
#12435=ADVANCED_FACE('',(#1423),#984,.T.);
#12436=ADVANCED_FACE('',(#1424,#279),#1047,.F.);
#12437=ADVANCED_FACE('',(#1425,#280),#1048,.T.);
#12438=ADVANCED_FACE('',(#1426),#12078,.T.);
#12439=ADVANCED_FACE('',(#1427),#12079,.T.);
#12440=ADVANCED_FACE('',(#1428),#12080,.T.);
#12441=ADVANCED_FACE('',(#1429),#12081,.T.);
#12442=ADVANCED_FACE('',(#1430),#12082,.T.);
#12443=ADVANCED_FACE('',(#1431),#12083,.T.);
#12444=ADVANCED_FACE('',(#1432),#12084,.T.);
#12445=ADVANCED_FACE('',(#1433),#12085,.T.);
#12446=ADVANCED_FACE('',(#1434),#12086,.T.);
#12447=ADVANCED_FACE('',(#1435),#12087,.T.);
#12448=ADVANCED_FACE('',(#1436),#12088,.T.);
#12449=ADVANCED_FACE('',(#1437),#12089,.T.);
#12450=ADVANCED_FACE('',(#1438),#12090,.T.);
#12451=ADVANCED_FACE('',(#1439),#12091,.T.);
#12452=ADVANCED_FACE('',(#1440),#12092,.T.);
#12453=ADVANCED_FACE('',(#1441),#12093,.T.);
#12454=ADVANCED_FACE('',(#1442),#12094,.T.);
#12455=ADVANCED_FACE('',(#1443),#12095,.T.);
#12456=ADVANCED_FACE('',(#1444),#12096,.T.);
#12457=ADVANCED_FACE('',(#1445),#12097,.F.);
#12458=ADVANCED_FACE('',(#1446),#1049,.T.);
#12459=ADVANCED_FACE('',(#1447),#12098,.F.);
#12460=ADVANCED_FACE('',(#1448),#1050,.T.);
#12461=ADVANCED_FACE('',(#1449),#985,.T.);
#12462=ADVANCED_FACE('',(#1450),#12099,.T.);
#12463=ADVANCED_FACE('',(#1451),#986,.T.);
#12464=ADVANCED_FACE('',(#1452),#12100,.T.);
#12465=ADVANCED_FACE('',(#1453),#12101,.T.);
#12466=ADVANCED_FACE('',(#1454),#12102,.T.);
#12467=ADVANCED_FACE('',(#1455),#1051,.F.);
#12468=ADVANCED_FACE('',(#1456),#1052,.T.);
#12469=ADVANCED_FACE('',(#1457),#12103,.F.);
#12470=ADVANCED_FACE('',(#1458),#1053,.T.);
#12471=ADVANCED_FACE('',(#1459),#12104,.F.);
#12472=ADVANCED_FACE('',(#1460),#1054,.T.);
#12473=ADVANCED_FACE('',(#1461),#12105,.F.);
#12474=ADVANCED_FACE('',(#1462),#1055,.T.);
#12475=ADVANCED_FACE('',(#1463),#12106,.F.);
#12476=ADVANCED_FACE('',(#1464),#1056,.T.);
#12477=ADVANCED_FACE('',(#1465),#12107,.F.);
#12478=ADVANCED_FACE('',(#1466),#1057,.T.);
#12479=ADVANCED_FACE('',(#1467),#12108,.F.);
#12480=ADVANCED_FACE('',(#1468),#1058,.T.);
#12481=ADVANCED_FACE('',(#1469),#12109,.F.);
#12482=ADVANCED_FACE('',(#1470),#1059,.T.);
#12483=ADVANCED_FACE('',(#1471),#12110,.F.);
#12484=ADVANCED_FACE('',(#1472),#1060,.T.);
#12485=ADVANCED_FACE('',(#1473),#12111,.F.);
#12486=ADVANCED_FACE('',(#1474),#1061,.T.);
#12487=ADVANCED_FACE('',(#1475),#12112,.F.);
#12488=ADVANCED_FACE('',(#1476),#1062,.T.);
#12489=ADVANCED_FACE('',(#1477),#12113,.F.);
#12490=ADVANCED_FACE('',(#1478),#1063,.T.);
#12491=ADVANCED_FACE('',(#1479),#12114,.F.);
#12492=ADVANCED_FACE('',(#1480),#1064,.T.);
#12493=ADVANCED_FACE('',(#1481),#12115,.F.);
#12494=ADVANCED_FACE('',(#1482),#1065,.T.);
#12495=ADVANCED_FACE('',(#1483),#12116,.F.);
#12496=ADVANCED_FACE('',(#1484),#1066,.T.);
#12497=ADVANCED_FACE('',(#1485),#12117,.F.);
#12498=ADVANCED_FACE('',(#1486),#1067,.T.);
#12499=ADVANCED_FACE('',(#1487),#12118,.F.);
#12500=ADVANCED_FACE('',(#1488),#1068,.T.);
#12501=ADVANCED_FACE('',(#1489),#12119,.F.);
#12502=ADVANCED_FACE('',(#1490),#1069,.T.);
#12503=ADVANCED_FACE('',(#1491),#12120,.F.);
#12504=ADVANCED_FACE('',(#1492),#1070,.T.);
#12505=ADVANCED_FACE('',(#1493),#987,.T.);
#12506=ADVANCED_FACE('',(#1494),#12121,.T.);
#12507=ADVANCED_FACE('',(#1495),#988,.T.);
#12508=ADVANCED_FACE('',(#1496),#989,.T.);
#12509=ADVANCED_FACE('',(#1497),#12122,.T.);
#12510=ADVANCED_FACE('',(#1498),#990,.T.);
#12511=ADVANCED_FACE('',(#1499),#991,.T.);
#12512=ADVANCED_FACE('',(#1500),#12123,.T.);
#12513=ADVANCED_FACE('',(#1501),#992,.T.);
#12514=ADVANCED_FACE('',(#1502),#993,.T.);
#12515=ADVANCED_FACE('',(#1503),#12124,.T.);
#12516=ADVANCED_FACE('',(#1504),#994,.T.);
#12517=ADVANCED_FACE('',(#1505),#995,.T.);
#12518=ADVANCED_FACE('',(#1506),#12125,.T.);
#12519=ADVANCED_FACE('',(#1507),#996,.T.);
#12520=ADVANCED_FACE('',(#1508),#997,.T.);
#12521=ADVANCED_FACE('',(#1509),#12126,.T.);
#12522=ADVANCED_FACE('',(#1510),#998,.T.);
#12523=ADVANCED_FACE('',(#1511),#999,.T.);
#12524=ADVANCED_FACE('',(#1512),#12127,.T.);
#12525=ADVANCED_FACE('',(#1513),#1000,.T.);
#12526=ADVANCED_FACE('',(#1514),#1001,.T.);
#12527=ADVANCED_FACE('',(#1515),#12128,.T.);
#12528=ADVANCED_FACE('',(#1516),#1002,.T.);
#12529=ADVANCED_FACE('',(#1517),#1003,.T.);
#12530=ADVANCED_FACE('',(#1518),#12129,.T.);
#12531=ADVANCED_FACE('',(#1519),#1004,.T.);
#12532=ADVANCED_FACE('',(#1520,#281),#1071,.F.);
#12533=ADVANCED_FACE('',(#1521,#282),#1072,.T.);
#12534=ADVANCED_FACE('',(#1522),#12130,.T.);
#12535=ADVANCED_FACE('',(#1523),#12131,.T.);
#12536=ADVANCED_FACE('',(#1524),#12132,.T.);
#12537=ADVANCED_FACE('',(#1525),#12133,.T.);
#12538=ADVANCED_FACE('',(#1526),#12134,.T.);
#12539=ADVANCED_FACE('',(#1527),#12135,.T.);
#12540=ADVANCED_FACE('',(#1528),#12136,.T.);
#12541=ADVANCED_FACE('',(#1529),#12137,.T.);
#12542=ADVANCED_FACE('',(#1530),#12138,.T.);
#12543=ADVANCED_FACE('',(#1531),#12139,.F.);
#12544=ADVANCED_FACE('',(#1532),#1073,.T.);
#12545=ADVANCED_FACE('',(#1533),#12140,.F.);
#12546=ADVANCED_FACE('',(#1534),#1074,.T.);
#12547=ADVANCED_FACE('',(#1535),#1005,.T.);
#12548=ADVANCED_FACE('',(#1536),#12141,.T.);
#12549=ADVANCED_FACE('',(#1537),#1006,.T.);
#12550=ADVANCED_FACE('',(#1538),#12142,.T.);
#12551=ADVANCED_FACE('',(#1539),#115,.F.);
#12552=ADVANCED_FACE('',(#1540),#116,.T.);
#12553=ADVANCED_FACE('',(#1541),#117,.T.);
#12554=ADVANCED_FACE('',(#1542),#99,.F.);
#12555=ADVANCED_FACE('',(#1543),#12143,.F.);
#12556=ADVANCED_FACE('',(#1544),#100,.F.);
#12557=ADVANCED_FACE('',(#1545),#12144,.T.);
#12558=ADVANCED_FACE('',(#1546),#12145,.T.);
#12559=ADVANCED_FACE('',(#1547,#283),#1075,.F.);
#12560=ADVANCED_FACE('',(#1548,#284),#1076,.F.);
#12561=ADVANCED_FACE('',(#1549),#43,.T.);
#12562=ADVANCED_FACE('',(#1550),#44,.T.);
#12563=ADVANCED_FACE('',(#1551),#45,.T.);
#12564=ADVANCED_FACE('',(#1552),#46,.T.);
#12565=ADVANCED_FACE('',(#1553),#47,.T.);
#12566=ADVANCED_FACE('',(#1554),#48,.T.);
#12567=ADVANCED_FACE('',(#1555),#49,.T.);
#12568=ADVANCED_FACE('',(#1556),#118,.T.);
#12569=ADVANCED_FACE('',(#1557),#119,.T.);
#12570=ADVANCED_FACE('',(#1558),#120,.T.);
#12571=ADVANCED_FACE('',(#1559),#121,.T.);
#12572=ADVANCED_FACE('',(#1560),#12146,.F.);
#12573=ADVANCED_FACE('',(#1561),#12147,.F.);
#12574=ADVANCED_FACE('',(#1562),#12148,.F.);
#12575=ADVANCED_FACE('',(#1563),#122,.F.);
#12576=ADVANCED_FACE('',(#1564),#12149,.F.);
#12577=ADVANCED_FACE('',(#1565),#12150,.F.);
#12578=ADVANCED_FACE('',(#1566),#12151,.F.);
#12579=ADVANCED_FACE('',(#1567),#101,.T.);
#12580=ADVANCED_FACE('',(#1568),#102,.T.);
#12581=ADVANCED_FACE('',(#1569),#12152,.T.);
#12582=ADVANCED_FACE('',(#1570,#285),#1077,.F.);
#12583=ADVANCED_FACE('',(#1571,#286),#1078,.F.);
#12584=ADVANCED_FACE('',(#1572,#287),#1079,.T.);
#12585=ADVANCED_FACE('',(#1573,#288),#1080,.T.);
#12586=ADVANCED_FACE('',(#1574,#289),#1081,.T.);
#12587=ADVANCED_FACE('',(#1575,#290),#1082,.T.);
#12588=ADVANCED_FACE('',(#1576,#291,#292),#123,.T.);
#12589=ADVANCED_FACE('',(#1577,#293,#294),#50,.F.);
#12590=ADVANCED_FACE('',(#1578,#295,#296),#124,.T.);
#12591=ADVANCED_FACE('',(#1579,#297,#298),#51,.F.);
#12592=ADVANCED_FACE('',(#1580,#299,#300),#125,.T.);
#12593=ADVANCED_FACE('',(#1581,#301,#302),#52,.F.);
#12594=ADVANCED_FACE('',(#1582,#303,#304),#126,.T.);
#12595=ADVANCED_FACE('',(#1583,#305,#306),#53,.F.);
#12596=ADVANCED_FACE('',(#1584,#307,#308),#127,.T.);
#12597=ADVANCED_FACE('',(#1585,#309,#310),#54,.F.);
#12598=ADVANCED_FACE('',(#1586,#311,#312),#128,.T.);
#12599=ADVANCED_FACE('',(#1587,#313,#314),#55,.F.);
#12600=ADVANCED_FACE('',(#1588,#315,#316),#56,.F.);
#12601=ADVANCED_FACE('',(#1589,#317,#318),#129,.T.);
#12602=ADVANCED_FACE('',(#1590),#12153,.F.);
#12603=ADVANCED_FACE('',(#1591),#12154,.T.);
#12604=ADVANCED_FACE('',(#1592),#1083,.T.);
#12605=ADVANCED_FACE('',(#1593),#1084,.F.);
#12606=ADVANCED_FACE('',(#1594,#319),#1085,.T.);
#12607=ADVANCED_FACE('',(#1595,#320),#1086,.T.);
#12608=ADVANCED_FACE('',(#1596),#1087,.T.);
#12609=ADVANCED_FACE('',(#1597),#1088,.F.);
#12610=ADVANCED_FACE('',(#1598),#12155,.T.);
#12611=ADVANCED_FACE('',(#1599),#12156,.F.);
#12612=ADVANCED_FACE('',(#1600,#321),#1089,.T.);
#12613=ADVANCED_FACE('',(#1601,#322),#1090,.T.);
#12614=ADVANCED_FACE('',(#1602),#1091,.F.);
#12615=ADVANCED_FACE('',(#1603),#1092,.T.);
#12616=ADVANCED_FACE('',(#1604),#12157,.T.);
#12617=ADVANCED_FACE('',(#1605),#12158,.F.);
#12618=ADVANCED_FACE('',(#1606),#12159,.F.);
#12619=ADVANCED_FACE('',(#1607),#12160,.T.);
#12620=ADVANCED_FACE('',(#1608),#1093,.F.);
#12621=ADVANCED_FACE('',(#1609),#1094,.T.);
#12622=ADVANCED_FACE('',(#1610,#323),#1095,.T.);
#12623=ADVANCED_FACE('',(#1611,#324),#1096,.T.);
#12624=ADVANCED_FACE('',(#1612),#1097,.F.);
#12625=ADVANCED_FACE('',(#1613),#1098,.T.);
#12626=ADVANCED_FACE('',(#1614),#12161,.T.);
#12627=ADVANCED_FACE('',(#1615),#12162,.F.);
#12628=ADVANCED_FACE('',(#1616),#12163,.F.);
#12629=ADVANCED_FACE('',(#1617),#12164,.T.);
#12630=ADVANCED_FACE('',(#1618),#1099,.F.);
#12631=ADVANCED_FACE('',(#1619),#1100,.T.);
#12632=ADVANCED_FACE('',(#1620,#325),#1101,.T.);
#12633=ADVANCED_FACE('',(#1621,#326),#1102,.T.);
#12634=ADVANCED_FACE('',(#1622),#1103,.F.);
#12635=ADVANCED_FACE('',(#1623),#1104,.T.);
#12636=ADVANCED_FACE('',(#1624),#12165,.T.);
#12637=ADVANCED_FACE('',(#1625),#12166,.F.);
#12638=ADVANCED_FACE('',(#1626),#12167,.F.);
#12639=ADVANCED_FACE('',(#1627),#12168,.T.);
#12640=ADVANCED_FACE('',(#1628),#1105,.F.);
#12641=ADVANCED_FACE('',(#1629),#1106,.T.);
#12642=ADVANCED_FACE('',(#1630,#327),#1107,.T.);
#12643=ADVANCED_FACE('',(#1631,#328),#1108,.T.);
#12644=ADVANCED_FACE('',(#1632),#1109,.F.);
#12645=ADVANCED_FACE('',(#1633),#1110,.T.);
#12646=ADVANCED_FACE('',(#1634),#12169,.T.);
#12647=ADVANCED_FACE('',(#1635),#12170,.F.);
#12648=ADVANCED_FACE('',(#1636),#12171,.F.);
#12649=ADVANCED_FACE('',(#1637),#12172,.T.);
#12650=ADVANCED_FACE('',(#1638),#1111,.F.);
#12651=ADVANCED_FACE('',(#1639),#1112,.T.);
#12652=ADVANCED_FACE('',(#1640,#329),#1113,.T.);
#12653=ADVANCED_FACE('',(#1641,#330),#1114,.T.);
#12654=ADVANCED_FACE('',(#1642),#1115,.F.);
#12655=ADVANCED_FACE('',(#1643),#1116,.T.);
#12656=ADVANCED_FACE('',(#1644),#12173,.T.);
#12657=ADVANCED_FACE('',(#1645),#12174,.F.);
#12658=ADVANCED_FACE('',(#1646),#12175,.F.);
#12659=ADVANCED_FACE('',(#1647),#12176,.T.);
#12660=ADVANCED_FACE('',(#1648),#1117,.F.);
#12661=ADVANCED_FACE('',(#1649),#1118,.T.);
#12662=ADVANCED_FACE('',(#1650,#331),#1119,.T.);
#12663=ADVANCED_FACE('',(#1651,#332),#1120,.T.);
#12664=ADVANCED_FACE('',(#1652),#1121,.F.);
#12665=ADVANCED_FACE('',(#1653),#1122,.T.);
#12666=ADVANCED_FACE('',(#1654),#12177,.T.);
#12667=ADVANCED_FACE('',(#1655),#12178,.F.);
#12668=ADVANCED_FACE('',(#1656),#1123,.T.);
#12669=ADVANCED_FACE('',(#1657),#1124,.F.);
#12670=ADVANCED_FACE('',(#1658),#12179,.T.);
#12671=ADVANCED_FACE('',(#1659),#12180,.F.);
#12672=ADVANCED_FACE('',(#1660),#130,.F.);
#12673=ADVANCED_FACE('',(#1661),#131,.T.);
#12674=ADVANCED_FACE('',(#1662),#132,.T.);
#12675=ADVANCED_FACE('',(#1663),#103,.F.);
#12676=ADVANCED_FACE('',(#1664),#12181,.F.);
#12677=ADVANCED_FACE('',(#1665),#104,.F.);
#12678=ADVANCED_FACE('',(#1666),#12182,.T.);
#12679=ADVANCED_FACE('',(#1667),#12183,.T.);
#12680=ADVANCED_FACE('',(#1668,#333),#1125,.F.);
#12681=ADVANCED_FACE('',(#1669,#334),#1126,.F.);
#12682=ADVANCED_FACE('',(#1670),#57,.T.);
#12683=ADVANCED_FACE('',(#1671),#58,.T.);
#12684=ADVANCED_FACE('',(#1672),#59,.T.);
#12685=ADVANCED_FACE('',(#1673),#60,.T.);
#12686=ADVANCED_FACE('',(#1674),#61,.T.);
#12687=ADVANCED_FACE('',(#1675),#62,.T.);
#12688=ADVANCED_FACE('',(#1676),#63,.T.);
#12689=ADVANCED_FACE('',(#1677),#133,.T.);
#12690=ADVANCED_FACE('',(#1678),#134,.T.);
#12691=ADVANCED_FACE('',(#1679),#135,.T.);
#12692=ADVANCED_FACE('',(#1680),#136,.T.);
#12693=ADVANCED_FACE('',(#1681),#12184,.F.);
#12694=ADVANCED_FACE('',(#1682),#12185,.F.);
#12695=ADVANCED_FACE('',(#1683),#12186,.F.);
#12696=ADVANCED_FACE('',(#1684),#137,.F.);
#12697=ADVANCED_FACE('',(#1685),#12187,.F.);
#12698=ADVANCED_FACE('',(#1686),#12188,.F.);
#12699=ADVANCED_FACE('',(#1687),#12189,.F.);
#12700=ADVANCED_FACE('',(#1688),#105,.T.);
#12701=ADVANCED_FACE('',(#1689),#106,.T.);
#12702=ADVANCED_FACE('',(#1690),#12190,.T.);
#12703=ADVANCED_FACE('',(#1691,#335),#1127,.F.);
#12704=ADVANCED_FACE('',(#1692,#336),#1128,.F.);
#12705=ADVANCED_FACE('',(#1693,#337),#1129,.T.);
#12706=ADVANCED_FACE('',(#1694,#338),#1130,.T.);
#12707=ADVANCED_FACE('',(#1695,#339),#1131,.T.);
#12708=ADVANCED_FACE('',(#1696,#340),#1132,.T.);
#12709=ADVANCED_FACE('',(#1697,#341,#342),#138,.T.);
#12710=ADVANCED_FACE('',(#1698,#343,#344),#64,.F.);
#12711=ADVANCED_FACE('',(#1699,#345,#346),#139,.T.);
#12712=ADVANCED_FACE('',(#1700,#347,#348),#65,.F.);
#12713=ADVANCED_FACE('',(#1701,#349,#350),#140,.T.);
#12714=ADVANCED_FACE('',(#1702,#351,#352),#66,.F.);
#12715=ADVANCED_FACE('',(#1703,#353,#354),#141,.T.);
#12716=ADVANCED_FACE('',(#1704,#355,#356),#67,.F.);
#12717=ADVANCED_FACE('',(#1705,#357,#358),#142,.T.);
#12718=ADVANCED_FACE('',(#1706,#359,#360),#68,.F.);
#12719=ADVANCED_FACE('',(#1707,#361,#362),#143,.T.);
#12720=ADVANCED_FACE('',(#1708,#363,#364),#69,.F.);
#12721=ADVANCED_FACE('',(#1709,#365,#366),#70,.F.);
#12722=ADVANCED_FACE('',(#1710,#367,#368),#144,.T.);
#12723=ADVANCED_FACE('',(#1711),#12191,.F.);
#12724=ADVANCED_FACE('',(#1712),#12192,.T.);
#12725=ADVANCED_FACE('',(#1713),#1133,.T.);
#12726=ADVANCED_FACE('',(#1714),#1134,.F.);
#12727=ADVANCED_FACE('',(#1715,#369),#1135,.T.);
#12728=ADVANCED_FACE('',(#1716,#370),#1136,.T.);
#12729=ADVANCED_FACE('',(#1717),#1137,.T.);
#12730=ADVANCED_FACE('',(#1718),#1138,.F.);
#12731=ADVANCED_FACE('',(#1719),#12193,.T.);
#12732=ADVANCED_FACE('',(#1720),#12194,.F.);
#12733=ADVANCED_FACE('',(#1721,#371),#1139,.T.);
#12734=ADVANCED_FACE('',(#1722,#372),#1140,.T.);
#12735=ADVANCED_FACE('',(#1723),#1141,.F.);
#12736=ADVANCED_FACE('',(#1724),#1142,.T.);
#12737=ADVANCED_FACE('',(#1725),#12195,.T.);
#12738=ADVANCED_FACE('',(#1726),#12196,.F.);
#12739=ADVANCED_FACE('',(#1727),#12197,.F.);
#12740=ADVANCED_FACE('',(#1728),#12198,.T.);
#12741=ADVANCED_FACE('',(#1729),#1143,.F.);
#12742=ADVANCED_FACE('',(#1730),#1144,.T.);
#12743=ADVANCED_FACE('',(#1731,#373),#1145,.T.);
#12744=ADVANCED_FACE('',(#1732,#374),#1146,.T.);
#12745=ADVANCED_FACE('',(#1733),#1147,.F.);
#12746=ADVANCED_FACE('',(#1734),#1148,.T.);
#12747=ADVANCED_FACE('',(#1735),#12199,.T.);
#12748=ADVANCED_FACE('',(#1736),#12200,.F.);
#12749=ADVANCED_FACE('',(#1737),#12201,.F.);
#12750=ADVANCED_FACE('',(#1738),#12202,.T.);
#12751=ADVANCED_FACE('',(#1739),#1149,.F.);
#12752=ADVANCED_FACE('',(#1740),#1150,.T.);
#12753=ADVANCED_FACE('',(#1741,#375),#1151,.T.);
#12754=ADVANCED_FACE('',(#1742,#376),#1152,.T.);
#12755=ADVANCED_FACE('',(#1743),#1153,.F.);
#12756=ADVANCED_FACE('',(#1744),#1154,.T.);
#12757=ADVANCED_FACE('',(#1745),#12203,.T.);
#12758=ADVANCED_FACE('',(#1746),#12204,.F.);
#12759=ADVANCED_FACE('',(#1747),#12205,.F.);
#12760=ADVANCED_FACE('',(#1748),#12206,.T.);
#12761=ADVANCED_FACE('',(#1749),#1155,.F.);
#12762=ADVANCED_FACE('',(#1750),#1156,.T.);
#12763=ADVANCED_FACE('',(#1751,#377),#1157,.T.);
#12764=ADVANCED_FACE('',(#1752,#378),#1158,.T.);
#12765=ADVANCED_FACE('',(#1753),#1159,.F.);
#12766=ADVANCED_FACE('',(#1754),#1160,.T.);
#12767=ADVANCED_FACE('',(#1755),#12207,.T.);
#12768=ADVANCED_FACE('',(#1756),#12208,.F.);
#12769=ADVANCED_FACE('',(#1757),#12209,.F.);
#12770=ADVANCED_FACE('',(#1758),#12210,.T.);
#12771=ADVANCED_FACE('',(#1759),#1161,.F.);
#12772=ADVANCED_FACE('',(#1760),#1162,.T.);
#12773=ADVANCED_FACE('',(#1761,#379),#1163,.T.);
#12774=ADVANCED_FACE('',(#1762,#380),#1164,.T.);
#12775=ADVANCED_FACE('',(#1763),#1165,.F.);
#12776=ADVANCED_FACE('',(#1764),#1166,.T.);
#12777=ADVANCED_FACE('',(#1765),#12211,.T.);
#12778=ADVANCED_FACE('',(#1766),#12212,.F.);
#12779=ADVANCED_FACE('',(#1767),#12213,.F.);
#12780=ADVANCED_FACE('',(#1768),#12214,.T.);
#12781=ADVANCED_FACE('',(#1769),#1167,.F.);
#12782=ADVANCED_FACE('',(#1770),#1168,.T.);
#12783=ADVANCED_FACE('',(#1771,#381),#1169,.T.);
#12784=ADVANCED_FACE('',(#1772,#382),#1170,.T.);
#12785=ADVANCED_FACE('',(#1773),#1171,.F.);
#12786=ADVANCED_FACE('',(#1774),#1172,.T.);
#12787=ADVANCED_FACE('',(#1775),#12215,.T.);
#12788=ADVANCED_FACE('',(#1776),#12216,.F.);
#12789=ADVANCED_FACE('',(#1777),#1173,.T.);
#12790=ADVANCED_FACE('',(#1778),#1174,.F.);
#12791=ADVANCED_FACE('',(#1779),#12217,.T.);
#12792=ADVANCED_FACE('',(#1780),#12218,.F.);
#12793=ADVANCED_FACE('',(#1781),#145,.F.);
#12794=ADVANCED_FACE('',(#1782),#146,.T.);
#12795=ADVANCED_FACE('',(#1783),#147,.T.);
#12796=ADVANCED_FACE('',(#1784),#107,.F.);
#12797=ADVANCED_FACE('',(#1785),#12219,.F.);
#12798=ADVANCED_FACE('',(#1786),#108,.F.);
#12799=ADVANCED_FACE('',(#1787),#12220,.T.);
#12800=ADVANCED_FACE('',(#1788),#12221,.T.);
#12801=ADVANCED_FACE('',(#1789,#383),#1175,.T.);
#12802=ADVANCED_FACE('',(#1790,#384),#1176,.T.);
#12803=ADVANCED_FACE('',(#1791),#71,.T.);
#12804=ADVANCED_FACE('',(#1792),#72,.T.);
#12805=ADVANCED_FACE('',(#1793),#73,.T.);
#12806=ADVANCED_FACE('',(#1794),#74,.T.);
#12807=ADVANCED_FACE('',(#1795),#75,.T.);
#12808=ADVANCED_FACE('',(#1796),#76,.T.);
#12809=ADVANCED_FACE('',(#1797),#77,.T.);
#12810=ADVANCED_FACE('',(#1798),#148,.T.);
#12811=ADVANCED_FACE('',(#1799),#149,.T.);
#12812=ADVANCED_FACE('',(#1800),#150,.T.);
#12813=ADVANCED_FACE('',(#1801),#151,.T.);
#12814=ADVANCED_FACE('',(#1802),#12222,.F.);
#12815=ADVANCED_FACE('',(#1803),#12223,.F.);
#12816=ADVANCED_FACE('',(#1804),#12224,.F.);
#12817=ADVANCED_FACE('',(#1805),#152,.F.);
#12818=ADVANCED_FACE('',(#1806),#12225,.F.);
#12819=ADVANCED_FACE('',(#1807),#12226,.F.);
#12820=ADVANCED_FACE('',(#1808),#12227,.F.);
#12821=ADVANCED_FACE('',(#1809),#109,.T.);
#12822=ADVANCED_FACE('',(#1810),#110,.T.);
#12823=ADVANCED_FACE('',(#1811),#12228,.T.);
#12824=ADVANCED_FACE('',(#1812,#385),#1177,.T.);
#12825=ADVANCED_FACE('',(#1813,#386),#1178,.T.);
#12826=ADVANCED_FACE('',(#1814,#387),#1179,.F.);
#12827=ADVANCED_FACE('',(#1815,#388),#1180,.F.);
#12828=ADVANCED_FACE('',(#1816,#389),#1181,.F.);
#12829=ADVANCED_FACE('',(#1817,#390),#1182,.F.);
#12830=ADVANCED_FACE('',(#1818,#391,#392),#153,.T.);
#12831=ADVANCED_FACE('',(#1819,#393,#394),#78,.F.);
#12832=ADVANCED_FACE('',(#1820,#395,#396),#154,.T.);
#12833=ADVANCED_FACE('',(#1821,#397,#398),#79,.F.);
#12834=ADVANCED_FACE('',(#1822,#399,#400),#155,.T.);
#12835=ADVANCED_FACE('',(#1823,#401,#402),#80,.F.);
#12836=ADVANCED_FACE('',(#1824,#403,#404),#156,.T.);
#12837=ADVANCED_FACE('',(#1825,#405,#406),#81,.F.);
#12838=ADVANCED_FACE('',(#1826,#407,#408),#157,.T.);
#12839=ADVANCED_FACE('',(#1827,#409,#410),#82,.F.);
#12840=ADVANCED_FACE('',(#1828,#411,#412),#158,.T.);
#12841=ADVANCED_FACE('',(#1829,#413,#414),#83,.F.);
#12842=ADVANCED_FACE('',(#1830,#415,#416),#84,.F.);
#12843=ADVANCED_FACE('',(#1831,#417,#418),#159,.T.);
#12844=ADVANCED_FACE('',(#1832),#12229,.F.);
#12845=ADVANCED_FACE('',(#1833),#12230,.T.);
#12846=ADVANCED_FACE('',(#1834),#1183,.F.);
#12847=ADVANCED_FACE('',(#1835),#1184,.T.);
#12848=ADVANCED_FACE('',(#1836,#419),#1185,.F.);
#12849=ADVANCED_FACE('',(#1837,#420),#1186,.F.);
#12850=ADVANCED_FACE('',(#1838),#1187,.F.);
#12851=ADVANCED_FACE('',(#1839),#1188,.T.);
#12852=ADVANCED_FACE('',(#1840),#12231,.T.);
#12853=ADVANCED_FACE('',(#1841),#12232,.F.);
#12854=ADVANCED_FACE('',(#1842,#421),#1189,.F.);
#12855=ADVANCED_FACE('',(#1843,#422),#1190,.F.);
#12856=ADVANCED_FACE('',(#1844),#1191,.T.);
#12857=ADVANCED_FACE('',(#1845),#1192,.F.);
#12858=ADVANCED_FACE('',(#1846),#12233,.T.);
#12859=ADVANCED_FACE('',(#1847),#12234,.F.);
#12860=ADVANCED_FACE('',(#1848),#12235,.F.);
#12861=ADVANCED_FACE('',(#1849),#12236,.T.);
#12862=ADVANCED_FACE('',(#1850),#1193,.T.);
#12863=ADVANCED_FACE('',(#1851),#1194,.F.);
#12864=ADVANCED_FACE('',(#1852,#423),#1195,.F.);
#12865=ADVANCED_FACE('',(#1853,#424),#1196,.F.);
#12866=ADVANCED_FACE('',(#1854),#1197,.T.);
#12867=ADVANCED_FACE('',(#1855),#1198,.F.);
#12868=ADVANCED_FACE('',(#1856),#12237,.T.);
#12869=ADVANCED_FACE('',(#1857),#12238,.F.);
#12870=ADVANCED_FACE('',(#1858),#12239,.F.);
#12871=ADVANCED_FACE('',(#1859),#12240,.T.);
#12872=ADVANCED_FACE('',(#1860),#1199,.T.);
#12873=ADVANCED_FACE('',(#1861),#1200,.F.);
#12874=ADVANCED_FACE('',(#1862,#425),#1201,.F.);
#12875=ADVANCED_FACE('',(#1863,#426),#1202,.F.);
#12876=ADVANCED_FACE('',(#1864),#1203,.T.);
#12877=ADVANCED_FACE('',(#1865),#1204,.F.);
#12878=ADVANCED_FACE('',(#1866),#12241,.T.);
#12879=ADVANCED_FACE('',(#1867),#12242,.F.);
#12880=ADVANCED_FACE('',(#1868),#12243,.F.);
#12881=ADVANCED_FACE('',(#1869),#12244,.T.);
#12882=ADVANCED_FACE('',(#1870),#1205,.T.);
#12883=ADVANCED_FACE('',(#1871),#1206,.F.);
#12884=ADVANCED_FACE('',(#1872,#427),#1207,.F.);
#12885=ADVANCED_FACE('',(#1873,#428),#1208,.F.);
#12886=ADVANCED_FACE('',(#1874),#1209,.T.);
#12887=ADVANCED_FACE('',(#1875),#1210,.F.);
#12888=ADVANCED_FACE('',(#1876),#12245,.T.);
#12889=ADVANCED_FACE('',(#1877),#12246,.F.);
#12890=ADVANCED_FACE('',(#1878),#12247,.F.);
#12891=ADVANCED_FACE('',(#1879),#12248,.T.);
#12892=ADVANCED_FACE('',(#1880),#1211,.T.);
#12893=ADVANCED_FACE('',(#1881),#1212,.F.);
#12894=ADVANCED_FACE('',(#1882,#429),#1213,.F.);
#12895=ADVANCED_FACE('',(#1883,#430),#1214,.F.);
#12896=ADVANCED_FACE('',(#1884),#1215,.T.);
#12897=ADVANCED_FACE('',(#1885),#1216,.F.);
#12898=ADVANCED_FACE('',(#1886),#12249,.T.);
#12899=ADVANCED_FACE('',(#1887),#12250,.F.);
#12900=ADVANCED_FACE('',(#1888),#12251,.F.);
#12901=ADVANCED_FACE('',(#1889),#12252,.T.);
#12902=ADVANCED_FACE('',(#1890),#1217,.T.);
#12903=ADVANCED_FACE('',(#1891),#1218,.F.);
#12904=ADVANCED_FACE('',(#1892,#431),#1219,.F.);
#12905=ADVANCED_FACE('',(#1893,#432),#1220,.F.);
#12906=ADVANCED_FACE('',(#1894),#1221,.T.);
#12907=ADVANCED_FACE('',(#1895),#1222,.F.);
#12908=ADVANCED_FACE('',(#1896),#12253,.T.);
#12909=ADVANCED_FACE('',(#1897),#12254,.F.);
#12910=ADVANCED_FACE('',(#1898),#1223,.F.);
#12911=ADVANCED_FACE('',(#1899),#1224,.T.);
#12912=ADVANCED_FACE('',(#1900),#12255,.T.);
#12913=ADVANCED_FACE('',(#1901),#12256,.F.);
#12914=ADVANCED_FACE('',(#1902),#160,.F.);
#12915=ADVANCED_FACE('',(#1903),#161,.T.);
#12916=ADVANCED_FACE('',(#1904),#162,.T.);
#12917=ADVANCED_FACE('',(#1905),#111,.F.);
#12918=ADVANCED_FACE('',(#1906),#12257,.F.);
#12919=ADVANCED_FACE('',(#1907),#112,.F.);
#12920=ADVANCED_FACE('',(#1908),#12258,.T.);
#12921=ADVANCED_FACE('',(#1909),#12259,.T.);
#12922=ADVANCED_FACE('',(#1910,#433),#1225,.T.);
#12923=ADVANCED_FACE('',(#1911,#434),#1226,.T.);
#12924=ADVANCED_FACE('',(#1912),#85,.T.);
#12925=ADVANCED_FACE('',(#1913),#86,.T.);
#12926=ADVANCED_FACE('',(#1914),#87,.T.);
#12927=ADVANCED_FACE('',(#1915),#88,.T.);
#12928=ADVANCED_FACE('',(#1916),#89,.T.);
#12929=ADVANCED_FACE('',(#1917),#90,.T.);
#12930=ADVANCED_FACE('',(#1918),#91,.T.);
#12931=ADVANCED_FACE('',(#1919),#163,.T.);
#12932=ADVANCED_FACE('',(#1920),#164,.T.);
#12933=ADVANCED_FACE('',(#1921),#165,.T.);
#12934=ADVANCED_FACE('',(#1922),#166,.T.);
#12935=ADVANCED_FACE('',(#1923),#12260,.F.);
#12936=ADVANCED_FACE('',(#1924),#12261,.F.);
#12937=ADVANCED_FACE('',(#1925),#12262,.F.);
#12938=ADVANCED_FACE('',(#1926),#167,.F.);
#12939=ADVANCED_FACE('',(#1927),#12263,.F.);
#12940=ADVANCED_FACE('',(#1928),#12264,.F.);
#12941=ADVANCED_FACE('',(#1929),#12265,.F.);
#12942=ADVANCED_FACE('',(#1930),#113,.T.);
#12943=ADVANCED_FACE('',(#1931),#114,.T.);
#12944=ADVANCED_FACE('',(#1932),#12266,.T.);
#12945=ADVANCED_FACE('',(#1933,#435),#1227,.T.);
#12946=ADVANCED_FACE('',(#1934,#436),#1228,.T.);
#12947=ADVANCED_FACE('',(#1935,#437),#1229,.F.);
#12948=ADVANCED_FACE('',(#1936,#438),#1230,.F.);
#12949=ADVANCED_FACE('',(#1937,#439),#1231,.F.);
#12950=ADVANCED_FACE('',(#1938,#440),#1232,.F.);
#12951=ADVANCED_FACE('',(#1939,#441,#442),#168,.T.);
#12952=ADVANCED_FACE('',(#1940,#443,#444),#92,.F.);
#12953=ADVANCED_FACE('',(#1941,#445,#446),#169,.T.);
#12954=ADVANCED_FACE('',(#1942,#447,#448),#93,.F.);
#12955=ADVANCED_FACE('',(#1943,#449,#450),#170,.T.);
#12956=ADVANCED_FACE('',(#1944,#451,#452),#94,.F.);
#12957=ADVANCED_FACE('',(#1945,#453,#454),#171,.T.);
#12958=ADVANCED_FACE('',(#1946,#455,#456),#95,.F.);
#12959=ADVANCED_FACE('',(#1947,#457,#458),#172,.T.);
#12960=ADVANCED_FACE('',(#1948,#459,#460),#96,.F.);
#12961=ADVANCED_FACE('',(#1949,#461,#462),#173,.T.);
#12962=ADVANCED_FACE('',(#1950,#463,#464),#97,.F.);
#12963=ADVANCED_FACE('',(#1951,#465,#466),#98,.F.);
#12964=ADVANCED_FACE('',(#1952,#467,#468),#174,.T.);
#12965=ADVANCED_FACE('',(#1953),#12267,.F.);
#12966=ADVANCED_FACE('',(#1954),#12268,.T.);
#12967=ADVANCED_FACE('',(#1955),#1233,.F.);
#12968=ADVANCED_FACE('',(#1956),#1234,.T.);
#12969=ADVANCED_FACE('',(#1957,#469),#1235,.F.);
#12970=ADVANCED_FACE('',(#1958,#470),#1236,.F.);
#12971=ADVANCED_FACE('',(#1959),#1237,.F.);
#12972=ADVANCED_FACE('',(#1960),#1238,.T.);
#12973=ADVANCED_FACE('',(#1961),#12269,.T.);
#12974=ADVANCED_FACE('',(#1962),#12270,.F.);
#12975=ADVANCED_FACE('',(#1963,#471),#1239,.F.);
#12976=ADVANCED_FACE('',(#1964,#472),#1240,.F.);
#12977=ADVANCED_FACE('',(#1965),#1241,.T.);
#12978=ADVANCED_FACE('',(#1966),#1242,.F.);
#12979=ADVANCED_FACE('',(#1967),#12271,.T.);
#12980=ADVANCED_FACE('',(#1968),#12272,.F.);
#12981=ADVANCED_FACE('',(#1969),#12273,.F.);
#12982=ADVANCED_FACE('',(#1970),#12274,.T.);
#12983=ADVANCED_FACE('',(#1971),#1243,.T.);
#12984=ADVANCED_FACE('',(#1972),#1244,.F.);
#12985=ADVANCED_FACE('',(#1973,#473),#1245,.F.);
#12986=ADVANCED_FACE('',(#1974,#474),#1246,.F.);
#12987=ADVANCED_FACE('',(#1975),#1247,.T.);
#12988=ADVANCED_FACE('',(#1976),#1248,.F.);
#12989=ADVANCED_FACE('',(#1977),#12275,.T.);
#12990=ADVANCED_FACE('',(#1978),#12276,.F.);
#12991=ADVANCED_FACE('',(#1979),#12277,.F.);
#12992=ADVANCED_FACE('',(#1980),#12278,.T.);
#12993=ADVANCED_FACE('',(#1981),#1249,.T.);
#12994=ADVANCED_FACE('',(#1982),#1250,.F.);
#12995=ADVANCED_FACE('',(#1983,#475),#1251,.F.);
#12996=ADVANCED_FACE('',(#1984,#476),#1252,.F.);
#12997=ADVANCED_FACE('',(#1985),#1253,.T.);
#12998=ADVANCED_FACE('',(#1986),#1254,.F.);
#12999=ADVANCED_FACE('',(#1987),#12279,.T.);
#13000=ADVANCED_FACE('',(#1988),#12280,.F.);
#13001=ADVANCED_FACE('',(#1989),#12281,.F.);
#13002=ADVANCED_FACE('',(#1990),#12282,.T.);
#13003=ADVANCED_FACE('',(#1991),#1255,.T.);
#13004=ADVANCED_FACE('',(#1992),#1256,.F.);
#13005=ADVANCED_FACE('',(#1993,#477),#1257,.F.);
#13006=ADVANCED_FACE('',(#1994,#478),#1258,.F.);
#13007=ADVANCED_FACE('',(#1995),#1259,.T.);
#13008=ADVANCED_FACE('',(#1996),#1260,.F.);
#13009=ADVANCED_FACE('',(#1997),#12283,.T.);
#13010=ADVANCED_FACE('',(#1998),#12284,.F.);
#13011=ADVANCED_FACE('',(#1999),#12285,.F.);
#13012=ADVANCED_FACE('',(#2000),#12286,.T.);
#13013=ADVANCED_FACE('',(#2001),#1261,.T.);
#13014=ADVANCED_FACE('',(#2002),#1262,.F.);
#13015=ADVANCED_FACE('',(#2003,#479),#1263,.F.);
#13016=ADVANCED_FACE('',(#2004,#480),#1264,.F.);
#13017=ADVANCED_FACE('',(#2005),#1265,.T.);
#13018=ADVANCED_FACE('',(#2006),#1266,.F.);
#13019=ADVANCED_FACE('',(#2007),#12287,.T.);
#13020=ADVANCED_FACE('',(#2008),#12288,.F.);
#13021=ADVANCED_FACE('',(#2009),#12289,.F.);
#13022=ADVANCED_FACE('',(#2010),#12290,.T.);
#13023=ADVANCED_FACE('',(#2011),#1267,.T.);
#13024=ADVANCED_FACE('',(#2012),#1268,.F.);
#13025=ADVANCED_FACE('',(#2013,#481),#1269,.F.);
#13026=ADVANCED_FACE('',(#2014,#482),#1270,.F.);
#13027=ADVANCED_FACE('',(#2015),#1271,.T.);
#13028=ADVANCED_FACE('',(#2016),#1272,.F.);
#13029=ADVANCED_FACE('',(#2017),#12291,.T.);
#13030=ADVANCED_FACE('',(#2018),#12292,.F.);
#13031=ADVANCED_FACE('',(#2019),#1273,.F.);
#13032=ADVANCED_FACE('',(#2020),#1274,.T.);
#13033=ADVANCED_FACE('',(#2021),#12293,.T.);
#13034=ADVANCED_FACE('',(#2022),#12294,.F.);
#13035=ADVANCED_FACE('',(#2023),#12295,.F.);
#13036=ADVANCED_FACE('',(#2024,#483,#484),#1275,.F.);
#13037=ADVANCED_FACE('',(#2025),#12296,.F.);
#13038=ADVANCED_FACE('',(#2026,#485,#486),#1276,.T.);
#13039=ADVANCED_FACE('',(#2027),#1277,.F.);
#13040=ADVANCED_FACE('',(#2028),#1278,.F.);
#13041=ADVANCED_FACE('',(#2029),#1279,.F.);
#13042=ADVANCED_FACE('',(#2030),#1280,.F.);
#13043=ADVANCED_FACE('',(#2031),#12297,.F.);
#13044=ADVANCED_FACE('',(#2032),#12298,.F.);
#13045=ADVANCED_FACE('',(#2033,#487,#488),#1281,.F.);
#13046=ADVANCED_FACE('',(#2034),#1282,.T.);
#13047=ADVANCED_FACE('',(#2035),#1283,.T.);
#13048=ADVANCED_FACE('',(#2036),#1284,.T.);
#13049=ADVANCED_FACE('',(#2037),#1285,.T.);
#13050=ADVANCED_FACE('',(#2038,#489,#490),#1286,.T.);
#13051=CLOSED_SHELL('',(#12299,#12300,#12301,#12302,#12303,#12304,#12305,
#12306,#12307,#12308,#12309,#12310,#12311,#12312,#12313,#12314,#12315,#12316,
#12317,#12318,#12319,#12320,#12321,#12322,#12323,#12324,#12325,#12326,#12327,
#12328,#12329,#12330,#12331,#12332,#12333,#12334,#12335,#12336,#12337,#12338,
#12339,#12340,#12341,#12342,#12343,#12344,#12345,#12346,#12347,#12348,#12349,
#12350,#12351,#12352,#12353,#12354,#12355,#12356,#12357,#12358,#12359,#12360,
#12361,#12362,#12363,#12364,#12365,#12366,#12367,#12368,#12369,#12370,#12371,
#12372,#12373,#12374,#12375,#12376,#12377,#12378,#12379,#12380,#12381,#12382,
#12383,#12384,#12385,#12386,#12387,#12388,#12389,#12390,#12391,#12392,#12393,
#12394,#12395,#12396,#12397,#12398,#12399,#12400,#12401,#12402,#12403,#12404,
#12405,#12406,#12407,#12408,#12409,#12410,#12411,#12412,#12413,#12414,#12415,
#12416,#12417,#12418,#12419,#12420,#12421,#12422,#12423,#12424,#12425,#12426,
#12427,#12428,#12429,#12430,#12431,#12432,#12433,#12434,#12435,#12436,#12437,
#12438,#12439,#12440,#12441,#12442,#12443,#12444,#12445,#12446,#12447,#12448,
#12449,#12450,#12451,#12452,#12453,#12454,#12455,#12456,#12457,#12458,#12459,
#12460,#12461,#12462,#12463,#12464));
#13052=CLOSED_SHELL('',(#12465,#12466,#12467,#12468,#12469,#12470,#12471,
#12472,#12473,#12474,#12475,#12476,#12477,#12478,#12479,#12480,#12481,#12482,
#12483,#12484,#12485,#12486,#12487,#12488,#12489,#12490,#12491,#12492,#12493,
#12494,#12495,#12496,#12497,#12498,#12499,#12500,#12501,#12502,#12503,#12504,
#12505,#12506,#12507,#12508,#12509,#12510,#12511,#12512,#12513,#12514,#12515,
#12516,#12517,#12518,#12519,#12520,#12521,#12522,#12523,#12524,#12525,#12526,
#12527,#12528,#12529,#12530,#12531,#12532,#12533,#12534,#12535,#12536,#12537,
#12538,#12539,#12540,#12541,#12542,#12543,#12544,#12545,#12546,#12547,#12548,
#12549,#12550));
#13053=CLOSED_SHELL('',(#12551,#12552,#12553,#12554,#12555,#12556,#12557,
#12558,#12559,#12560));
#13054=CLOSED_SHELL('',(#12561));
#13055=CLOSED_SHELL('',(#12562));
#13056=CLOSED_SHELL('',(#12563));
#13057=CLOSED_SHELL('',(#12564));
#13058=CLOSED_SHELL('',(#12565));
#13059=CLOSED_SHELL('',(#12566));
#13060=CLOSED_SHELL('',(#12567));
#13061=CLOSED_SHELL('',(#12568,#12569,#12570,#12571,#12572,#12573,#12574,
#12575,#12576,#12577,#12578,#12579,#12580,#12581,#12582,#12583,#12584,#12585,
#12586,#12587));
#13062=CLOSED_SHELL('',(#12588,#12589,#12590,#12591,#12592,#12593,#12594,
#12595,#12596,#12597,#12598,#12599,#12600,#12601,#12602,#12603,#12604,#12605,
#12606,#12607,#12608,#12609,#12610,#12611,#12612,#12613,#12614,#12615,#12616,
#12617,#12618,#12619,#12620,#12621,#12622,#12623,#12624,#12625,#12626,#12627,
#12628,#12629,#12630,#12631,#12632,#12633,#12634,#12635,#12636,#12637,#12638,
#12639,#12640,#12641,#12642,#12643,#12644,#12645,#12646,#12647,#12648,#12649,
#12650,#12651,#12652,#12653,#12654,#12655,#12656,#12657,#12658,#12659,#12660,
#12661,#12662,#12663,#12664,#12665,#12666,#12667,#12668,#12669,#12670,#12671));
#13063=CLOSED_SHELL('',(#12672,#12673,#12674,#12675,#12676,#12677,#12678,
#12679,#12680,#12681));
#13064=CLOSED_SHELL('',(#12682));
#13065=CLOSED_SHELL('',(#12683));
#13066=CLOSED_SHELL('',(#12684));
#13067=CLOSED_SHELL('',(#12685));
#13068=CLOSED_SHELL('',(#12686));
#13069=CLOSED_SHELL('',(#12687));
#13070=CLOSED_SHELL('',(#12688));
#13071=CLOSED_SHELL('',(#12689,#12690,#12691,#12692,#12693,#12694,#12695,
#12696,#12697,#12698,#12699,#12700,#12701,#12702,#12703,#12704,#12705,#12706,
#12707,#12708));
#13072=CLOSED_SHELL('',(#12709,#12710,#12711,#12712,#12713,#12714,#12715,
#12716,#12717,#12718,#12719,#12720,#12721,#12722,#12723,#12724,#12725,#12726,
#12727,#12728,#12729,#12730,#12731,#12732,#12733,#12734,#12735,#12736,#12737,
#12738,#12739,#12740,#12741,#12742,#12743,#12744,#12745,#12746,#12747,#12748,
#12749,#12750,#12751,#12752,#12753,#12754,#12755,#12756,#12757,#12758,#12759,
#12760,#12761,#12762,#12763,#12764,#12765,#12766,#12767,#12768,#12769,#12770,
#12771,#12772,#12773,#12774,#12775,#12776,#12777,#12778,#12779,#12780,#12781,
#12782,#12783,#12784,#12785,#12786,#12787,#12788,#12789,#12790,#12791,#12792));
#13073=CLOSED_SHELL('',(#12793,#12794,#12795,#12796,#12797,#12798,#12799,
#12800,#12801,#12802));
#13074=CLOSED_SHELL('',(#12803));
#13075=CLOSED_SHELL('',(#12804));
#13076=CLOSED_SHELL('',(#12805));
#13077=CLOSED_SHELL('',(#12806));
#13078=CLOSED_SHELL('',(#12807));
#13079=CLOSED_SHELL('',(#12808));
#13080=CLOSED_SHELL('',(#12809));
#13081=CLOSED_SHELL('',(#12810,#12811,#12812,#12813,#12814,#12815,#12816,
#12817,#12818,#12819,#12820,#12821,#12822,#12823,#12824,#12825,#12826,#12827,
#12828,#12829));
#13082=CLOSED_SHELL('',(#12830,#12831,#12832,#12833,#12834,#12835,#12836,
#12837,#12838,#12839,#12840,#12841,#12842,#12843,#12844,#12845,#12846,#12847,
#12848,#12849,#12850,#12851,#12852,#12853,#12854,#12855,#12856,#12857,#12858,
#12859,#12860,#12861,#12862,#12863,#12864,#12865,#12866,#12867,#12868,#12869,
#12870,#12871,#12872,#12873,#12874,#12875,#12876,#12877,#12878,#12879,#12880,
#12881,#12882,#12883,#12884,#12885,#12886,#12887,#12888,#12889,#12890,#12891,
#12892,#12893,#12894,#12895,#12896,#12897,#12898,#12899,#12900,#12901,#12902,
#12903,#12904,#12905,#12906,#12907,#12908,#12909,#12910,#12911,#12912,#12913));
#13083=CLOSED_SHELL('',(#12914,#12915,#12916,#12917,#12918,#12919,#12920,
#12921,#12922,#12923));
#13084=CLOSED_SHELL('',(#12924));
#13085=CLOSED_SHELL('',(#12925));
#13086=CLOSED_SHELL('',(#12926));
#13087=CLOSED_SHELL('',(#12927));
#13088=CLOSED_SHELL('',(#12928));
#13089=CLOSED_SHELL('',(#12929));
#13090=CLOSED_SHELL('',(#12930));
#13091=CLOSED_SHELL('',(#12931,#12932,#12933,#12934,#12935,#12936,#12937,
#12938,#12939,#12940,#12941,#12942,#12943,#12944,#12945,#12946,#12947,#12948,
#12949,#12950));
#13092=CLOSED_SHELL('',(#12951,#12952,#12953,#12954,#12955,#12956,#12957,
#12958,#12959,#12960,#12961,#12962,#12963,#12964,#12965,#12966,#12967,#12968,
#12969,#12970,#12971,#12972,#12973,#12974,#12975,#12976,#12977,#12978,#12979,
#12980,#12981,#12982,#12983,#12984,#12985,#12986,#12987,#12988,#12989,#12990,
#12991,#12992,#12993,#12994,#12995,#12996,#12997,#12998,#12999,#13000,#13001,
#13002,#13003,#13004,#13005,#13006,#13007,#13008,#13009,#13010,#13011,#13012,
#13013,#13014,#13015,#13016,#13017,#13018,#13019,#13020,#13021,#13022,#13023,
#13024,#13025,#13026,#13027,#13028,#13029,#13030,#13031,#13032,#13033,#13034));
#13093=CLOSED_SHELL('',(#13035,#13036,#13037,#13038,#13039,#13040,#13041,
#13042));
#13094=CLOSED_SHELL('',(#13043,#13044,#13045,#13046,#13047,#13048,#13049,
#13050));
#13095=DERIVED_UNIT_ELEMENT(#13111,1.);
#13096=DERIVED_UNIT_ELEMENT(#43783,-3.);
#13097=DERIVED_UNIT_ELEMENT(#13111,1.);
#13098=DERIVED_UNIT_ELEMENT(#43783,-3.);
#13099=DERIVED_UNIT_ELEMENT(#13111,1.);
#13100=DERIVED_UNIT_ELEMENT(#43783,-3.);
#13101=DERIVED_UNIT_ELEMENT(#13111,1.);
#13102=DERIVED_UNIT_ELEMENT(#43783,-3.);
#13103=DERIVED_UNIT_ELEMENT(#13111,1.);
#13104=DERIVED_UNIT_ELEMENT(#43783,-3.);
#13105=DERIVED_UNIT_ELEMENT(#13111,1.);
#13106=DERIVED_UNIT_ELEMENT(#43783,-3.);
#13107=DERIVED_UNIT_ELEMENT(#13111,1.);
#13108=DERIVED_UNIT_ELEMENT(#43783,-3.);
#13109=DERIVED_UNIT_ELEMENT(#13111,1.);
#13110=DERIVED_UNIT_ELEMENT(#43783,-3.);
#13111=(
MASS_UNIT()
NAMED_UNIT(*)
SI_UNIT(.KILO.,.GRAM.)
);
#13112=DERIVED_UNIT((#13095,#13096));
#13113=DERIVED_UNIT((#13097,#13098));
#13114=DERIVED_UNIT((#13099,#13100));
#13115=DERIVED_UNIT((#13101,#13102));
#13116=DERIVED_UNIT((#13103,#13104));
#13117=DERIVED_UNIT((#13105,#13106));
#13118=DERIVED_UNIT((#13107,#13108));
#13119=DERIVED_UNIT((#13109,#13110));
#13120=MEASURE_REPRESENTATION_ITEM('density measure',
POSITIVE_RATIO_MEASURE(7850.),#13112);
#13121=MEASURE_REPRESENTATION_ITEM('density measure',
POSITIVE_RATIO_MEASURE(7850.),#13113);
#13122=MEASURE_REPRESENTATION_ITEM('density measure',
POSITIVE_RATIO_MEASURE(7850.),#13114);
#13123=MEASURE_REPRESENTATION_ITEM('density measure',
POSITIVE_RATIO_MEASURE(7850.),#13115);
#13124=MEASURE_REPRESENTATION_ITEM('density measure',
POSITIVE_RATIO_MEASURE(7850.),#13116);
#13125=MEASURE_REPRESENTATION_ITEM('density measure',
POSITIVE_RATIO_MEASURE(7850.),#13117);
#13126=MEASURE_REPRESENTATION_ITEM('density measure',
POSITIVE_RATIO_MEASURE(7850.),#13118);
#13127=MEASURE_REPRESENTATION_ITEM('density measure',
POSITIVE_RATIO_MEASURE(7850.),#13119);
#13128=PROPERTY_DEFINITION_REPRESENTATION(#13168,#13144);
#13129=PROPERTY_DEFINITION_REPRESENTATION(#13169,#13145);
#13130=PROPERTY_DEFINITION_REPRESENTATION(#13170,#13146);
#13131=PROPERTY_DEFINITION_REPRESENTATION(#13171,#13147);
#13132=PROPERTY_DEFINITION_REPRESENTATION(#13172,#13148);
#13133=PROPERTY_DEFINITION_REPRESENTATION(#13173,#13149);
#13134=PROPERTY_DEFINITION_REPRESENTATION(#13174,#13150);
#13135=PROPERTY_DEFINITION_REPRESENTATION(#13175,#13151);
#13136=PROPERTY_DEFINITION_REPRESENTATION(#13176,#13152);
#13137=PROPERTY_DEFINITION_REPRESENTATION(#13177,#13153);
#13138=PROPERTY_DEFINITION_REPRESENTATION(#13178,#13154);
#13139=PROPERTY_DEFINITION_REPRESENTATION(#13179,#13155);
#13140=PROPERTY_DEFINITION_REPRESENTATION(#13180,#13156);
#13141=PROPERTY_DEFINITION_REPRESENTATION(#13181,#13157);
#13142=PROPERTY_DEFINITION_REPRESENTATION(#13182,#13158);
#13143=PROPERTY_DEFINITION_REPRESENTATION(#13183,#13159);
#13144=REPRESENTATION('material name',(#13160),#43773);
#13145=REPRESENTATION('density',(#13120),#43773);
#13146=REPRESENTATION('material name',(#13161),#43774);
#13147=REPRESENTATION('density',(#13121),#43774);
#13148=REPRESENTATION('material name',(#13162),#43775);
#13149=REPRESENTATION('density',(#13122),#43775);
#13150=REPRESENTATION('material name',(#13163),#43776);
#13151=REPRESENTATION('density',(#13123),#43776);
#13152=REPRESENTATION('material name',(#13164),#43777);
#13153=REPRESENTATION('density',(#13124),#43777);
#13154=REPRESENTATION('material name',(#13165),#43778);
#13155=REPRESENTATION('density',(#13125),#43778);
#13156=REPRESENTATION('material name',(#13166),#43779);
#13157=REPRESENTATION('density',(#13126),#43779);
#13158=REPRESENTATION('material name',(#13167),#43780);
#13159=REPRESENTATION('density',(#13127),#43780);
#13160=DESCRIPTIVE_REPRESENTATION_ITEM('Steel','Steel');
#13161=DESCRIPTIVE_REPRESENTATION_ITEM('Steel','Steel');
#13162=DESCRIPTIVE_REPRESENTATION_ITEM('Steel','Steel');
#13163=DESCRIPTIVE_REPRESENTATION_ITEM('Steel','Steel');
#13164=DESCRIPTIVE_REPRESENTATION_ITEM('Steel','Steel');
#13165=DESCRIPTIVE_REPRESENTATION_ITEM('Steel','Steel');
#13166=DESCRIPTIVE_REPRESENTATION_ITEM('Steel','Steel');
#13167=DESCRIPTIVE_REPRESENTATION_ITEM('Steel','Steel');
#13168=PROPERTY_DEFINITION('material property','material name',#43823);
#13169=PROPERTY_DEFINITION('material property','density of part',#43823);
#13170=PROPERTY_DEFINITION('material property','material name',#43824);
#13171=PROPERTY_DEFINITION('material property','density of part',#43824);
#13172=PROPERTY_DEFINITION('material property','material name',#43825);
#13173=PROPERTY_DEFINITION('material property','density of part',#43825);
#13174=PROPERTY_DEFINITION('material property','material name',#43826);
#13175=PROPERTY_DEFINITION('material property','density of part',#43826);
#13176=PROPERTY_DEFINITION('material property','material name',#43827);
#13177=PROPERTY_DEFINITION('material property','density of part',#43827);
#13178=PROPERTY_DEFINITION('material property','material name',#43828);
#13179=PROPERTY_DEFINITION('material property','density of part',#43828);
#13180=PROPERTY_DEFINITION('material property','material name',#43829);
#13181=PROPERTY_DEFINITION('material property','density of part',#43829);
#13182=PROPERTY_DEFINITION('material property','material name',#43830);
#13183=PROPERTY_DEFINITION('material property','density of part',#43830);
#13184=AXIS2_PLACEMENT_3D('',#18819,#14913,#14914);
#13185=AXIS2_PLACEMENT_3D('',#18820,#14915,#14916);
#13186=AXIS2_PLACEMENT_3D('',#18821,#14917,#14918);
#13187=AXIS2_PLACEMENT_3D('',#18823,#14919,#14920);
#13188=AXIS2_PLACEMENT_3D('',#18826,#14922,#14923);
#13189=AXIS2_PLACEMENT_3D('',#18827,#14924,#14925);
#13190=AXIS2_PLACEMENT_3D('',#18829,#14926,#14927);
#13191=AXIS2_PLACEMENT_3D('',#18832,#14929,#14930);
#13192=AXIS2_PLACEMENT_3D('',#18833,#14931,#14932);
#13193=AXIS2_PLACEMENT_3D('',#18834,#14933,#14934);
#13194=AXIS2_PLACEMENT_3D('',#18835,#14935,#14936);
#13195=AXIS2_PLACEMENT_3D('',#18838,#14937,#14938);
#13196=AXIS2_PLACEMENT_3D('',#18842,#14940,#14941);
#13197=AXIS2_PLACEMENT_3D('',#18844,#14943,#14944);
#13198=AXIS2_PLACEMENT_3D('',#18850,#14948,#14949);
#13199=AXIS2_PLACEMENT_3D('',#18853,#14950,#14951);
#13200=AXIS2_PLACEMENT_3D('',#18857,#14953,#14954);
#13201=AXIS2_PLACEMENT_3D('',#18859,#14956,#14957);
#13202=AXIS2_PLACEMENT_3D('',#18865,#14961,#14962);
#13203=AXIS2_PLACEMENT_3D('',#18868,#14963,#14964);
#13204=AXIS2_PLACEMENT_3D('',#18872,#14966,#14967);
#13205=AXIS2_PLACEMENT_3D('',#18874,#14969,#14970);
#13206=AXIS2_PLACEMENT_3D('',#18880,#14974,#14975);
#13207=AXIS2_PLACEMENT_3D('',#18883,#14976,#14977);
#13208=AXIS2_PLACEMENT_3D('',#18887,#14979,#14980);
#13209=AXIS2_PLACEMENT_3D('',#18889,#14982,#14983);
#13210=AXIS2_PLACEMENT_3D('',#18895,#14987,#14988);
#13211=AXIS2_PLACEMENT_3D('',#18898,#14989,#14990);
#13212=AXIS2_PLACEMENT_3D('',#18902,#14992,#14993);
#13213=AXIS2_PLACEMENT_3D('',#18904,#14995,#14996);
#13214=AXIS2_PLACEMENT_3D('',#18910,#15000,#15001);
#13215=AXIS2_PLACEMENT_3D('',#18913,#15002,#15003);
#13216=AXIS2_PLACEMENT_3D('',#18917,#15005,#15006);
#13217=AXIS2_PLACEMENT_3D('',#18919,#15008,#15009);
#13218=AXIS2_PLACEMENT_3D('',#18925,#15013,#15014);
#13219=AXIS2_PLACEMENT_3D('',#18928,#15015,#15016);
#13220=AXIS2_PLACEMENT_3D('',#18932,#15018,#15019);
#13221=AXIS2_PLACEMENT_3D('',#18934,#15021,#15022);
#13222=AXIS2_PLACEMENT_3D('',#18940,#15026,#15027);
#13223=AXIS2_PLACEMENT_3D('',#18943,#15028,#15029);
#13224=AXIS2_PLACEMENT_3D('',#18947,#15031,#15032);
#13225=AXIS2_PLACEMENT_3D('',#18949,#15034,#15035);
#13226=AXIS2_PLACEMENT_3D('',#18955,#15039,#15040);
#13227=AXIS2_PLACEMENT_3D('',#18958,#15041,#15042);
#13228=AXIS2_PLACEMENT_3D('',#18962,#15044,#15045);
#13229=AXIS2_PLACEMENT_3D('',#18964,#15047,#15048);
#13230=AXIS2_PLACEMENT_3D('',#18970,#15052,#15053);
#13231=AXIS2_PLACEMENT_3D('',#18973,#15054,#15055);
#13232=AXIS2_PLACEMENT_3D('',#18977,#15057,#15058);
#13233=AXIS2_PLACEMENT_3D('',#18979,#15060,#15061);
#13234=AXIS2_PLACEMENT_3D('',#18985,#15065,#15066);
#13235=AXIS2_PLACEMENT_3D('',#18988,#15067,#15068);
#13236=AXIS2_PLACEMENT_3D('',#18992,#15070,#15071);
#13237=AXIS2_PLACEMENT_3D('',#18994,#15073,#15074);
#13238=AXIS2_PLACEMENT_3D('',#19000,#15078,#15079);
#13239=AXIS2_PLACEMENT_3D('',#19003,#15080,#15081);
#13240=AXIS2_PLACEMENT_3D('',#19007,#15083,#15084);
#13241=AXIS2_PLACEMENT_3D('',#19009,#15086,#15087);
#13242=AXIS2_PLACEMENT_3D('',#19015,#15091,#15092);
#13243=AXIS2_PLACEMENT_3D('',#19018,#15093,#15094);
#13244=AXIS2_PLACEMENT_3D('',#19022,#15096,#15097);
#13245=AXIS2_PLACEMENT_3D('',#19024,#15099,#15100);
#13246=AXIS2_PLACEMENT_3D('',#19030,#15104,#15105);
#13247=AXIS2_PLACEMENT_3D('',#19033,#15106,#15107);
#13248=AXIS2_PLACEMENT_3D('',#19037,#15109,#15110);
#13249=AXIS2_PLACEMENT_3D('',#19039,#15112,#15113);
#13250=AXIS2_PLACEMENT_3D('',#19045,#15117,#15118);
#13251=AXIS2_PLACEMENT_3D('',#19048,#15119,#15120);
#13252=AXIS2_PLACEMENT_3D('',#19052,#15122,#15123);
#13253=AXIS2_PLACEMENT_3D('',#19054,#15125,#15126);
#13254=AXIS2_PLACEMENT_3D('',#19060,#15130,#15131);
#13255=AXIS2_PLACEMENT_3D('',#19063,#15132,#15133);
#13256=AXIS2_PLACEMENT_3D('',#19067,#15135,#15136);
#13257=AXIS2_PLACEMENT_3D('',#19069,#15138,#15139);
#13258=AXIS2_PLACEMENT_3D('',#19075,#15143,#15144);
#13259=AXIS2_PLACEMENT_3D('',#19078,#15145,#15146);
#13260=AXIS2_PLACEMENT_3D('',#19082,#15148,#15149);
#13261=AXIS2_PLACEMENT_3D('',#19084,#15151,#15152);
#13262=AXIS2_PLACEMENT_3D('',#19090,#15156,#15157);
#13263=AXIS2_PLACEMENT_3D('',#19093,#15158,#15159);
#13264=AXIS2_PLACEMENT_3D('',#19097,#15161,#15162);
#13265=AXIS2_PLACEMENT_3D('',#19099,#15164,#15165);
#13266=AXIS2_PLACEMENT_3D('',#19105,#15169,#15170);
#13267=AXIS2_PLACEMENT_3D('',#19108,#15171,#15172);
#13268=AXIS2_PLACEMENT_3D('',#19112,#15174,#15175);
#13269=AXIS2_PLACEMENT_3D('',#19114,#15177,#15178);
#13270=AXIS2_PLACEMENT_3D('',#19120,#15182,#15183);
#13271=AXIS2_PLACEMENT_3D('',#19123,#15184,#15185);
#13272=AXIS2_PLACEMENT_3D('',#19127,#15187,#15188);
#13273=AXIS2_PLACEMENT_3D('',#19129,#15190,#15191);
#13274=AXIS2_PLACEMENT_3D('',#19135,#15195,#15196);
#13275=AXIS2_PLACEMENT_3D('',#19138,#15197,#15198);
#13276=AXIS2_PLACEMENT_3D('',#19142,#15200,#15201);
#13277=AXIS2_PLACEMENT_3D('',#19144,#15203,#15204);
#13278=AXIS2_PLACEMENT_3D('',#19150,#15208,#15209);
#13279=AXIS2_PLACEMENT_3D('',#19153,#15210,#15211);
#13280=AXIS2_PLACEMENT_3D('',#19157,#15213,#15214);
#13281=AXIS2_PLACEMENT_3D('',#19159,#15216,#15217);
#13282=AXIS2_PLACEMENT_3D('',#19165,#15221,#15222);
#13283=AXIS2_PLACEMENT_3D('',#19168,#15223,#15224);
#13284=AXIS2_PLACEMENT_3D('',#19172,#15226,#15227);
#13285=AXIS2_PLACEMENT_3D('',#19174,#15229,#15230);
#13286=AXIS2_PLACEMENT_3D('',#19180,#15234,#15235);
#13287=AXIS2_PLACEMENT_3D('',#19183,#15236,#15237);
#13288=AXIS2_PLACEMENT_3D('',#19187,#15239,#15240);
#13289=AXIS2_PLACEMENT_3D('',#19189,#15242,#15243);
#13290=AXIS2_PLACEMENT_3D('',#19195,#15247,#15248);
#13291=AXIS2_PLACEMENT_3D('',#19198,#15249,#15250);
#13292=AXIS2_PLACEMENT_3D('',#19202,#15252,#15253);
#13293=AXIS2_PLACEMENT_3D('',#19204,#15255,#15256);
#13294=AXIS2_PLACEMENT_3D('',#19210,#15260,#15261);
#13295=AXIS2_PLACEMENT_3D('',#19213,#15262,#15263);
#13296=AXIS2_PLACEMENT_3D('',#19217,#15265,#15266);
#13297=AXIS2_PLACEMENT_3D('',#19219,#15268,#15269);
#13298=AXIS2_PLACEMENT_3D('',#19225,#15273,#15274);
#13299=AXIS2_PLACEMENT_3D('',#19228,#15275,#15276);
#13300=AXIS2_PLACEMENT_3D('',#19232,#15278,#15279);
#13301=AXIS2_PLACEMENT_3D('',#19234,#15281,#15282);
#13302=AXIS2_PLACEMENT_3D('',#19240,#15286,#15287);
#13303=AXIS2_PLACEMENT_3D('',#19243,#15288,#15289);
#13304=AXIS2_PLACEMENT_3D('',#19247,#15291,#15292);
#13305=AXIS2_PLACEMENT_3D('',#19249,#15294,#15295);
#13306=AXIS2_PLACEMENT_3D('',#19255,#15299,#15300);
#13307=AXIS2_PLACEMENT_3D('',#19258,#15301,#15302);
#13308=AXIS2_PLACEMENT_3D('',#19262,#15304,#15305);
#13309=AXIS2_PLACEMENT_3D('',#19264,#15307,#15308);
#13310=AXIS2_PLACEMENT_3D('',#19270,#15312,#15313);
#13311=AXIS2_PLACEMENT_3D('',#19273,#15314,#15315);
#13312=AXIS2_PLACEMENT_3D('',#19277,#15317,#15318);
#13313=AXIS2_PLACEMENT_3D('',#19279,#15320,#15321);
#13314=AXIS2_PLACEMENT_3D('',#19285,#15325,#15326);
#13315=AXIS2_PLACEMENT_3D('',#19288,#15327,#15328);
#13316=AXIS2_PLACEMENT_3D('',#19292,#15330,#15331);
#13317=AXIS2_PLACEMENT_3D('',#19294,#15333,#15334);
#13318=AXIS2_PLACEMENT_3D('',#19300,#15338,#15339);
#13319=AXIS2_PLACEMENT_3D('',#19303,#15340,#15341);
#13320=AXIS2_PLACEMENT_3D('',#19307,#15343,#15344);
#13321=AXIS2_PLACEMENT_3D('',#19309,#15346,#15347);
#13322=AXIS2_PLACEMENT_3D('',#19315,#15351,#15352);
#13323=AXIS2_PLACEMENT_3D('',#19318,#15353,#15354);
#13324=AXIS2_PLACEMENT_3D('',#19322,#15356,#15357);
#13325=AXIS2_PLACEMENT_3D('',#19324,#15359,#15360);
#13326=AXIS2_PLACEMENT_3D('',#19330,#15364,#15365);
#13327=AXIS2_PLACEMENT_3D('',#19333,#15366,#15367);
#13328=AXIS2_PLACEMENT_3D('',#19337,#15369,#15370);
#13329=AXIS2_PLACEMENT_3D('',#19339,#15372,#15373);
#13330=AXIS2_PLACEMENT_3D('',#19345,#15377,#15378);
#13331=AXIS2_PLACEMENT_3D('',#19348,#15379,#15380);
#13332=AXIS2_PLACEMENT_3D('',#19352,#15382,#15383);
#13333=AXIS2_PLACEMENT_3D('',#19354,#15385,#15386);
#13334=AXIS2_PLACEMENT_3D('',#19360,#15390,#15391);
#13335=AXIS2_PLACEMENT_3D('',#19363,#15392,#15393);
#13336=AXIS2_PLACEMENT_3D('',#19367,#15395,#15396);
#13337=AXIS2_PLACEMENT_3D('',#19369,#15398,#15399);
#13338=AXIS2_PLACEMENT_3D('',#19375,#15403,#15404);
#13339=AXIS2_PLACEMENT_3D('',#19378,#15405,#15406);
#13340=AXIS2_PLACEMENT_3D('',#19382,#15408,#15409);
#13341=AXIS2_PLACEMENT_3D('',#19384,#15411,#15412);
#13342=AXIS2_PLACEMENT_3D('',#19390,#15416,#15417);
#13343=AXIS2_PLACEMENT_3D('',#19393,#15418,#15419);
#13344=AXIS2_PLACEMENT_3D('',#19397,#15421,#15422);
#13345=AXIS2_PLACEMENT_3D('',#19399,#15424,#15425);
#13346=AXIS2_PLACEMENT_3D('',#19707,#15430,#15431);
#13347=AXIS2_PLACEMENT_3D('',#19709,#15432,#15433);
#13348=AXIS2_PLACEMENT_3D('',#19711,#15434,#15435);
#13349=AXIS2_PLACEMENT_3D('',#20313,#15438,#15439);
#13350=AXIS2_PLACEMENT_3D('',#20315,#15440,#15441);
#13351=AXIS2_PLACEMENT_3D('',#20317,#15442,#15443);
#13352=AXIS2_PLACEMENT_3D('',#20919,#15446,#15447);
#13353=AXIS2_PLACEMENT_3D('',#20921,#15448,#15449);
#13354=AXIS2_PLACEMENT_3D('',#20923,#15450,#15451);
#13355=AXIS2_PLACEMENT_3D('',#21525,#15454,#15455);
#13356=AXIS2_PLACEMENT_3D('',#21527,#15456,#15457);
#13357=AXIS2_PLACEMENT_3D('',#21529,#15458,#15459);
#13358=AXIS2_PLACEMENT_3D('',#22131,#15462,#15463);
#13359=AXIS2_PLACEMENT_3D('',#22133,#15464,#15465);
#13360=AXIS2_PLACEMENT_3D('',#22135,#15466,#15467);
#13361=AXIS2_PLACEMENT_3D('',#22737,#15470,#15471);
#13362=AXIS2_PLACEMENT_3D('',#22739,#15472,#15473);
#13363=AXIS2_PLACEMENT_3D('',#22741,#15474,#15475);
#13364=AXIS2_PLACEMENT_3D('',#23343,#15478,#15479);
#13365=AXIS2_PLACEMENT_3D('',#23345,#15480,#15481);
#13366=AXIS2_PLACEMENT_3D('',#23347,#15482,#15483);
#13367=AXIS2_PLACEMENT_3D('',#23949,#15486,#15487);
#13368=AXIS2_PLACEMENT_3D('',#23951,#15488,#15489);
#13369=AXIS2_PLACEMENT_3D('',#23953,#15490,#15491);
#13370=AXIS2_PLACEMENT_3D('',#24555,#15494,#15495);
#13371=AXIS2_PLACEMENT_3D('',#24557,#15496,#15497);
#13372=AXIS2_PLACEMENT_3D('',#24559,#15498,#15499);
#13373=AXIS2_PLACEMENT_3D('',#25161,#15502,#15503);
#13374=AXIS2_PLACEMENT_3D('',#25163,#15504,#15505);
#13375=AXIS2_PLACEMENT_3D('',#25165,#15506,#15507);
#13376=AXIS2_PLACEMENT_3D('',#25767,#15510,#15511);
#13377=AXIS2_PLACEMENT_3D('',#25769,#15512,#15513);
#13378=AXIS2_PLACEMENT_3D('',#25771,#15514,#15515);
#13379=AXIS2_PLACEMENT_3D('',#26373,#15518,#15519);
#13380=AXIS2_PLACEMENT_3D('',#26375,#15520,#15521);
#13381=AXIS2_PLACEMENT_3D('',#26377,#15522,#15523);
#13382=AXIS2_PLACEMENT_3D('',#26979,#15526,#15527);
#13383=AXIS2_PLACEMENT_3D('',#26981,#15528,#15529);
#13384=AXIS2_PLACEMENT_3D('',#26983,#15530,#15531);
#13385=AXIS2_PLACEMENT_3D('',#27585,#15534,#15535);
#13386=AXIS2_PLACEMENT_3D('',#27587,#15536,#15537);
#13387=AXIS2_PLACEMENT_3D('',#27589,#15538,#15539);
#13388=AXIS2_PLACEMENT_3D('',#28191,#15542,#15543);
#13389=AXIS2_PLACEMENT_3D('',#28193,#15544,#15545);
#13390=AXIS2_PLACEMENT_3D('',#28195,#15546,#15547);
#13391=AXIS2_PLACEMENT_3D('',#28797,#15550,#15551);
#13392=AXIS2_PLACEMENT_3D('',#28799,#15552,#15553);
#13393=AXIS2_PLACEMENT_3D('',#28801,#15554,#15555);
#13394=AXIS2_PLACEMENT_3D('',#29403,#15558,#15559);
#13395=AXIS2_PLACEMENT_3D('',#29405,#15560,#15561);
#13396=AXIS2_PLACEMENT_3D('',#29407,#15562,#15563);
#13397=AXIS2_PLACEMENT_3D('',#30009,#15566,#15567);
#13398=AXIS2_PLACEMENT_3D('',#30011,#15568,#15569);
#13399=AXIS2_PLACEMENT_3D('',#30013,#15570,#15571);
#13400=AXIS2_PLACEMENT_3D('',#30615,#15574,#15575);
#13401=AXIS2_PLACEMENT_3D('',#30617,#15576,#15577);
#13402=AXIS2_PLACEMENT_3D('',#30619,#15578,#15579);
#13403=AXIS2_PLACEMENT_3D('',#30919,#15581,#15582);
#13404=AXIS2_PLACEMENT_3D('',#30920,#15583,#15584);
#13405=AXIS2_PLACEMENT_3D('',#30921,#15585,#15586);
#13406=AXIS2_PLACEMENT_3D('',#30922,#15587,#15588);
#13407=AXIS2_PLACEMENT_3D('',#30923,#15589,#15590);
#13408=AXIS2_PLACEMENT_3D('',#30924,#15591,#15592);
#13409=AXIS2_PLACEMENT_3D('',#30925,#15593,#15594);
#13410=AXIS2_PLACEMENT_3D('',#30926,#15595,#15596);
#13411=AXIS2_PLACEMENT_3D('',#30927,#15597,#15598);
#13412=AXIS2_PLACEMENT_3D('',#30928,#15599,#15600);
#13413=AXIS2_PLACEMENT_3D('',#30929,#15601,#15602);
#13414=AXIS2_PLACEMENT_3D('',#30930,#15603,#15604);
#13415=AXIS2_PLACEMENT_3D('',#30931,#15605,#15606);
#13416=AXIS2_PLACEMENT_3D('',#30932,#15607,#15608);
#13417=AXIS2_PLACEMENT_3D('',#30933,#15609,#15610);
#13418=AXIS2_PLACEMENT_3D('',#30934,#15611,#15612);
#13419=AXIS2_PLACEMENT_3D('',#30935,#15613,#15614);
#13420=AXIS2_PLACEMENT_3D('',#30936,#15615,#15616);
#13421=AXIS2_PLACEMENT_3D('',#30938,#15617,#15618);
#13422=AXIS2_PLACEMENT_3D('',#30940,#15619,#15620);
#13423=AXIS2_PLACEMENT_3D('',#31019,#15622,#15623);
#13424=AXIS2_PLACEMENT_3D('',#31098,#15625,#15626);
#13425=AXIS2_PLACEMENT_3D('',#31099,#15627,#15628);
#13426=AXIS2_PLACEMENT_3D('',#31100,#15629,#15630);
#13427=AXIS2_PLACEMENT_3D('',#31101,#15631,#15632);
#13428=AXIS2_PLACEMENT_3D('',#31103,#15633,#15634);
#13429=AXIS2_PLACEMENT_3D('',#31105,#15635,#15636);
#13430=AXIS2_PLACEMENT_3D('',#31184,#15638,#15639);
#13431=AXIS2_PLACEMENT_3D('',#31264,#15641,#15642);
#13432=AXIS2_PLACEMENT_3D('',#31265,#15643,#15644);
#13433=AXIS2_PLACEMENT_3D('',#31266,#15645,#15646);
#13434=AXIS2_PLACEMENT_3D('',#31267,#15647,#15648);
#13435=AXIS2_PLACEMENT_3D('',#31268,#15649,#15650);
#13436=AXIS2_PLACEMENT_3D('',#31269,#15651,#15652);
#13437=AXIS2_PLACEMENT_3D('',#31270,#15653,#15654);
#13438=AXIS2_PLACEMENT_3D('',#31271,#15655,#15656);
#13439=AXIS2_PLACEMENT_3D('',#31272,#15657,#15658);
#13440=AXIS2_PLACEMENT_3D('',#31273,#15659,#15660);
#13441=AXIS2_PLACEMENT_3D('',#31274,#15661,#15662);
#13442=AXIS2_PLACEMENT_3D('',#31275,#15663,#15664);
#13443=AXIS2_PLACEMENT_3D('',#31276,#15665,#15666);
#13444=AXIS2_PLACEMENT_3D('',#31277,#15667,#15668);
#13445=AXIS2_PLACEMENT_3D('',#31278,#15669,#15670);
#13446=AXIS2_PLACEMENT_3D('',#31279,#15671,#15672);
#13447=AXIS2_PLACEMENT_3D('',#31280,#15673,#15674);
#13448=AXIS2_PLACEMENT_3D('',#31281,#15675,#15676);
#13449=AXIS2_PLACEMENT_3D('',#31282,#15677,#15678);
#13450=AXIS2_PLACEMENT_3D('',#31283,#15679,#15680);
#13451=AXIS2_PLACEMENT_3D('',#31284,#15681,#15682);
#13452=AXIS2_PLACEMENT_3D('',#31286,#15684,#15685);
#13453=AXIS2_PLACEMENT_3D('',#31287,#15686,#15687);
#13454=AXIS2_PLACEMENT_3D('',#31288,#15688,#15689);
#13455=AXIS2_PLACEMENT_3D('',#31289,#15690,#15691);
#13456=AXIS2_PLACEMENT_3D('',#31290,#15692,#15693);
#13457=AXIS2_PLACEMENT_3D('',#31291,#15694,#15695);
#13458=AXIS2_PLACEMENT_3D('',#31292,#15696,#15697);
#13459=AXIS2_PLACEMENT_3D('',#31293,#15698,#15699);
#13460=AXIS2_PLACEMENT_3D('',#31294,#15700,#15701);
#13461=AXIS2_PLACEMENT_3D('',#31295,#15702,#15703);
#13462=AXIS2_PLACEMENT_3D('',#31296,#15704,#15705);
#13463=AXIS2_PLACEMENT_3D('',#31297,#15706,#15707);
#13464=AXIS2_PLACEMENT_3D('',#31298,#15708,#15709);
#13465=AXIS2_PLACEMENT_3D('',#31299,#15710,#15711);
#13466=AXIS2_PLACEMENT_3D('',#31300,#15712,#15713);
#13467=AXIS2_PLACEMENT_3D('',#31301,#15714,#15715);
#13468=AXIS2_PLACEMENT_3D('',#31302,#15716,#15717);
#13469=AXIS2_PLACEMENT_3D('',#31303,#15718,#15719);
#13470=AXIS2_PLACEMENT_3D('',#31304,#15720,#15721);
#13471=AXIS2_PLACEMENT_3D('',#31306,#15723,#15724);
#13472=AXIS2_PLACEMENT_3D('',#31308,#15726,#15727);
#13473=AXIS2_PLACEMENT_3D('',#31311,#15730,#15731);
#13474=AXIS2_PLACEMENT_3D('',#31464,#15734,#15735);
#13475=AXIS2_PLACEMENT_3D('',#31616,#15737,#15738);
#13476=AXIS2_PLACEMENT_3D('',#31617,#15739,#15740);
#13477=AXIS2_PLACEMENT_3D('',#31618,#15741,#15742);
#13478=AXIS2_PLACEMENT_3D('',#31620,#15743,#15744);
#13479=AXIS2_PLACEMENT_3D('',#31623,#15746,#15747);
#13480=AXIS2_PLACEMENT_3D('',#31624,#15748,#15749);
#13481=AXIS2_PLACEMENT_3D('',#31626,#15750,#15751);
#13482=AXIS2_PLACEMENT_3D('',#31629,#15753,#15754);
#13483=AXIS2_PLACEMENT_3D('',#31630,#15755,#15756);
#13484=AXIS2_PLACEMENT_3D('',#31631,#15757,#15758);
#13485=AXIS2_PLACEMENT_3D('',#31632,#15759,#15760);
#13486=AXIS2_PLACEMENT_3D('',#31635,#15761,#15762);
#13487=AXIS2_PLACEMENT_3D('',#31639,#15764,#15765);
#13488=AXIS2_PLACEMENT_3D('',#31641,#15767,#15768);
#13489=AXIS2_PLACEMENT_3D('',#31647,#15772,#15773);
#13490=AXIS2_PLACEMENT_3D('',#31650,#15774,#15775);
#13491=AXIS2_PLACEMENT_3D('',#31654,#15777,#15778);
#13492=AXIS2_PLACEMENT_3D('',#31656,#15780,#15781);
#13493=AXIS2_PLACEMENT_3D('',#31662,#15785,#15786);
#13494=AXIS2_PLACEMENT_3D('',#31665,#15787,#15788);
#13495=AXIS2_PLACEMENT_3D('',#31669,#15790,#15791);
#13496=AXIS2_PLACEMENT_3D('',#31671,#15793,#15794);
#13497=AXIS2_PLACEMENT_3D('',#31677,#15798,#15799);
#13498=AXIS2_PLACEMENT_3D('',#31680,#15800,#15801);
#13499=AXIS2_PLACEMENT_3D('',#31684,#15803,#15804);
#13500=AXIS2_PLACEMENT_3D('',#31686,#15806,#15807);
#13501=AXIS2_PLACEMENT_3D('',#31692,#15811,#15812);
#13502=AXIS2_PLACEMENT_3D('',#31695,#15813,#15814);
#13503=AXIS2_PLACEMENT_3D('',#31699,#15816,#15817);
#13504=AXIS2_PLACEMENT_3D('',#31701,#15819,#15820);
#13505=AXIS2_PLACEMENT_3D('',#31707,#15824,#15825);
#13506=AXIS2_PLACEMENT_3D('',#31710,#15826,#15827);
#13507=AXIS2_PLACEMENT_3D('',#31714,#15829,#15830);
#13508=AXIS2_PLACEMENT_3D('',#31716,#15832,#15833);
#13509=AXIS2_PLACEMENT_3D('',#31722,#15837,#15838);
#13510=AXIS2_PLACEMENT_3D('',#31725,#15839,#15840);
#13511=AXIS2_PLACEMENT_3D('',#31729,#15842,#15843);
#13512=AXIS2_PLACEMENT_3D('',#31731,#15845,#15846);
#13513=AXIS2_PLACEMENT_3D('',#31737,#15850,#15851);
#13514=AXIS2_PLACEMENT_3D('',#31740,#15852,#15853);
#13515=AXIS2_PLACEMENT_3D('',#31744,#15855,#15856);
#13516=AXIS2_PLACEMENT_3D('',#31746,#15858,#15859);
#13517=AXIS2_PLACEMENT_3D('',#31752,#15863,#15864);
#13518=AXIS2_PLACEMENT_3D('',#31755,#15865,#15866);
#13519=AXIS2_PLACEMENT_3D('',#31759,#15868,#15869);
#13520=AXIS2_PLACEMENT_3D('',#31761,#15871,#15872);
#13521=AXIS2_PLACEMENT_3D('',#31767,#15876,#15877);
#13522=AXIS2_PLACEMENT_3D('',#31770,#15878,#15879);
#13523=AXIS2_PLACEMENT_3D('',#31774,#15881,#15882);
#13524=AXIS2_PLACEMENT_3D('',#31776,#15884,#15885);
#13525=AXIS2_PLACEMENT_3D('',#31782,#15889,#15890);
#13526=AXIS2_PLACEMENT_3D('',#31785,#15891,#15892);
#13527=AXIS2_PLACEMENT_3D('',#31789,#15894,#15895);
#13528=AXIS2_PLACEMENT_3D('',#31791,#15897,#15898);
#13529=AXIS2_PLACEMENT_3D('',#31797,#15902,#15903);
#13530=AXIS2_PLACEMENT_3D('',#31800,#15904,#15905);
#13531=AXIS2_PLACEMENT_3D('',#31804,#15907,#15908);
#13532=AXIS2_PLACEMENT_3D('',#31806,#15910,#15911);
#13533=AXIS2_PLACEMENT_3D('',#31812,#15915,#15916);
#13534=AXIS2_PLACEMENT_3D('',#31815,#15917,#15918);
#13535=AXIS2_PLACEMENT_3D('',#31819,#15920,#15921);
#13536=AXIS2_PLACEMENT_3D('',#31821,#15923,#15924);
#13537=AXIS2_PLACEMENT_3D('',#31827,#15928,#15929);
#13538=AXIS2_PLACEMENT_3D('',#31830,#15930,#15931);
#13539=AXIS2_PLACEMENT_3D('',#31834,#15933,#15934);
#13540=AXIS2_PLACEMENT_3D('',#31836,#15936,#15937);
#13541=AXIS2_PLACEMENT_3D('',#31842,#15941,#15942);
#13542=AXIS2_PLACEMENT_3D('',#31845,#15943,#15944);
#13543=AXIS2_PLACEMENT_3D('',#31849,#15946,#15947);
#13544=AXIS2_PLACEMENT_3D('',#31851,#15949,#15950);
#13545=AXIS2_PLACEMENT_3D('',#31857,#15954,#15955);
#13546=AXIS2_PLACEMENT_3D('',#31860,#15956,#15957);
#13547=AXIS2_PLACEMENT_3D('',#31864,#15959,#15960);
#13548=AXIS2_PLACEMENT_3D('',#31866,#15962,#15963);
#13549=AXIS2_PLACEMENT_3D('',#31872,#15967,#15968);
#13550=AXIS2_PLACEMENT_3D('',#31875,#15969,#15970);
#13551=AXIS2_PLACEMENT_3D('',#31879,#15972,#15973);
#13552=AXIS2_PLACEMENT_3D('',#31881,#15975,#15976);
#13553=AXIS2_PLACEMENT_3D('',#31887,#15980,#15981);
#13554=AXIS2_PLACEMENT_3D('',#31890,#15982,#15983);
#13555=AXIS2_PLACEMENT_3D('',#31894,#15985,#15986);
#13556=AXIS2_PLACEMENT_3D('',#31896,#15988,#15989);
#13557=AXIS2_PLACEMENT_3D('',#32204,#15994,#15995);
#13558=AXIS2_PLACEMENT_3D('',#32206,#15996,#15997);
#13559=AXIS2_PLACEMENT_3D('',#32208,#15998,#15999);
#13560=AXIS2_PLACEMENT_3D('',#32810,#16002,#16003);
#13561=AXIS2_PLACEMENT_3D('',#32812,#16004,#16005);
#13562=AXIS2_PLACEMENT_3D('',#32814,#16006,#16007);
#13563=AXIS2_PLACEMENT_3D('',#33416,#16010,#16011);
#13564=AXIS2_PLACEMENT_3D('',#33418,#16012,#16013);
#13565=AXIS2_PLACEMENT_3D('',#33420,#16014,#16015);
#13566=AXIS2_PLACEMENT_3D('',#34022,#16018,#16019);
#13567=AXIS2_PLACEMENT_3D('',#34024,#16020,#16021);
#13568=AXIS2_PLACEMENT_3D('',#34026,#16022,#16023);
#13569=AXIS2_PLACEMENT_3D('',#34628,#16026,#16027);
#13570=AXIS2_PLACEMENT_3D('',#34630,#16028,#16029);
#13571=AXIS2_PLACEMENT_3D('',#34632,#16030,#16031);
#13572=AXIS2_PLACEMENT_3D('',#35234,#16034,#16035);
#13573=AXIS2_PLACEMENT_3D('',#35236,#16036,#16037);
#13574=AXIS2_PLACEMENT_3D('',#35238,#16038,#16039);
#13575=AXIS2_PLACEMENT_3D('',#35840,#16042,#16043);
#13576=AXIS2_PLACEMENT_3D('',#35842,#16044,#16045);
#13577=AXIS2_PLACEMENT_3D('',#35844,#16046,#16047);
#13578=AXIS2_PLACEMENT_3D('',#36446,#16050,#16051);
#13579=AXIS2_PLACEMENT_3D('',#36448,#16052,#16053);
#13580=AXIS2_PLACEMENT_3D('',#36450,#16054,#16055);
#13581=AXIS2_PLACEMENT_3D('',#37052,#16058,#16059);
#13582=AXIS2_PLACEMENT_3D('',#37054,#16060,#16061);
#13583=AXIS2_PLACEMENT_3D('',#37056,#16062,#16063);
#13584=AXIS2_PLACEMENT_3D('',#37356,#16065,#16066);
#13585=AXIS2_PLACEMENT_3D('',#37357,#16067,#16068);
#13586=AXIS2_PLACEMENT_3D('',#37358,#16069,#16070);
#13587=AXIS2_PLACEMENT_3D('',#37359,#16071,#16072);
#13588=AXIS2_PLACEMENT_3D('',#37360,#16073,#16074);
#13589=AXIS2_PLACEMENT_3D('',#37361,#16075,#16076);
#13590=AXIS2_PLACEMENT_3D('',#37362,#16077,#16078);
#13591=AXIS2_PLACEMENT_3D('',#37363,#16079,#16080);
#13592=AXIS2_PLACEMENT_3D('',#37365,#16081,#16082);
#13593=AXIS2_PLACEMENT_3D('',#37367,#16083,#16084);
#13594=AXIS2_PLACEMENT_3D('',#37446,#16086,#16087);
#13595=AXIS2_PLACEMENT_3D('',#37525,#16089,#16090);
#13596=AXIS2_PLACEMENT_3D('',#37526,#16091,#16092);
#13597=AXIS2_PLACEMENT_3D('',#37527,#16093,#16094);
#13598=AXIS2_PLACEMENT_3D('',#37528,#16095,#16096);
#13599=AXIS2_PLACEMENT_3D('',#37530,#16097,#16098);
#13600=AXIS2_PLACEMENT_3D('',#37532,#16099,#16100);
#13601=AXIS2_PLACEMENT_3D('',#37611,#16102,#16103);
#13602=AXIS2_PLACEMENT_3D('',#37691,#16105,#16106);
#13603=AXIS2_PLACEMENT_3D('',#37692,#16107,#16108);
#13604=AXIS2_PLACEMENT_3D('',#37693,#16109,#16110);
#13605=AXIS2_PLACEMENT_3D('',#37694,#16111,#16112);
#13606=AXIS2_PLACEMENT_3D('',#37695,#16113,#16114);
#13607=AXIS2_PLACEMENT_3D('',#37696,#16115,#16116);
#13608=AXIS2_PLACEMENT_3D('',#37697,#16117,#16118);
#13609=AXIS2_PLACEMENT_3D('',#37698,#16119,#16120);
#13610=AXIS2_PLACEMENT_3D('',#37699,#16121,#16122);
#13611=AXIS2_PLACEMENT_3D('',#37700,#16123,#16124);
#13612=AXIS2_PLACEMENT_3D('',#37701,#16125,#16126);
#13613=AXIS2_PLACEMENT_3D('',#37703,#16128,#16129);
#13614=AXIS2_PLACEMENT_3D('',#37704,#16130,#16131);
#13615=AXIS2_PLACEMENT_3D('',#37705,#16132,#16133);
#13616=AXIS2_PLACEMENT_3D('',#37706,#16134,#16135);
#13617=AXIS2_PLACEMENT_3D('',#37707,#16136,#16137);
#13618=AXIS2_PLACEMENT_3D('',#37708,#16138,#16139);
#13619=AXIS2_PLACEMENT_3D('',#37709,#16140,#16141);
#13620=AXIS2_PLACEMENT_3D('',#37710,#16142,#16143);
#13621=AXIS2_PLACEMENT_3D('',#37711,#16144,#16145);
#13622=AXIS2_PLACEMENT_3D('',#37713,#16147,#16148);
#13623=AXIS2_PLACEMENT_3D('',#37715,#16150,#16151);
#13624=AXIS2_PLACEMENT_3D('',#37718,#16154,#16155);
#13625=AXIS2_PLACEMENT_3D('',#37871,#16158,#16159);
#13626=AXIS2_PLACEMENT_3D('',#38023,#16161,#16162);
#13627=AXIS2_PLACEMENT_3D('',#38024,#16163,#16164);
#13628=AXIS2_PLACEMENT_3D('',#38025,#16165,#16166);
#13629=AXIS2_PLACEMENT_3D('',#38027,#16167,#16168);
#13630=AXIS2_PLACEMENT_3D('',#38029,#16169,#16170);
#13631=AXIS2_PLACEMENT_3D('',#38030,#16171,#16172);
#13632=AXIS2_PLACEMENT_3D('',#38031,#16173,#16174);
#13633=AXIS2_PLACEMENT_3D('',#38034,#16175,#16176);
#13634=AXIS2_PLACEMENT_3D('',#38035,#16177,#16178);
#13635=AXIS2_PLACEMENT_3D('',#38037,#16179,#16180);
#13636=AXIS2_PLACEMENT_3D('',#38039,#16181,#16182);
#13637=AXIS2_PLACEMENT_3D('',#38040,#16183,#16184);
#13638=AXIS2_PLACEMENT_3D('',#38041,#16185,#16186);
#13639=AXIS2_PLACEMENT_3D('',#38044,#16187,#16188);
#13640=AXIS2_PLACEMENT_3D('',#38045,#16189,#16190);
#13641=AXIS2_PLACEMENT_3D('',#38047,#16191,#16192);
#13642=AXIS2_PLACEMENT_3D('',#38048,#16193,#16194);
#13643=AXIS2_PLACEMENT_3D('',#38049,#16195,#16196);
#13644=AXIS2_PLACEMENT_3D('',#38052,#16198,#16199);
#13645=AXIS2_PLACEMENT_3D('',#38053,#16200,#16201);
#13646=AXIS2_PLACEMENT_3D('',#38055,#16203,#16204);
#13647=AXIS2_PLACEMENT_3D('',#38058,#16206,#16207);
#13648=AXIS2_PLACEMENT_3D('',#38059,#16208,#16209);
#13649=AXIS2_PLACEMENT_3D('',#38062,#16211,#16212);
#13650=AXIS2_PLACEMENT_3D('',#38063,#16213,#16214);
#13651=AXIS2_PLACEMENT_3D('',#38065,#16215,#16216);
#13652=AXIS2_PLACEMENT_3D('',#38067,#16218,#16219);
#13653=AXIS2_PLACEMENT_3D('',#38068,#16220,#16221);
#13654=AXIS2_PLACEMENT_3D('',#38069,#16222,#16223);
#13655=AXIS2_PLACEMENT_3D('',#38072,#16224,#16225);
#13656=AXIS2_PLACEMENT_3D('',#38073,#16226,#16227);
#13657=AXIS2_PLACEMENT_3D('',#38076,#16228,#16229);
#13658=AXIS2_PLACEMENT_3D('',#38077,#16230,#16231);
#13659=AXIS2_PLACEMENT_3D('',#38080,#16232,#16233);
#13660=AXIS2_PLACEMENT_3D('',#38081,#16234,#16235);
#13661=AXIS2_PLACEMENT_3D('',#38084,#16236,#16237);
#13662=AXIS2_PLACEMENT_3D('',#38085,#16238,#16239);
#13663=AXIS2_PLACEMENT_3D('',#38088,#16240,#16241);
#13664=AXIS2_PLACEMENT_3D('',#38089,#16242,#16243);
#13665=AXIS2_PLACEMENT_3D('',#38092,#16244,#16245);
#13666=AXIS2_PLACEMENT_3D('',#38093,#16246,#16247);
#13667=AXIS2_PLACEMENT_3D('',#38096,#16248,#16249);
#13668=AXIS2_PLACEMENT_3D('',#38097,#16250,#16251);
#13669=AXIS2_PLACEMENT_3D('',#38099,#16252,#16253);
#13670=AXIS2_PLACEMENT_3D('',#38101,#16254,#16255);
#13671=AXIS2_PLACEMENT_3D('',#38103,#16256,#16257);
#13672=AXIS2_PLACEMENT_3D('',#38104,#16258,#16259);
#13673=AXIS2_PLACEMENT_3D('',#38105,#16260,#16261);
#13674=AXIS2_PLACEMENT_3D('',#38107,#16262,#16263);
#13675=AXIS2_PLACEMENT_3D('',#38109,#16264,#16265);
#13676=AXIS2_PLACEMENT_3D('',#38110,#16266,#16267);
#13677=AXIS2_PLACEMENT_3D('',#38111,#16268,#16269);
#13678=AXIS2_PLACEMENT_3D('',#38113,#16270,#16271);
#13679=AXIS2_PLACEMENT_3D('',#38115,#16272,#16273);
#13680=AXIS2_PLACEMENT_3D('',#38116,#16274,#16275);
#13681=AXIS2_PLACEMENT_3D('',#38117,#16276,#16277);
#13682=AXIS2_PLACEMENT_3D('',#38120,#16278,#16279);
#13683=AXIS2_PLACEMENT_3D('',#38121,#16280,#16281);
#13684=AXIS2_PLACEMENT_3D('',#38123,#16282,#16283);
#13685=AXIS2_PLACEMENT_3D('',#38124,#16284,#16285);
#13686=AXIS2_PLACEMENT_3D('',#38125,#16286,#16287);
#13687=AXIS2_PLACEMENT_3D('',#38127,#16288,#16289);
#13688=AXIS2_PLACEMENT_3D('',#38130,#16291,#16292);
#13689=AXIS2_PLACEMENT_3D('',#38131,#16293,#16294);
#13690=AXIS2_PLACEMENT_3D('',#38133,#16295,#16296);
#13691=AXIS2_PLACEMENT_3D('',#38135,#16298,#16299);
#13692=AXIS2_PLACEMENT_3D('',#38138,#16301,#16302);
#13693=AXIS2_PLACEMENT_3D('',#38139,#16303,#16304);
#13694=AXIS2_PLACEMENT_3D('',#38141,#16305,#16306);
#13695=AXIS2_PLACEMENT_3D('',#38142,#16307,#16308);
#13696=AXIS2_PLACEMENT_3D('',#38143,#16309,#16310);
#13697=AXIS2_PLACEMENT_3D('',#38145,#16312,#16313);
#13698=AXIS2_PLACEMENT_3D('',#38148,#16315,#16316);
#13699=AXIS2_PLACEMENT_3D('',#38149,#16317,#16318);
#13700=AXIS2_PLACEMENT_3D('',#38151,#16319,#16320);
#13701=AXIS2_PLACEMENT_3D('',#38154,#16322,#16323);
#13702=AXIS2_PLACEMENT_3D('',#38155,#16324,#16325);
#13703=AXIS2_PLACEMENT_3D('',#38157,#16326,#16327);
#13704=AXIS2_PLACEMENT_3D('',#38160,#16329,#16330);
#13705=AXIS2_PLACEMENT_3D('',#38161,#16331,#16332);
#13706=AXIS2_PLACEMENT_3D('',#38164,#16333,#16334);
#13707=AXIS2_PLACEMENT_3D('',#38167,#16336,#16337);
#13708=AXIS2_PLACEMENT_3D('',#38168,#16338,#16339);
#13709=AXIS2_PLACEMENT_3D('',#38169,#16340,#16341);
#13710=AXIS2_PLACEMENT_3D('',#38171,#16343,#16344);
#13711=AXIS2_PLACEMENT_3D('',#38172,#16345,#16346);
#13712=AXIS2_PLACEMENT_3D('',#38173,#16347,#16348);
#13713=AXIS2_PLACEMENT_3D('',#38174,#16349,#16350);
#13714=AXIS2_PLACEMENT_3D('',#38175,#16351,#16352);
#13715=AXIS2_PLACEMENT_3D('',#38176,#16353,#16354);
#13716=AXIS2_PLACEMENT_3D('',#38177,#16355,#16356);
#13717=AXIS2_PLACEMENT_3D('',#38179,#16357,#16358);
#13718=AXIS2_PLACEMENT_3D('',#38181,#16359,#16360);
#13719=AXIS2_PLACEMENT_3D('',#38182,#16361,#16362);
#13720=AXIS2_PLACEMENT_3D('',#38291,#16363,#16364);
#13721=AXIS2_PLACEMENT_3D('',#38294,#16365,#16366);
#13722=AXIS2_PLACEMENT_3D('',#38296,#16367,#16368);
#13723=AXIS2_PLACEMENT_3D('',#38298,#16369,#16370);
#13724=AXIS2_PLACEMENT_3D('',#38308,#16371,#16372);
#13725=AXIS2_PLACEMENT_3D('',#38317,#16373,#16374);
#13726=AXIS2_PLACEMENT_3D('',#38319,#16375,#16376);
#13727=AXIS2_PLACEMENT_3D('',#38328,#16377,#16378);
#13728=AXIS2_PLACEMENT_3D('',#38336,#16379,#16380);
#13729=AXIS2_PLACEMENT_3D('',#38338,#16381,#16382);
#13730=AXIS2_PLACEMENT_3D('',#38339,#16383,#16384);
#13731=AXIS2_PLACEMENT_3D('',#38341,#16385,#16386);
#13732=AXIS2_PLACEMENT_3D('',#38343,#16387,#16388);
#13733=AXIS2_PLACEMENT_3D('',#38344,#16389,#16390);
#13734=AXIS2_PLACEMENT_3D('',#38453,#16391,#16392);
#13735=AXIS2_PLACEMENT_3D('',#38456,#16393,#16394);
#13736=AXIS2_PLACEMENT_3D('',#38458,#16395,#16396);
#13737=AXIS2_PLACEMENT_3D('',#38460,#16397,#16398);
#13738=AXIS2_PLACEMENT_3D('',#38470,#16399,#16400);
#13739=AXIS2_PLACEMENT_3D('',#38479,#16401,#16402);
#13740=AXIS2_PLACEMENT_3D('',#38481,#16403,#16404);
#13741=AXIS2_PLACEMENT_3D('',#38490,#16405,#16406);
#13742=AXIS2_PLACEMENT_3D('',#38498,#16407,#16408);
#13743=AXIS2_PLACEMENT_3D('',#38500,#16409,#16410);
#13744=AXIS2_PLACEMENT_3D('',#38501,#16411,#16412);
#13745=AXIS2_PLACEMENT_3D('',#38503,#16413,#16414);
#13746=AXIS2_PLACEMENT_3D('',#38505,#16415,#16416);
#13747=AXIS2_PLACEMENT_3D('',#38506,#16417,#16418);
#13748=AXIS2_PLACEMENT_3D('',#38615,#16419,#16420);
#13749=AXIS2_PLACEMENT_3D('',#38618,#16421,#16422);
#13750=AXIS2_PLACEMENT_3D('',#38620,#16423,#16424);
#13751=AXIS2_PLACEMENT_3D('',#38622,#16425,#16426);
#13752=AXIS2_PLACEMENT_3D('',#38632,#16427,#16428);
#13753=AXIS2_PLACEMENT_3D('',#38641,#16429,#16430);
#13754=AXIS2_PLACEMENT_3D('',#38643,#16431,#16432);
#13755=AXIS2_PLACEMENT_3D('',#38652,#16433,#16434);
#13756=AXIS2_PLACEMENT_3D('',#38660,#16435,#16436);
#13757=AXIS2_PLACEMENT_3D('',#38662,#16437,#16438);
#13758=AXIS2_PLACEMENT_3D('',#38663,#16439,#16440);
#13759=AXIS2_PLACEMENT_3D('',#38665,#16441,#16442);
#13760=AXIS2_PLACEMENT_3D('',#38667,#16443,#16444);
#13761=AXIS2_PLACEMENT_3D('',#38668,#16445,#16446);
#13762=AXIS2_PLACEMENT_3D('',#38777,#16447,#16448);
#13763=AXIS2_PLACEMENT_3D('',#38780,#16449,#16450);
#13764=AXIS2_PLACEMENT_3D('',#38782,#16451,#16452);
#13765=AXIS2_PLACEMENT_3D('',#38784,#16453,#16454);
#13766=AXIS2_PLACEMENT_3D('',#38794,#16455,#16456);
#13767=AXIS2_PLACEMENT_3D('',#38803,#16457,#16458);
#13768=AXIS2_PLACEMENT_3D('',#38805,#16459,#16460);
#13769=AXIS2_PLACEMENT_3D('',#38814,#16461,#16462);
#13770=AXIS2_PLACEMENT_3D('',#38822,#16463,#16464);
#13771=AXIS2_PLACEMENT_3D('',#38824,#16465,#16466);
#13772=AXIS2_PLACEMENT_3D('',#38825,#16467,#16468);
#13773=AXIS2_PLACEMENT_3D('',#38827,#16469,#16470);
#13774=AXIS2_PLACEMENT_3D('',#38829,#16471,#16472);
#13775=AXIS2_PLACEMENT_3D('',#38830,#16473,#16474);
#13776=AXIS2_PLACEMENT_3D('',#38939,#16475,#16476);
#13777=AXIS2_PLACEMENT_3D('',#38942,#16477,#16478);
#13778=AXIS2_PLACEMENT_3D('',#38944,#16479,#16480);
#13779=AXIS2_PLACEMENT_3D('',#38946,#16481,#16482);
#13780=AXIS2_PLACEMENT_3D('',#38956,#16483,#16484);
#13781=AXIS2_PLACEMENT_3D('',#38965,#16485,#16486);
#13782=AXIS2_PLACEMENT_3D('',#38967,#16487,#16488);
#13783=AXIS2_PLACEMENT_3D('',#38976,#16489,#16490);
#13784=AXIS2_PLACEMENT_3D('',#38984,#16491,#16492);
#13785=AXIS2_PLACEMENT_3D('',#38986,#16493,#16494);
#13786=AXIS2_PLACEMENT_3D('',#38987,#16495,#16496);
#13787=AXIS2_PLACEMENT_3D('',#38989,#16497,#16498);
#13788=AXIS2_PLACEMENT_3D('',#38991,#16499,#16500);
#13789=AXIS2_PLACEMENT_3D('',#38992,#16501,#16502);
#13790=AXIS2_PLACEMENT_3D('',#39101,#16503,#16504);
#13791=AXIS2_PLACEMENT_3D('',#39104,#16505,#16506);
#13792=AXIS2_PLACEMENT_3D('',#39113,#16507,#16508);
#13793=AXIS2_PLACEMENT_3D('',#39121,#16509,#16510);
#13794=AXIS2_PLACEMENT_3D('',#39123,#16511,#16512);
#13795=AXIS2_PLACEMENT_3D('',#39125,#16513,#16514);
#13796=AXIS2_PLACEMENT_3D('',#39135,#16515,#16516);
#13797=AXIS2_PLACEMENT_3D('',#39144,#16517,#16518);
#13798=AXIS2_PLACEMENT_3D('',#39146,#16519,#16520);
#13799=AXIS2_PLACEMENT_3D('',#39148,#16521,#16522);
#13800=AXIS2_PLACEMENT_3D('',#39149,#16523,#16524);
#13801=AXIS2_PLACEMENT_3D('',#39152,#16525,#16526);
#13802=AXIS2_PLACEMENT_3D('',#39154,#16527,#16528);
#13803=AXIS2_PLACEMENT_3D('',#39156,#16529,#16530);
#13804=AXIS2_PLACEMENT_3D('',#39166,#16531,#16532);
#13805=AXIS2_PLACEMENT_3D('',#39175,#16533,#16534);
#13806=AXIS2_PLACEMENT_3D('',#39177,#16535,#16536);
#13807=AXIS2_PLACEMENT_3D('',#39186,#16537,#16538);
#13808=AXIS2_PLACEMENT_3D('',#39194,#16539,#16540);
#13809=AXIS2_PLACEMENT_3D('',#39196,#16541,#16542);
#13810=AXIS2_PLACEMENT_3D('',#39197,#16543,#16544);
#13811=AXIS2_PLACEMENT_3D('',#39199,#16545,#16546);
#13812=AXIS2_PLACEMENT_3D('',#39201,#16547,#16548);
#13813=AXIS2_PLACEMENT_3D('',#39202,#16549,#16550);
#13814=AXIS2_PLACEMENT_3D('',#39311,#16551,#16552);
#13815=AXIS2_PLACEMENT_3D('',#39312,#16553,#16554);
#13816=AXIS2_PLACEMENT_3D('',#39313,#16555,#16556);
#13817=AXIS2_PLACEMENT_3D('',#39314,#16557,#16558);
#13818=AXIS2_PLACEMENT_3D('',#39315,#16559,#16560);
#13819=AXIS2_PLACEMENT_3D('',#39316,#16561,#16562);
#13820=AXIS2_PLACEMENT_3D('',#39317,#16563,#16564);
#13821=AXIS2_PLACEMENT_3D('',#39318,#16565,#16566);
#13822=AXIS2_PLACEMENT_3D('',#39319,#16567,#16568);
#13823=AXIS2_PLACEMENT_3D('',#39320,#16569,#16570);
#13824=AXIS2_PLACEMENT_3D('',#39321,#16571,#16572);
#13825=AXIS2_PLACEMENT_3D('',#39322,#16573,#16574);
#13826=AXIS2_PLACEMENT_3D('',#39323,#16575,#16576);
#13827=AXIS2_PLACEMENT_3D('',#39324,#16577,#16578);
#13828=AXIS2_PLACEMENT_3D('',#39325,#16579,#16580);
#13829=AXIS2_PLACEMENT_3D('',#39326,#16581,#16582);
#13830=AXIS2_PLACEMENT_3D('',#39327,#16583,#16584);
#13831=AXIS2_PLACEMENT_3D('',#39328,#16585,#16586);
#13832=AXIS2_PLACEMENT_3D('',#39329,#16587,#16588);
#13833=AXIS2_PLACEMENT_3D('',#39330,#16589,#16590);
#13834=AXIS2_PLACEMENT_3D('',#39331,#16591,#16592);
#13835=AXIS2_PLACEMENT_3D('',#39332,#16593,#16594);
#13836=AXIS2_PLACEMENT_3D('',#39333,#16595,#16596);
#13837=AXIS2_PLACEMENT_3D('',#39334,#16597,#16598);
#13838=AXIS2_PLACEMENT_3D('',#39335,#16599,#16600);
#13839=AXIS2_PLACEMENT_3D('',#39336,#16601,#16602);
#13840=AXIS2_PLACEMENT_3D('',#39337,#16603,#16604);
#13841=AXIS2_PLACEMENT_3D('',#39338,#16605,#16606);
#13842=AXIS2_PLACEMENT_3D('',#39339,#16607,#16608);
#13843=AXIS2_PLACEMENT_3D('',#39340,#16609,#16610);
#13844=AXIS2_PLACEMENT_3D('',#39341,#16611,#16612);
#13845=AXIS2_PLACEMENT_3D('',#39342,#16613,#16614);
#13846=AXIS2_PLACEMENT_3D('',#39343,#16615,#16616);
#13847=AXIS2_PLACEMENT_3D('',#39344,#16617,#16618);
#13848=AXIS2_PLACEMENT_3D('',#39345,#16619,#16620);
#13849=AXIS2_PLACEMENT_3D('',#39346,#16621,#16622);
#13850=AXIS2_PLACEMENT_3D('',#39347,#16623,#16624);
#13851=AXIS2_PLACEMENT_3D('',#39348,#16625,#16626);
#13852=AXIS2_PLACEMENT_3D('',#39349,#16627,#16628);
#13853=AXIS2_PLACEMENT_3D('',#39350,#16629,#16630);
#13854=AXIS2_PLACEMENT_3D('',#39351,#16631,#16632);
#13855=AXIS2_PLACEMENT_3D('',#39352,#16633,#16634);
#13856=AXIS2_PLACEMENT_3D('',#39353,#16635,#16636);
#13857=AXIS2_PLACEMENT_3D('',#39354,#16637,#16638);
#13858=AXIS2_PLACEMENT_3D('',#39355,#16639,#16640);
#13859=AXIS2_PLACEMENT_3D('',#39356,#16641,#16642);
#13860=AXIS2_PLACEMENT_3D('',#39357,#16643,#16644);
#13861=AXIS2_PLACEMENT_3D('',#39358,#16645,#16646);
#13862=AXIS2_PLACEMENT_3D('',#39359,#16647,#16648);
#13863=AXIS2_PLACEMENT_3D('',#39360,#16649,#16650);
#13864=AXIS2_PLACEMENT_3D('',#39361,#16651,#16652);
#13865=AXIS2_PLACEMENT_3D('',#39362,#16653,#16654);
#13866=AXIS2_PLACEMENT_3D('',#39363,#16655,#16656);
#13867=AXIS2_PLACEMENT_3D('',#39364,#16657,#16658);
#13868=AXIS2_PLACEMENT_3D('',#39365,#16659,#16660);
#13869=AXIS2_PLACEMENT_3D('',#39366,#16661,#16662);
#13870=AXIS2_PLACEMENT_3D('',#39367,#16663,#16664);
#13871=AXIS2_PLACEMENT_3D('',#39368,#16665,#16666);
#13872=AXIS2_PLACEMENT_3D('',#39369,#16667,#16668);
#13873=AXIS2_PLACEMENT_3D('',#39370,#16669,#16670);
#13874=AXIS2_PLACEMENT_3D('',#39371,#16671,#16672);
#13875=AXIS2_PLACEMENT_3D('',#39372,#16673,#16674);
#13876=AXIS2_PLACEMENT_3D('',#39373,#16675,#16676);
#13877=AXIS2_PLACEMENT_3D('',#39374,#16677,#16678);
#13878=AXIS2_PLACEMENT_3D('',#39375,#16679,#16680);
#13879=AXIS2_PLACEMENT_3D('',#39376,#16681,#16682);
#13880=AXIS2_PLACEMENT_3D('',#39377,#16683,#16684);
#13881=AXIS2_PLACEMENT_3D('',#39378,#16685,#16686);
#13882=AXIS2_PLACEMENT_3D('',#39379,#16687,#16688);
#13883=AXIS2_PLACEMENT_3D('',#39380,#16689,#16690);
#13884=AXIS2_PLACEMENT_3D('',#39381,#16691,#16692);
#13885=AXIS2_PLACEMENT_3D('',#39382,#16693,#16694);
#13886=AXIS2_PLACEMENT_3D('',#39383,#16695,#16696);
#13887=AXIS2_PLACEMENT_3D('',#39384,#16697,#16698);
#13888=AXIS2_PLACEMENT_3D('',#39385,#16699,#16700);
#13889=AXIS2_PLACEMENT_3D('',#39386,#16701,#16702);
#13890=AXIS2_PLACEMENT_3D('',#39387,#16703,#16704);
#13891=AXIS2_PLACEMENT_3D('',#39388,#16705,#16706);
#13892=AXIS2_PLACEMENT_3D('',#39389,#16707,#16708);
#13893=AXIS2_PLACEMENT_3D('',#39390,#16709,#16710);
#13894=AXIS2_PLACEMENT_3D('',#39391,#16711,#16712);
#13895=AXIS2_PLACEMENT_3D('',#39392,#16713,#16714);
#13896=AXIS2_PLACEMENT_3D('',#39393,#16715,#16716);
#13897=AXIS2_PLACEMENT_3D('',#39394,#16717,#16718);
#13898=AXIS2_PLACEMENT_3D('',#39395,#16719,#16720);
#13899=AXIS2_PLACEMENT_3D('',#39396,#16721,#16722);
#13900=AXIS2_PLACEMENT_3D('',#39397,#16723,#16724);
#13901=AXIS2_PLACEMENT_3D('',#39398,#16725,#16726);
#13902=AXIS2_PLACEMENT_3D('',#39399,#16727,#16728);
#13903=AXIS2_PLACEMENT_3D('',#39400,#16729,#16730);
#13904=AXIS2_PLACEMENT_3D('',#39401,#16731,#16732);
#13905=AXIS2_PLACEMENT_3D('',#39402,#16733,#16734);
#13906=AXIS2_PLACEMENT_3D('',#39403,#16735,#16736);
#13907=AXIS2_PLACEMENT_3D('',#39404,#16737,#16738);
#13908=AXIS2_PLACEMENT_3D('',#39405,#16739,#16740);
#13909=AXIS2_PLACEMENT_3D('',#39406,#16741,#16742);
#13910=AXIS2_PLACEMENT_3D('',#39407,#16743,#16744);
#13911=AXIS2_PLACEMENT_3D('',#39408,#16745,#16746);
#13912=AXIS2_PLACEMENT_3D('',#39409,#16747,#16748);
#13913=AXIS2_PLACEMENT_3D('',#39410,#16749,#16750);
#13914=AXIS2_PLACEMENT_3D('',#39411,#16751,#16752);
#13915=AXIS2_PLACEMENT_3D('',#39412,#16753,#16754);
#13916=AXIS2_PLACEMENT_3D('',#39413,#16755,#16756);
#13917=AXIS2_PLACEMENT_3D('',#39414,#16757,#16758);
#13918=AXIS2_PLACEMENT_3D('',#39415,#16759,#16760);
#13919=AXIS2_PLACEMENT_3D('',#39416,#16761,#16762);
#13920=AXIS2_PLACEMENT_3D('',#39417,#16763,#16764);
#13921=AXIS2_PLACEMENT_3D('',#39418,#16765,#16766);
#13922=AXIS2_PLACEMENT_3D('',#39419,#16767,#16768);
#13923=AXIS2_PLACEMENT_3D('',#39420,#16769,#16770);
#13924=AXIS2_PLACEMENT_3D('',#39421,#16771,#16772);
#13925=AXIS2_PLACEMENT_3D('',#39422,#16773,#16774);
#13926=AXIS2_PLACEMENT_3D('',#39423,#16775,#16776);
#13927=AXIS2_PLACEMENT_3D('',#39424,#16777,#16778);
#13928=AXIS2_PLACEMENT_3D('',#39425,#16779,#16780);
#13929=AXIS2_PLACEMENT_3D('',#39426,#16781,#16782);
#13930=AXIS2_PLACEMENT_3D('',#39427,#16783,#16784);
#13931=AXIS2_PLACEMENT_3D('',#39428,#16785,#16786);
#13932=AXIS2_PLACEMENT_3D('',#39429,#16787,#16788);
#13933=AXIS2_PLACEMENT_3D('',#39430,#16789,#16790);
#13934=AXIS2_PLACEMENT_3D('',#39431,#16791,#16792);
#13935=AXIS2_PLACEMENT_3D('',#39432,#16793,#16794);
#13936=AXIS2_PLACEMENT_3D('',#39433,#16795,#16796);
#13937=AXIS2_PLACEMENT_3D('',#39434,#16797,#16798);
#13938=AXIS2_PLACEMENT_3D('',#39435,#16799,#16800);
#13939=AXIS2_PLACEMENT_3D('',#39436,#16801,#16802);
#13940=AXIS2_PLACEMENT_3D('',#39437,#16803,#16804);
#13941=AXIS2_PLACEMENT_3D('',#39438,#16805,#16806);
#13942=AXIS2_PLACEMENT_3D('',#39440,#16807,#16808);
#13943=AXIS2_PLACEMENT_3D('',#39442,#16809,#16810);
#13944=AXIS2_PLACEMENT_3D('',#39443,#16811,#16812);
#13945=AXIS2_PLACEMENT_3D('',#39444,#16813,#16814);
#13946=AXIS2_PLACEMENT_3D('',#39447,#16815,#16816);
#13947=AXIS2_PLACEMENT_3D('',#39448,#16817,#16818);
#13948=AXIS2_PLACEMENT_3D('',#39450,#16819,#16820);
#13949=AXIS2_PLACEMENT_3D('',#39452,#16821,#16822);
#13950=AXIS2_PLACEMENT_3D('',#39453,#16823,#16824);
#13951=AXIS2_PLACEMENT_3D('',#39454,#16825,#16826);
#13952=AXIS2_PLACEMENT_3D('',#39457,#16827,#16828);
#13953=AXIS2_PLACEMENT_3D('',#39458,#16829,#16830);
#13954=AXIS2_PLACEMENT_3D('',#39460,#16831,#16832);
#13955=AXIS2_PLACEMENT_3D('',#39461,#16833,#16834);
#13956=AXIS2_PLACEMENT_3D('',#39462,#16835,#16836);
#13957=AXIS2_PLACEMENT_3D('',#39465,#16838,#16839);
#13958=AXIS2_PLACEMENT_3D('',#39466,#16840,#16841);
#13959=AXIS2_PLACEMENT_3D('',#39468,#16843,#16844);
#13960=AXIS2_PLACEMENT_3D('',#39471,#16846,#16847);
#13961=AXIS2_PLACEMENT_3D('',#39472,#16848,#16849);
#13962=AXIS2_PLACEMENT_3D('',#39475,#16851,#16852);
#13963=AXIS2_PLACEMENT_3D('',#39476,#16853,#16854);
#13964=AXIS2_PLACEMENT_3D('',#39478,#16855,#16856);
#13965=AXIS2_PLACEMENT_3D('',#39480,#16858,#16859);
#13966=AXIS2_PLACEMENT_3D('',#39481,#16860,#16861);
#13967=AXIS2_PLACEMENT_3D('',#39482,#16862,#16863);
#13968=AXIS2_PLACEMENT_3D('',#39485,#16864,#16865);
#13969=AXIS2_PLACEMENT_3D('',#39486,#16866,#16867);
#13970=AXIS2_PLACEMENT_3D('',#39489,#16868,#16869);
#13971=AXIS2_PLACEMENT_3D('',#39490,#16870,#16871);
#13972=AXIS2_PLACEMENT_3D('',#39493,#16872,#16873);
#13973=AXIS2_PLACEMENT_3D('',#39494,#16874,#16875);
#13974=AXIS2_PLACEMENT_3D('',#39497,#16876,#16877);
#13975=AXIS2_PLACEMENT_3D('',#39498,#16878,#16879);
#13976=AXIS2_PLACEMENT_3D('',#39501,#16880,#16881);
#13977=AXIS2_PLACEMENT_3D('',#39502,#16882,#16883);
#13978=AXIS2_PLACEMENT_3D('',#39505,#16884,#16885);
#13979=AXIS2_PLACEMENT_3D('',#39506,#16886,#16887);
#13980=AXIS2_PLACEMENT_3D('',#39509,#16888,#16889);
#13981=AXIS2_PLACEMENT_3D('',#39510,#16890,#16891);
#13982=AXIS2_PLACEMENT_3D('',#39512,#16892,#16893);
#13983=AXIS2_PLACEMENT_3D('',#39514,#16894,#16895);
#13984=AXIS2_PLACEMENT_3D('',#39516,#16896,#16897);
#13985=AXIS2_PLACEMENT_3D('',#39517,#16898,#16899);
#13986=AXIS2_PLACEMENT_3D('',#39518,#16900,#16901);
#13987=AXIS2_PLACEMENT_3D('',#39520,#16902,#16903);
#13988=AXIS2_PLACEMENT_3D('',#39522,#16904,#16905);
#13989=AXIS2_PLACEMENT_3D('',#39523,#16906,#16907);
#13990=AXIS2_PLACEMENT_3D('',#39524,#16908,#16909);
#13991=AXIS2_PLACEMENT_3D('',#39526,#16910,#16911);
#13992=AXIS2_PLACEMENT_3D('',#39528,#16912,#16913);
#13993=AXIS2_PLACEMENT_3D('',#39529,#16914,#16915);
#13994=AXIS2_PLACEMENT_3D('',#39530,#16916,#16917);
#13995=AXIS2_PLACEMENT_3D('',#39533,#16918,#16919);
#13996=AXIS2_PLACEMENT_3D('',#39534,#16920,#16921);
#13997=AXIS2_PLACEMENT_3D('',#39536,#16922,#16923);
#13998=AXIS2_PLACEMENT_3D('',#39537,#16924,#16925);
#13999=AXIS2_PLACEMENT_3D('',#39538,#16926,#16927);
#14000=AXIS2_PLACEMENT_3D('',#39540,#16928,#16929);
#14001=AXIS2_PLACEMENT_3D('',#39543,#16931,#16932);
#14002=AXIS2_PLACEMENT_3D('',#39544,#16933,#16934);
#14003=AXIS2_PLACEMENT_3D('',#39546,#16935,#16936);
#14004=AXIS2_PLACEMENT_3D('',#39548,#16938,#16939);
#14005=AXIS2_PLACEMENT_3D('',#39551,#16941,#16942);
#14006=AXIS2_PLACEMENT_3D('',#39552,#16943,#16944);
#14007=AXIS2_PLACEMENT_3D('',#39554,#16945,#16946);
#14008=AXIS2_PLACEMENT_3D('',#39555,#16947,#16948);
#14009=AXIS2_PLACEMENT_3D('',#39556,#16949,#16950);
#14010=AXIS2_PLACEMENT_3D('',#39558,#16952,#16953);
#14011=AXIS2_PLACEMENT_3D('',#39561,#16955,#16956);
#14012=AXIS2_PLACEMENT_3D('',#39562,#16957,#16958);
#14013=AXIS2_PLACEMENT_3D('',#39564,#16959,#16960);
#14014=AXIS2_PLACEMENT_3D('',#39567,#16962,#16963);
#14015=AXIS2_PLACEMENT_3D('',#39568,#16964,#16965);
#14016=AXIS2_PLACEMENT_3D('',#39570,#16966,#16967);
#14017=AXIS2_PLACEMENT_3D('',#39573,#16969,#16970);
#14018=AXIS2_PLACEMENT_3D('',#39574,#16971,#16972);
#14019=AXIS2_PLACEMENT_3D('',#39577,#16973,#16974);
#14020=AXIS2_PLACEMENT_3D('',#39580,#16976,#16977);
#14021=AXIS2_PLACEMENT_3D('',#39581,#16978,#16979);
#14022=AXIS2_PLACEMENT_3D('',#39582,#16980,#16981);
#14023=AXIS2_PLACEMENT_3D('',#39584,#16983,#16984);
#14024=AXIS2_PLACEMENT_3D('',#39585,#16985,#16986);
#14025=AXIS2_PLACEMENT_3D('',#39586,#16987,#16988);
#14026=AXIS2_PLACEMENT_3D('',#39587,#16989,#16990);
#14027=AXIS2_PLACEMENT_3D('',#39588,#16991,#16992);
#14028=AXIS2_PLACEMENT_3D('',#39589,#16993,#16994);
#14029=AXIS2_PLACEMENT_3D('',#39590,#16995,#16996);
#14030=AXIS2_PLACEMENT_3D('',#39592,#16997,#16998);
#14031=AXIS2_PLACEMENT_3D('',#39594,#16999,#17000);
#14032=AXIS2_PLACEMENT_3D('',#39595,#17001,#17002);
#14033=AXIS2_PLACEMENT_3D('',#39704,#17003,#17004);
#14034=AXIS2_PLACEMENT_3D('',#39707,#17005,#17006);
#14035=AXIS2_PLACEMENT_3D('',#39709,#17007,#17008);
#14036=AXIS2_PLACEMENT_3D('',#39711,#17009,#17010);
#14037=AXIS2_PLACEMENT_3D('',#39721,#17011,#17012);
#14038=AXIS2_PLACEMENT_3D('',#39730,#17013,#17014);
#14039=AXIS2_PLACEMENT_3D('',#39732,#17015,#17016);
#14040=AXIS2_PLACEMENT_3D('',#39741,#17017,#17018);
#14041=AXIS2_PLACEMENT_3D('',#39749,#17019,#17020);
#14042=AXIS2_PLACEMENT_3D('',#39751,#17021,#17022);
#14043=AXIS2_PLACEMENT_3D('',#39752,#17023,#17024);
#14044=AXIS2_PLACEMENT_3D('',#39754,#17025,#17026);
#14045=AXIS2_PLACEMENT_3D('',#39756,#17027,#17028);
#14046=AXIS2_PLACEMENT_3D('',#39757,#17029,#17030);
#14047=AXIS2_PLACEMENT_3D('',#39866,#17031,#17032);
#14048=AXIS2_PLACEMENT_3D('',#39869,#17033,#17034);
#14049=AXIS2_PLACEMENT_3D('',#39871,#17035,#17036);
#14050=AXIS2_PLACEMENT_3D('',#39873,#17037,#17038);
#14051=AXIS2_PLACEMENT_3D('',#39883,#17039,#17040);
#14052=AXIS2_PLACEMENT_3D('',#39892,#17041,#17042);
#14053=AXIS2_PLACEMENT_3D('',#39894,#17043,#17044);
#14054=AXIS2_PLACEMENT_3D('',#39903,#17045,#17046);
#14055=AXIS2_PLACEMENT_3D('',#39911,#17047,#17048);
#14056=AXIS2_PLACEMENT_3D('',#39913,#17049,#17050);
#14057=AXIS2_PLACEMENT_3D('',#39914,#17051,#17052);
#14058=AXIS2_PLACEMENT_3D('',#39916,#17053,#17054);
#14059=AXIS2_PLACEMENT_3D('',#39918,#17055,#17056);
#14060=AXIS2_PLACEMENT_3D('',#39919,#17057,#17058);
#14061=AXIS2_PLACEMENT_3D('',#40028,#17059,#17060);
#14062=AXIS2_PLACEMENT_3D('',#40031,#17061,#17062);
#14063=AXIS2_PLACEMENT_3D('',#40033,#17063,#17064);
#14064=AXIS2_PLACEMENT_3D('',#40035,#17065,#17066);
#14065=AXIS2_PLACEMENT_3D('',#40045,#17067,#17068);
#14066=AXIS2_PLACEMENT_3D('',#40054,#17069,#17070);
#14067=AXIS2_PLACEMENT_3D('',#40056,#17071,#17072);
#14068=AXIS2_PLACEMENT_3D('',#40065,#17073,#17074);
#14069=AXIS2_PLACEMENT_3D('',#40073,#17075,#17076);
#14070=AXIS2_PLACEMENT_3D('',#40075,#17077,#17078);
#14071=AXIS2_PLACEMENT_3D('',#40076,#17079,#17080);
#14072=AXIS2_PLACEMENT_3D('',#40078,#17081,#17082);
#14073=AXIS2_PLACEMENT_3D('',#40080,#17083,#17084);
#14074=AXIS2_PLACEMENT_3D('',#40081,#17085,#17086);
#14075=AXIS2_PLACEMENT_3D('',#40190,#17087,#17088);
#14076=AXIS2_PLACEMENT_3D('',#40193,#17089,#17090);
#14077=AXIS2_PLACEMENT_3D('',#40195,#17091,#17092);
#14078=AXIS2_PLACEMENT_3D('',#40197,#17093,#17094);
#14079=AXIS2_PLACEMENT_3D('',#40207,#17095,#17096);
#14080=AXIS2_PLACEMENT_3D('',#40216,#17097,#17098);
#14081=AXIS2_PLACEMENT_3D('',#40218,#17099,#17100);
#14082=AXIS2_PLACEMENT_3D('',#40227,#17101,#17102);
#14083=AXIS2_PLACEMENT_3D('',#40235,#17103,#17104);
#14084=AXIS2_PLACEMENT_3D('',#40237,#17105,#17106);
#14085=AXIS2_PLACEMENT_3D('',#40238,#17107,#17108);
#14086=AXIS2_PLACEMENT_3D('',#40240,#17109,#17110);
#14087=AXIS2_PLACEMENT_3D('',#40242,#17111,#17112);
#14088=AXIS2_PLACEMENT_3D('',#40243,#17113,#17114);
#14089=AXIS2_PLACEMENT_3D('',#40352,#17115,#17116);
#14090=AXIS2_PLACEMENT_3D('',#40355,#17117,#17118);
#14091=AXIS2_PLACEMENT_3D('',#40357,#17119,#17120);
#14092=AXIS2_PLACEMENT_3D('',#40359,#17121,#17122);
#14093=AXIS2_PLACEMENT_3D('',#40369,#17123,#17124);
#14094=AXIS2_PLACEMENT_3D('',#40378,#17125,#17126);
#14095=AXIS2_PLACEMENT_3D('',#40380,#17127,#17128);
#14096=AXIS2_PLACEMENT_3D('',#40389,#17129,#17130);
#14097=AXIS2_PLACEMENT_3D('',#40397,#17131,#17132);
#14098=AXIS2_PLACEMENT_3D('',#40399,#17133,#17134);
#14099=AXIS2_PLACEMENT_3D('',#40400,#17135,#17136);
#14100=AXIS2_PLACEMENT_3D('',#40402,#17137,#17138);
#14101=AXIS2_PLACEMENT_3D('',#40404,#17139,#17140);
#14102=AXIS2_PLACEMENT_3D('',#40405,#17141,#17142);
#14103=AXIS2_PLACEMENT_3D('',#40514,#17143,#17144);
#14104=AXIS2_PLACEMENT_3D('',#40517,#17145,#17146);
#14105=AXIS2_PLACEMENT_3D('',#40526,#17147,#17148);
#14106=AXIS2_PLACEMENT_3D('',#40534,#17149,#17150);
#14107=AXIS2_PLACEMENT_3D('',#40536,#17151,#17152);
#14108=AXIS2_PLACEMENT_3D('',#40538,#17153,#17154);
#14109=AXIS2_PLACEMENT_3D('',#40548,#17155,#17156);
#14110=AXIS2_PLACEMENT_3D('',#40557,#17157,#17158);
#14111=AXIS2_PLACEMENT_3D('',#40559,#17159,#17160);
#14112=AXIS2_PLACEMENT_3D('',#40561,#17161,#17162);
#14113=AXIS2_PLACEMENT_3D('',#40562,#17163,#17164);
#14114=AXIS2_PLACEMENT_3D('',#40565,#17165,#17166);
#14115=AXIS2_PLACEMENT_3D('',#40567,#17167,#17168);
#14116=AXIS2_PLACEMENT_3D('',#40569,#17169,#17170);
#14117=AXIS2_PLACEMENT_3D('',#40579,#17171,#17172);
#14118=AXIS2_PLACEMENT_3D('',#40588,#17173,#17174);
#14119=AXIS2_PLACEMENT_3D('',#40590,#17175,#17176);
#14120=AXIS2_PLACEMENT_3D('',#40599,#17177,#17178);
#14121=AXIS2_PLACEMENT_3D('',#40607,#17179,#17180);
#14122=AXIS2_PLACEMENT_3D('',#40609,#17181,#17182);
#14123=AXIS2_PLACEMENT_3D('',#40610,#17183,#17184);
#14124=AXIS2_PLACEMENT_3D('',#40612,#17185,#17186);
#14125=AXIS2_PLACEMENT_3D('',#40614,#17187,#17188);
#14126=AXIS2_PLACEMENT_3D('',#40615,#17189,#17190);
#14127=AXIS2_PLACEMENT_3D('',#40724,#17191,#17192);
#14128=AXIS2_PLACEMENT_3D('',#40725,#17193,#17194);
#14129=AXIS2_PLACEMENT_3D('',#40726,#17195,#17196);
#14130=AXIS2_PLACEMENT_3D('',#40727,#17197,#17198);
#14131=AXIS2_PLACEMENT_3D('',#40728,#17199,#17200);
#14132=AXIS2_PLACEMENT_3D('',#40729,#17201,#17202);
#14133=AXIS2_PLACEMENT_3D('',#40730,#17203,#17204);
#14134=AXIS2_PLACEMENT_3D('',#40731,#17205,#17206);
#14135=AXIS2_PLACEMENT_3D('',#40732,#17207,#17208);
#14136=AXIS2_PLACEMENT_3D('',#40733,#17209,#17210);
#14137=AXIS2_PLACEMENT_3D('',#40734,#17211,#17212);
#14138=AXIS2_PLACEMENT_3D('',#40735,#17213,#17214);
#14139=AXIS2_PLACEMENT_3D('',#40736,#17215,#17216);
#14140=AXIS2_PLACEMENT_3D('',#40737,#17217,#17218);
#14141=AXIS2_PLACEMENT_3D('',#40738,#17219,#17220);
#14142=AXIS2_PLACEMENT_3D('',#40739,#17221,#17222);
#14143=AXIS2_PLACEMENT_3D('',#40740,#17223,#17224);
#14144=AXIS2_PLACEMENT_3D('',#40741,#17225,#17226);
#14145=AXIS2_PLACEMENT_3D('',#40742,#17227,#17228);
#14146=AXIS2_PLACEMENT_3D('',#40743,#17229,#17230);
#14147=AXIS2_PLACEMENT_3D('',#40744,#17231,#17232);
#14148=AXIS2_PLACEMENT_3D('',#40745,#17233,#17234);
#14149=AXIS2_PLACEMENT_3D('',#40746,#17235,#17236);
#14150=AXIS2_PLACEMENT_3D('',#40747,#17237,#17238);
#14151=AXIS2_PLACEMENT_3D('',#40748,#17239,#17240);
#14152=AXIS2_PLACEMENT_3D('',#40749,#17241,#17242);
#14153=AXIS2_PLACEMENT_3D('',#40750,#17243,#17244);
#14154=AXIS2_PLACEMENT_3D('',#40751,#17245,#17246);
#14155=AXIS2_PLACEMENT_3D('',#40752,#17247,#17248);
#14156=AXIS2_PLACEMENT_3D('',#40753,#17249,#17250);
#14157=AXIS2_PLACEMENT_3D('',#40754,#17251,#17252);
#14158=AXIS2_PLACEMENT_3D('',#40755,#17253,#17254);
#14159=AXIS2_PLACEMENT_3D('',#40756,#17255,#17256);
#14160=AXIS2_PLACEMENT_3D('',#40757,#17257,#17258);
#14161=AXIS2_PLACEMENT_3D('',#40758,#17259,#17260);
#14162=AXIS2_PLACEMENT_3D('',#40759,#17261,#17262);
#14163=AXIS2_PLACEMENT_3D('',#40760,#17263,#17264);
#14164=AXIS2_PLACEMENT_3D('',#40761,#17265,#17266);
#14165=AXIS2_PLACEMENT_3D('',#40762,#17267,#17268);
#14166=AXIS2_PLACEMENT_3D('',#40763,#17269,#17270);
#14167=AXIS2_PLACEMENT_3D('',#40764,#17271,#17272);
#14168=AXIS2_PLACEMENT_3D('',#40765,#17273,#17274);
#14169=AXIS2_PLACEMENT_3D('',#40766,#17275,#17276);
#14170=AXIS2_PLACEMENT_3D('',#40767,#17277,#17278);
#14171=AXIS2_PLACEMENT_3D('',#40768,#17279,#17280);
#14172=AXIS2_PLACEMENT_3D('',#40769,#17281,#17282);
#14173=AXIS2_PLACEMENT_3D('',#40770,#17283,#17284);
#14174=AXIS2_PLACEMENT_3D('',#40771,#17285,#17286);
#14175=AXIS2_PLACEMENT_3D('',#40772,#17287,#17288);
#14176=AXIS2_PLACEMENT_3D('',#40773,#17289,#17290);
#14177=AXIS2_PLACEMENT_3D('',#40774,#17291,#17292);
#14178=AXIS2_PLACEMENT_3D('',#40775,#17293,#17294);
#14179=AXIS2_PLACEMENT_3D('',#40776,#17295,#17296);
#14180=AXIS2_PLACEMENT_3D('',#40777,#17297,#17298);
#14181=AXIS2_PLACEMENT_3D('',#40778,#17299,#17300);
#14182=AXIS2_PLACEMENT_3D('',#40779,#17301,#17302);
#14183=AXIS2_PLACEMENT_3D('',#40780,#17303,#17304);
#14184=AXIS2_PLACEMENT_3D('',#40781,#17305,#17306);
#14185=AXIS2_PLACEMENT_3D('',#40782,#17307,#17308);
#14186=AXIS2_PLACEMENT_3D('',#40783,#17309,#17310);
#14187=AXIS2_PLACEMENT_3D('',#40784,#17311,#17312);
#14188=AXIS2_PLACEMENT_3D('',#40785,#17313,#17314);
#14189=AXIS2_PLACEMENT_3D('',#40786,#17315,#17316);
#14190=AXIS2_PLACEMENT_3D('',#40787,#17317,#17318);
#14191=AXIS2_PLACEMENT_3D('',#40788,#17319,#17320);
#14192=AXIS2_PLACEMENT_3D('',#40789,#17321,#17322);
#14193=AXIS2_PLACEMENT_3D('',#40790,#17323,#17324);
#14194=AXIS2_PLACEMENT_3D('',#40791,#17325,#17326);
#14195=AXIS2_PLACEMENT_3D('',#40792,#17327,#17328);
#14196=AXIS2_PLACEMENT_3D('',#40793,#17329,#17330);
#14197=AXIS2_PLACEMENT_3D('',#40794,#17331,#17332);
#14198=AXIS2_PLACEMENT_3D('',#40795,#17333,#17334);
#14199=AXIS2_PLACEMENT_3D('',#40796,#17335,#17336);
#14200=AXIS2_PLACEMENT_3D('',#40797,#17337,#17338);
#14201=AXIS2_PLACEMENT_3D('',#40798,#17339,#17340);
#14202=AXIS2_PLACEMENT_3D('',#40799,#17341,#17342);
#14203=AXIS2_PLACEMENT_3D('',#40800,#17343,#17344);
#14204=AXIS2_PLACEMENT_3D('',#40801,#17345,#17346);
#14205=AXIS2_PLACEMENT_3D('',#40802,#17347,#17348);
#14206=AXIS2_PLACEMENT_3D('',#40803,#17349,#17350);
#14207=AXIS2_PLACEMENT_3D('',#40804,#17351,#17352);
#14208=AXIS2_PLACEMENT_3D('',#40805,#17353,#17354);
#14209=AXIS2_PLACEMENT_3D('',#40806,#17355,#17356);
#14210=AXIS2_PLACEMENT_3D('',#40807,#17357,#17358);
#14211=AXIS2_PLACEMENT_3D('',#40808,#17359,#17360);
#14212=AXIS2_PLACEMENT_3D('',#40809,#17361,#17362);
#14213=AXIS2_PLACEMENT_3D('',#40810,#17363,#17364);
#14214=AXIS2_PLACEMENT_3D('',#40811,#17365,#17366);
#14215=AXIS2_PLACEMENT_3D('',#40812,#17367,#17368);
#14216=AXIS2_PLACEMENT_3D('',#40813,#17369,#17370);
#14217=AXIS2_PLACEMENT_3D('',#40814,#17371,#17372);
#14218=AXIS2_PLACEMENT_3D('',#40815,#17373,#17374);
#14219=AXIS2_PLACEMENT_3D('',#40816,#17375,#17376);
#14220=AXIS2_PLACEMENT_3D('',#40817,#17377,#17378);
#14221=AXIS2_PLACEMENT_3D('',#40818,#17379,#17380);
#14222=AXIS2_PLACEMENT_3D('',#40819,#17381,#17382);
#14223=AXIS2_PLACEMENT_3D('',#40820,#17383,#17384);
#14224=AXIS2_PLACEMENT_3D('',#40821,#17385,#17386);
#14225=AXIS2_PLACEMENT_3D('',#40822,#17387,#17388);
#14226=AXIS2_PLACEMENT_3D('',#40823,#17389,#17390);
#14227=AXIS2_PLACEMENT_3D('',#40824,#17391,#17392);
#14228=AXIS2_PLACEMENT_3D('',#40825,#17393,#17394);
#14229=AXIS2_PLACEMENT_3D('',#40826,#17395,#17396);
#14230=AXIS2_PLACEMENT_3D('',#40827,#17397,#17398);
#14231=AXIS2_PLACEMENT_3D('',#40828,#17399,#17400);
#14232=AXIS2_PLACEMENT_3D('',#40829,#17401,#17402);
#14233=AXIS2_PLACEMENT_3D('',#40830,#17403,#17404);
#14234=AXIS2_PLACEMENT_3D('',#40831,#17405,#17406);
#14235=AXIS2_PLACEMENT_3D('',#40832,#17407,#17408);
#14236=AXIS2_PLACEMENT_3D('',#40833,#17409,#17410);
#14237=AXIS2_PLACEMENT_3D('',#40834,#17411,#17412);
#14238=AXIS2_PLACEMENT_3D('',#40835,#17413,#17414);
#14239=AXIS2_PLACEMENT_3D('',#40836,#17415,#17416);
#14240=AXIS2_PLACEMENT_3D('',#40837,#17417,#17418);
#14241=AXIS2_PLACEMENT_3D('',#40838,#17419,#17420);
#14242=AXIS2_PLACEMENT_3D('',#40839,#17421,#17422);
#14243=AXIS2_PLACEMENT_3D('',#40840,#17423,#17424);
#14244=AXIS2_PLACEMENT_3D('',#40841,#17425,#17426);
#14245=AXIS2_PLACEMENT_3D('',#40842,#17427,#17428);
#14246=AXIS2_PLACEMENT_3D('',#40843,#17429,#17430);
#14247=AXIS2_PLACEMENT_3D('',#40844,#17431,#17432);
#14248=AXIS2_PLACEMENT_3D('',#40845,#17433,#17434);
#14249=AXIS2_PLACEMENT_3D('',#40846,#17435,#17436);
#14250=AXIS2_PLACEMENT_3D('',#40847,#17437,#17438);
#14251=AXIS2_PLACEMENT_3D('',#40848,#17439,#17440);
#14252=AXIS2_PLACEMENT_3D('',#40849,#17441,#17442);
#14253=AXIS2_PLACEMENT_3D('',#40850,#17443,#17444);
#14254=AXIS2_PLACEMENT_3D('',#40851,#17445,#17446);
#14255=AXIS2_PLACEMENT_3D('',#40853,#17447,#17448);
#14256=AXIS2_PLACEMENT_3D('',#40855,#17449,#17450);
#14257=AXIS2_PLACEMENT_3D('',#40856,#17451,#17452);
#14258=AXIS2_PLACEMENT_3D('',#40857,#17453,#17454);
#14259=AXIS2_PLACEMENT_3D('',#40860,#17455,#17456);
#14260=AXIS2_PLACEMENT_3D('',#40862,#17457,#17458);
#14261=AXIS2_PLACEMENT_3D('',#40864,#17459,#17460);
#14262=AXIS2_PLACEMENT_3D('',#40865,#17461,#17462);
#14263=AXIS2_PLACEMENT_3D('',#40866,#17463,#17464);
#14264=AXIS2_PLACEMENT_3D('',#40867,#17465,#17466);
#14265=AXIS2_PLACEMENT_3D('',#40870,#17467,#17468);
#14266=AXIS2_PLACEMENT_3D('',#40872,#17469,#17470);
#14267=AXIS2_PLACEMENT_3D('',#40873,#17471,#17472);
#14268=AXIS2_PLACEMENT_3D('',#40874,#17473,#17474);
#14269=AXIS2_PLACEMENT_3D('',#40875,#17475,#17476);
#14270=AXIS2_PLACEMENT_3D('',#40878,#17478,#17479);
#14271=AXIS2_PLACEMENT_3D('',#40879,#17480,#17481);
#14272=AXIS2_PLACEMENT_3D('',#40881,#17483,#17484);
#14273=AXIS2_PLACEMENT_3D('',#40884,#17486,#17487);
#14274=AXIS2_PLACEMENT_3D('',#40885,#17488,#17489);
#14275=AXIS2_PLACEMENT_3D('',#40887,#17490,#17491);
#14276=AXIS2_PLACEMENT_3D('',#40889,#17493,#17494);
#14277=AXIS2_PLACEMENT_3D('',#40892,#17496,#17497);
#14278=AXIS2_PLACEMENT_3D('',#40893,#17498,#17499);
#14279=AXIS2_PLACEMENT_3D('',#40894,#17500,#17501);
#14280=AXIS2_PLACEMENT_3D('',#40895,#17502,#17503);
#14281=AXIS2_PLACEMENT_3D('',#40898,#17504,#17505);
#14282=AXIS2_PLACEMENT_3D('',#40899,#17506,#17507);
#14283=AXIS2_PLACEMENT_3D('',#40902,#17508,#17509);
#14284=AXIS2_PLACEMENT_3D('',#40903,#17510,#17511);
#14285=AXIS2_PLACEMENT_3D('',#40906,#17512,#17513);
#14286=AXIS2_PLACEMENT_3D('',#40907,#17514,#17515);
#14287=AXIS2_PLACEMENT_3D('',#40910,#17516,#17517);
#14288=AXIS2_PLACEMENT_3D('',#40911,#17518,#17519);
#14289=AXIS2_PLACEMENT_3D('',#40914,#17520,#17521);
#14290=AXIS2_PLACEMENT_3D('',#40915,#17522,#17523);
#14291=AXIS2_PLACEMENT_3D('',#40918,#17524,#17525);
#14292=AXIS2_PLACEMENT_3D('',#40919,#17526,#17527);
#14293=AXIS2_PLACEMENT_3D('',#40922,#17528,#17529);
#14294=AXIS2_PLACEMENT_3D('',#40923,#17530,#17531);
#14295=AXIS2_PLACEMENT_3D('',#40925,#17532,#17533);
#14296=AXIS2_PLACEMENT_3D('',#40927,#17534,#17535);
#14297=AXIS2_PLACEMENT_3D('',#40929,#17536,#17537);
#14298=AXIS2_PLACEMENT_3D('',#40930,#17538,#17539);
#14299=AXIS2_PLACEMENT_3D('',#40931,#17540,#17541);
#14300=AXIS2_PLACEMENT_3D('',#40933,#17542,#17543);
#14301=AXIS2_PLACEMENT_3D('',#40935,#17544,#17545);
#14302=AXIS2_PLACEMENT_3D('',#40936,#17546,#17547);
#14303=AXIS2_PLACEMENT_3D('',#40937,#17548,#17549);
#14304=AXIS2_PLACEMENT_3D('',#40939,#17550,#17551);
#14305=AXIS2_PLACEMENT_3D('',#40941,#17552,#17553);
#14306=AXIS2_PLACEMENT_3D('',#40942,#17554,#17555);
#14307=AXIS2_PLACEMENT_3D('',#40943,#17556,#17557);
#14308=AXIS2_PLACEMENT_3D('',#40946,#17558,#17559);
#14309=AXIS2_PLACEMENT_3D('',#40948,#17560,#17561);
#14310=AXIS2_PLACEMENT_3D('',#40949,#17562,#17563);
#14311=AXIS2_PLACEMENT_3D('',#40950,#17564,#17565);
#14312=AXIS2_PLACEMENT_3D('',#40951,#17566,#17567);
#14313=AXIS2_PLACEMENT_3D('',#40953,#17568,#17569);
#14314=AXIS2_PLACEMENT_3D('',#40956,#17571,#17572);
#14315=AXIS2_PLACEMENT_3D('',#40957,#17573,#17574);
#14316=AXIS2_PLACEMENT_3D('',#40960,#17576,#17577);
#14317=AXIS2_PLACEMENT_3D('',#40961,#17578,#17579);
#14318=AXIS2_PLACEMENT_3D('',#40963,#17580,#17581);
#14319=AXIS2_PLACEMENT_3D('',#40965,#17583,#17584);
#14320=AXIS2_PLACEMENT_3D('',#40967,#17585,#17586);
#14321=AXIS2_PLACEMENT_3D('',#40968,#17587,#17588);
#14322=AXIS2_PLACEMENT_3D('',#40969,#17589,#17590);
#14323=AXIS2_PLACEMENT_3D('',#40971,#17592,#17593);
#14324=AXIS2_PLACEMENT_3D('',#40973,#17594,#17595);
#14325=AXIS2_PLACEMENT_3D('',#40975,#17597,#17598);
#14326=AXIS2_PLACEMENT_3D('',#40977,#17599,#17600);
#14327=AXIS2_PLACEMENT_3D('',#40980,#17602,#17603);
#14328=AXIS2_PLACEMENT_3D('',#40981,#17604,#17605);
#14329=AXIS2_PLACEMENT_3D('',#40983,#17606,#17607);
#14330=AXIS2_PLACEMENT_3D('',#40986,#17609,#17610);
#14331=AXIS2_PLACEMENT_3D('',#40987,#17611,#17612);
#14332=AXIS2_PLACEMENT_3D('',#40990,#17613,#17614);
#14333=AXIS2_PLACEMENT_3D('',#40991,#17615,#17616);
#14334=AXIS2_PLACEMENT_3D('',#40994,#17618,#17619);
#14335=AXIS2_PLACEMENT_3D('',#40995,#17620,#17621);
#14336=AXIS2_PLACEMENT_3D('',#40997,#17623,#17624);
#14337=AXIS2_PLACEMENT_3D('',#40998,#17625,#17626);
#14338=AXIS2_PLACEMENT_3D('',#40999,#17627,#17628);
#14339=AXIS2_PLACEMENT_3D('',#41000,#17629,#17630);
#14340=AXIS2_PLACEMENT_3D('',#41001,#17631,#17632);
#14341=AXIS2_PLACEMENT_3D('',#41002,#17633,#17634);
#14342=AXIS2_PLACEMENT_3D('',#41003,#17635,#17636);
#14343=AXIS2_PLACEMENT_3D('',#41005,#17637,#17638);
#14344=AXIS2_PLACEMENT_3D('',#41007,#17639,#17640);
#14345=AXIS2_PLACEMENT_3D('',#41008,#17641,#17642);
#14346=AXIS2_PLACEMENT_3D('',#41117,#17643,#17644);
#14347=AXIS2_PLACEMENT_3D('',#41120,#17645,#17646);
#14348=AXIS2_PLACEMENT_3D('',#41129,#17647,#17648);
#14349=AXIS2_PLACEMENT_3D('',#41137,#17649,#17650);
#14350=AXIS2_PLACEMENT_3D('',#41139,#17651,#17652);
#14351=AXIS2_PLACEMENT_3D('',#41141,#17653,#17654);
#14352=AXIS2_PLACEMENT_3D('',#41151,#17655,#17656);
#14353=AXIS2_PLACEMENT_3D('',#41160,#17657,#17658);
#14354=AXIS2_PLACEMENT_3D('',#41162,#17659,#17660);
#14355=AXIS2_PLACEMENT_3D('',#41164,#17661,#17662);
#14356=AXIS2_PLACEMENT_3D('',#41165,#17663,#17664);
#14357=AXIS2_PLACEMENT_3D('',#41167,#17665,#17666);
#14358=AXIS2_PLACEMENT_3D('',#41169,#17667,#17668);
#14359=AXIS2_PLACEMENT_3D('',#41170,#17669,#17670);
#14360=AXIS2_PLACEMENT_3D('',#41279,#17671,#17672);
#14361=AXIS2_PLACEMENT_3D('',#41282,#17673,#17674);
#14362=AXIS2_PLACEMENT_3D('',#41291,#17675,#17676);
#14363=AXIS2_PLACEMENT_3D('',#41299,#17677,#17678);
#14364=AXIS2_PLACEMENT_3D('',#41301,#17679,#17680);
#14365=AXIS2_PLACEMENT_3D('',#41303,#17681,#17682);
#14366=AXIS2_PLACEMENT_3D('',#41313,#17683,#17684);
#14367=AXIS2_PLACEMENT_3D('',#41322,#17685,#17686);
#14368=AXIS2_PLACEMENT_3D('',#41324,#17687,#17688);
#14369=AXIS2_PLACEMENT_3D('',#41326,#17689,#17690);
#14370=AXIS2_PLACEMENT_3D('',#41327,#17691,#17692);
#14371=AXIS2_PLACEMENT_3D('',#41329,#17693,#17694);
#14372=AXIS2_PLACEMENT_3D('',#41331,#17695,#17696);
#14373=AXIS2_PLACEMENT_3D('',#41332,#17697,#17698);
#14374=AXIS2_PLACEMENT_3D('',#41441,#17699,#17700);
#14375=AXIS2_PLACEMENT_3D('',#41444,#17701,#17702);
#14376=AXIS2_PLACEMENT_3D('',#41453,#17703,#17704);
#14377=AXIS2_PLACEMENT_3D('',#41461,#17705,#17706);
#14378=AXIS2_PLACEMENT_3D('',#41463,#17707,#17708);
#14379=AXIS2_PLACEMENT_3D('',#41465,#17709,#17710);
#14380=AXIS2_PLACEMENT_3D('',#41475,#17711,#17712);
#14381=AXIS2_PLACEMENT_3D('',#41484,#17713,#17714);
#14382=AXIS2_PLACEMENT_3D('',#41486,#17715,#17716);
#14383=AXIS2_PLACEMENT_3D('',#41488,#17717,#17718);
#14384=AXIS2_PLACEMENT_3D('',#41489,#17719,#17720);
#14385=AXIS2_PLACEMENT_3D('',#41491,#17721,#17722);
#14386=AXIS2_PLACEMENT_3D('',#41493,#17723,#17724);
#14387=AXIS2_PLACEMENT_3D('',#41494,#17725,#17726);
#14388=AXIS2_PLACEMENT_3D('',#41603,#17727,#17728);
#14389=AXIS2_PLACEMENT_3D('',#41606,#17729,#17730);
#14390=AXIS2_PLACEMENT_3D('',#41615,#17731,#17732);
#14391=AXIS2_PLACEMENT_3D('',#41623,#17733,#17734);
#14392=AXIS2_PLACEMENT_3D('',#41625,#17735,#17736);
#14393=AXIS2_PLACEMENT_3D('',#41627,#17737,#17738);
#14394=AXIS2_PLACEMENT_3D('',#41637,#17739,#17740);
#14395=AXIS2_PLACEMENT_3D('',#41646,#17741,#17742);
#14396=AXIS2_PLACEMENT_3D('',#41648,#17743,#17744);
#14397=AXIS2_PLACEMENT_3D('',#41650,#17745,#17746);
#14398=AXIS2_PLACEMENT_3D('',#41651,#17747,#17748);
#14399=AXIS2_PLACEMENT_3D('',#41653,#17749,#17750);
#14400=AXIS2_PLACEMENT_3D('',#41655,#17751,#17752);
#14401=AXIS2_PLACEMENT_3D('',#41656,#17753,#17754);
#14402=AXIS2_PLACEMENT_3D('',#41765,#17755,#17756);
#14403=AXIS2_PLACEMENT_3D('',#41768,#17757,#17758);
#14404=AXIS2_PLACEMENT_3D('',#41777,#17759,#17760);
#14405=AXIS2_PLACEMENT_3D('',#41785,#17761,#17762);
#14406=AXIS2_PLACEMENT_3D('',#41787,#17763,#17764);
#14407=AXIS2_PLACEMENT_3D('',#41789,#17765,#17766);
#14408=AXIS2_PLACEMENT_3D('',#41799,#17767,#17768);
#14409=AXIS2_PLACEMENT_3D('',#41808,#17769,#17770);
#14410=AXIS2_PLACEMENT_3D('',#41810,#17771,#17772);
#14411=AXIS2_PLACEMENT_3D('',#41812,#17773,#17774);
#14412=AXIS2_PLACEMENT_3D('',#41813,#17775,#17776);
#14413=AXIS2_PLACEMENT_3D('',#41815,#17777,#17778);
#14414=AXIS2_PLACEMENT_3D('',#41817,#17779,#17780);
#14415=AXIS2_PLACEMENT_3D('',#41818,#17781,#17782);
#14416=AXIS2_PLACEMENT_3D('',#41927,#17783,#17784);
#14417=AXIS2_PLACEMENT_3D('',#41930,#17785,#17786);
#14418=AXIS2_PLACEMENT_3D('',#41932,#17787,#17788);
#14419=AXIS2_PLACEMENT_3D('',#41934,#17789,#17790);
#14420=AXIS2_PLACEMENT_3D('',#41944,#17791,#17792);
#14421=AXIS2_PLACEMENT_3D('',#41953,#17793,#17794);
#14422=AXIS2_PLACEMENT_3D('',#41955,#17795,#17796);
#14423=AXIS2_PLACEMENT_3D('',#41964,#17797,#17798);
#14424=AXIS2_PLACEMENT_3D('',#41972,#17799,#17800);
#14425=AXIS2_PLACEMENT_3D('',#41974,#17801,#17802);
#14426=AXIS2_PLACEMENT_3D('',#41975,#17803,#17804);
#14427=AXIS2_PLACEMENT_3D('',#41978,#17805,#17806);
#14428=AXIS2_PLACEMENT_3D('',#41987,#17807,#17808);
#14429=AXIS2_PLACEMENT_3D('',#41995,#17809,#17810);
#14430=AXIS2_PLACEMENT_3D('',#41997,#17811,#17812);
#14431=AXIS2_PLACEMENT_3D('',#41999,#17813,#17814);
#14432=AXIS2_PLACEMENT_3D('',#42009,#17815,#17816);
#14433=AXIS2_PLACEMENT_3D('',#42018,#17817,#17818);
#14434=AXIS2_PLACEMENT_3D('',#42020,#17819,#17820);
#14435=AXIS2_PLACEMENT_3D('',#42022,#17821,#17822);
#14436=AXIS2_PLACEMENT_3D('',#42023,#17823,#17824);
#14437=AXIS2_PLACEMENT_3D('',#42025,#17825,#17826);
#14438=AXIS2_PLACEMENT_3D('',#42027,#17827,#17828);
#14439=AXIS2_PLACEMENT_3D('',#42028,#17829,#17830);
#14440=AXIS2_PLACEMENT_3D('',#42137,#17831,#17832);
#14441=AXIS2_PLACEMENT_3D('',#42138,#17833,#17834);
#14442=AXIS2_PLACEMENT_3D('',#42139,#17835,#17836);
#14443=AXIS2_PLACEMENT_3D('',#42140,#17837,#17838);
#14444=AXIS2_PLACEMENT_3D('',#42141,#17839,#17840);
#14445=AXIS2_PLACEMENT_3D('',#42142,#17841,#17842);
#14446=AXIS2_PLACEMENT_3D('',#42143,#17843,#17844);
#14447=AXIS2_PLACEMENT_3D('',#42144,#17845,#17846);
#14448=AXIS2_PLACEMENT_3D('',#42145,#17847,#17848);
#14449=AXIS2_PLACEMENT_3D('',#42146,#17849,#17850);
#14450=AXIS2_PLACEMENT_3D('',#42147,#17851,#17852);
#14451=AXIS2_PLACEMENT_3D('',#42148,#17853,#17854);
#14452=AXIS2_PLACEMENT_3D('',#42149,#17855,#17856);
#14453=AXIS2_PLACEMENT_3D('',#42150,#17857,#17858);
#14454=AXIS2_PLACEMENT_3D('',#42151,#17859,#17860);
#14455=AXIS2_PLACEMENT_3D('',#42152,#17861,#17862);
#14456=AXIS2_PLACEMENT_3D('',#42153,#17863,#17864);
#14457=AXIS2_PLACEMENT_3D('',#42154,#17865,#17866);
#14458=AXIS2_PLACEMENT_3D('',#42155,#17867,#17868);
#14459=AXIS2_PLACEMENT_3D('',#42156,#17869,#17870);
#14460=AXIS2_PLACEMENT_3D('',#42157,#17871,#17872);
#14461=AXIS2_PLACEMENT_3D('',#42158,#17873,#17874);
#14462=AXIS2_PLACEMENT_3D('',#42159,#17875,#17876);
#14463=AXIS2_PLACEMENT_3D('',#42160,#17877,#17878);
#14464=AXIS2_PLACEMENT_3D('',#42161,#17879,#17880);
#14465=AXIS2_PLACEMENT_3D('',#42162,#17881,#17882);
#14466=AXIS2_PLACEMENT_3D('',#42163,#17883,#17884);
#14467=AXIS2_PLACEMENT_3D('',#42164,#17885,#17886);
#14468=AXIS2_PLACEMENT_3D('',#42165,#17887,#17888);
#14469=AXIS2_PLACEMENT_3D('',#42166,#17889,#17890);
#14470=AXIS2_PLACEMENT_3D('',#42167,#17891,#17892);
#14471=AXIS2_PLACEMENT_3D('',#42168,#17893,#17894);
#14472=AXIS2_PLACEMENT_3D('',#42169,#17895,#17896);
#14473=AXIS2_PLACEMENT_3D('',#42170,#17897,#17898);
#14474=AXIS2_PLACEMENT_3D('',#42171,#17899,#17900);
#14475=AXIS2_PLACEMENT_3D('',#42172,#17901,#17902);
#14476=AXIS2_PLACEMENT_3D('',#42173,#17903,#17904);
#14477=AXIS2_PLACEMENT_3D('',#42174,#17905,#17906);
#14478=AXIS2_PLACEMENT_3D('',#42175,#17907,#17908);
#14479=AXIS2_PLACEMENT_3D('',#42176,#17909,#17910);
#14480=AXIS2_PLACEMENT_3D('',#42177,#17911,#17912);
#14481=AXIS2_PLACEMENT_3D('',#42178,#17913,#17914);
#14482=AXIS2_PLACEMENT_3D('',#42179,#17915,#17916);
#14483=AXIS2_PLACEMENT_3D('',#42180,#17917,#17918);
#14484=AXIS2_PLACEMENT_3D('',#42181,#17919,#17920);
#14485=AXIS2_PLACEMENT_3D('',#42182,#17921,#17922);
#14486=AXIS2_PLACEMENT_3D('',#42183,#17923,#17924);
#14487=AXIS2_PLACEMENT_3D('',#42184,#17925,#17926);
#14488=AXIS2_PLACEMENT_3D('',#42185,#17927,#17928);
#14489=AXIS2_PLACEMENT_3D('',#42186,#17929,#17930);
#14490=AXIS2_PLACEMENT_3D('',#42187,#17931,#17932);
#14491=AXIS2_PLACEMENT_3D('',#42188,#17933,#17934);
#14492=AXIS2_PLACEMENT_3D('',#42189,#17935,#17936);
#14493=AXIS2_PLACEMENT_3D('',#42190,#17937,#17938);
#14494=AXIS2_PLACEMENT_3D('',#42191,#17939,#17940);
#14495=AXIS2_PLACEMENT_3D('',#42192,#17941,#17942);
#14496=AXIS2_PLACEMENT_3D('',#42193,#17943,#17944);
#14497=AXIS2_PLACEMENT_3D('',#42194,#17945,#17946);
#14498=AXIS2_PLACEMENT_3D('',#42195,#17947,#17948);
#14499=AXIS2_PLACEMENT_3D('',#42196,#17949,#17950);
#14500=AXIS2_PLACEMENT_3D('',#42197,#17951,#17952);
#14501=AXIS2_PLACEMENT_3D('',#42198,#17953,#17954);
#14502=AXIS2_PLACEMENT_3D('',#42199,#17955,#17956);
#14503=AXIS2_PLACEMENT_3D('',#42200,#17957,#17958);
#14504=AXIS2_PLACEMENT_3D('',#42201,#17959,#17960);
#14505=AXIS2_PLACEMENT_3D('',#42202,#17961,#17962);
#14506=AXIS2_PLACEMENT_3D('',#42203,#17963,#17964);
#14507=AXIS2_PLACEMENT_3D('',#42204,#17965,#17966);
#14508=AXIS2_PLACEMENT_3D('',#42205,#17967,#17968);
#14509=AXIS2_PLACEMENT_3D('',#42206,#17969,#17970);
#14510=AXIS2_PLACEMENT_3D('',#42207,#17971,#17972);
#14511=AXIS2_PLACEMENT_3D('',#42208,#17973,#17974);
#14512=AXIS2_PLACEMENT_3D('',#42209,#17975,#17976);
#14513=AXIS2_PLACEMENT_3D('',#42210,#17977,#17978);
#14514=AXIS2_PLACEMENT_3D('',#42211,#17979,#17980);
#14515=AXIS2_PLACEMENT_3D('',#42212,#17981,#17982);
#14516=AXIS2_PLACEMENT_3D('',#42213,#17983,#17984);
#14517=AXIS2_PLACEMENT_3D('',#42214,#17985,#17986);
#14518=AXIS2_PLACEMENT_3D('',#42215,#17987,#17988);
#14519=AXIS2_PLACEMENT_3D('',#42216,#17989,#17990);
#14520=AXIS2_PLACEMENT_3D('',#42217,#17991,#17992);
#14521=AXIS2_PLACEMENT_3D('',#42218,#17993,#17994);
#14522=AXIS2_PLACEMENT_3D('',#42219,#17995,#17996);
#14523=AXIS2_PLACEMENT_3D('',#42220,#17997,#17998);
#14524=AXIS2_PLACEMENT_3D('',#42221,#17999,#18000);
#14525=AXIS2_PLACEMENT_3D('',#42222,#18001,#18002);
#14526=AXIS2_PLACEMENT_3D('',#42223,#18003,#18004);
#14527=AXIS2_PLACEMENT_3D('',#42224,#18005,#18006);
#14528=AXIS2_PLACEMENT_3D('',#42225,#18007,#18008);
#14529=AXIS2_PLACEMENT_3D('',#42226,#18009,#18010);
#14530=AXIS2_PLACEMENT_3D('',#42227,#18011,#18012);
#14531=AXIS2_PLACEMENT_3D('',#42228,#18013,#18014);
#14532=AXIS2_PLACEMENT_3D('',#42229,#18015,#18016);
#14533=AXIS2_PLACEMENT_3D('',#42230,#18017,#18018);
#14534=AXIS2_PLACEMENT_3D('',#42231,#18019,#18020);
#14535=AXIS2_PLACEMENT_3D('',#42232,#18021,#18022);
#14536=AXIS2_PLACEMENT_3D('',#42233,#18023,#18024);
#14537=AXIS2_PLACEMENT_3D('',#42234,#18025,#18026);
#14538=AXIS2_PLACEMENT_3D('',#42235,#18027,#18028);
#14539=AXIS2_PLACEMENT_3D('',#42236,#18029,#18030);
#14540=AXIS2_PLACEMENT_3D('',#42237,#18031,#18032);
#14541=AXIS2_PLACEMENT_3D('',#42238,#18033,#18034);
#14542=AXIS2_PLACEMENT_3D('',#42239,#18035,#18036);
#14543=AXIS2_PLACEMENT_3D('',#42240,#18037,#18038);
#14544=AXIS2_PLACEMENT_3D('',#42241,#18039,#18040);
#14545=AXIS2_PLACEMENT_3D('',#42242,#18041,#18042);
#14546=AXIS2_PLACEMENT_3D('',#42243,#18043,#18044);
#14547=AXIS2_PLACEMENT_3D('',#42244,#18045,#18046);
#14548=AXIS2_PLACEMENT_3D('',#42245,#18047,#18048);
#14549=AXIS2_PLACEMENT_3D('',#42246,#18049,#18050);
#14550=AXIS2_PLACEMENT_3D('',#42247,#18051,#18052);
#14551=AXIS2_PLACEMENT_3D('',#42248,#18053,#18054);
#14552=AXIS2_PLACEMENT_3D('',#42249,#18055,#18056);
#14553=AXIS2_PLACEMENT_3D('',#42250,#18057,#18058);
#14554=AXIS2_PLACEMENT_3D('',#42251,#18059,#18060);
#14555=AXIS2_PLACEMENT_3D('',#42252,#18061,#18062);
#14556=AXIS2_PLACEMENT_3D('',#42253,#18063,#18064);
#14557=AXIS2_PLACEMENT_3D('',#42254,#18065,#18066);
#14558=AXIS2_PLACEMENT_3D('',#42255,#18067,#18068);
#14559=AXIS2_PLACEMENT_3D('',#42256,#18069,#18070);
#14560=AXIS2_PLACEMENT_3D('',#42257,#18071,#18072);
#14561=AXIS2_PLACEMENT_3D('',#42258,#18073,#18074);
#14562=AXIS2_PLACEMENT_3D('',#42259,#18075,#18076);
#14563=AXIS2_PLACEMENT_3D('',#42260,#18077,#18078);
#14564=AXIS2_PLACEMENT_3D('',#42261,#18079,#18080);
#14565=AXIS2_PLACEMENT_3D('',#42262,#18081,#18082);
#14566=AXIS2_PLACEMENT_3D('',#42263,#18083,#18084);
#14567=AXIS2_PLACEMENT_3D('',#42264,#18085,#18086);
#14568=AXIS2_PLACEMENT_3D('',#42266,#18087,#18088);
#14569=AXIS2_PLACEMENT_3D('',#42268,#18089,#18090);
#14570=AXIS2_PLACEMENT_3D('',#42269,#18091,#18092);
#14571=AXIS2_PLACEMENT_3D('',#42270,#18093,#18094);
#14572=AXIS2_PLACEMENT_3D('',#42273,#18095,#18096);
#14573=AXIS2_PLACEMENT_3D('',#42275,#18097,#18098);
#14574=AXIS2_PLACEMENT_3D('',#42277,#18099,#18100);
#14575=AXIS2_PLACEMENT_3D('',#42278,#18101,#18102);
#14576=AXIS2_PLACEMENT_3D('',#42279,#18103,#18104);
#14577=AXIS2_PLACEMENT_3D('',#42280,#18105,#18106);
#14578=AXIS2_PLACEMENT_3D('',#42283,#18107,#18108);
#14579=AXIS2_PLACEMENT_3D('',#42285,#18109,#18110);
#14580=AXIS2_PLACEMENT_3D('',#42286,#18111,#18112);
#14581=AXIS2_PLACEMENT_3D('',#42287,#18113,#18114);
#14582=AXIS2_PLACEMENT_3D('',#42288,#18115,#18116);
#14583=AXIS2_PLACEMENT_3D('',#42291,#18118,#18119);
#14584=AXIS2_PLACEMENT_3D('',#42292,#18120,#18121);
#14585=AXIS2_PLACEMENT_3D('',#42294,#18123,#18124);
#14586=AXIS2_PLACEMENT_3D('',#42297,#18126,#18127);
#14587=AXIS2_PLACEMENT_3D('',#42298,#18128,#18129);
#14588=AXIS2_PLACEMENT_3D('',#42300,#18130,#18131);
#14589=AXIS2_PLACEMENT_3D('',#42302,#18133,#18134);
#14590=AXIS2_PLACEMENT_3D('',#42305,#18136,#18137);
#14591=AXIS2_PLACEMENT_3D('',#42306,#18138,#18139);
#14592=AXIS2_PLACEMENT_3D('',#42307,#18140,#18141);
#14593=AXIS2_PLACEMENT_3D('',#42308,#18142,#18143);
#14594=AXIS2_PLACEMENT_3D('',#42311,#18144,#18145);
#14595=AXIS2_PLACEMENT_3D('',#42312,#18146,#18147);
#14596=AXIS2_PLACEMENT_3D('',#42315,#18148,#18149);
#14597=AXIS2_PLACEMENT_3D('',#42316,#18150,#18151);
#14598=AXIS2_PLACEMENT_3D('',#42319,#18152,#18153);
#14599=AXIS2_PLACEMENT_3D('',#42320,#18154,#18155);
#14600=AXIS2_PLACEMENT_3D('',#42323,#18156,#18157);
#14601=AXIS2_PLACEMENT_3D('',#42324,#18158,#18159);
#14602=AXIS2_PLACEMENT_3D('',#42327,#18160,#18161);
#14603=AXIS2_PLACEMENT_3D('',#42328,#18162,#18163);
#14604=AXIS2_PLACEMENT_3D('',#42331,#18164,#18165);
#14605=AXIS2_PLACEMENT_3D('',#42332,#18166,#18167);
#14606=AXIS2_PLACEMENT_3D('',#42335,#18168,#18169);
#14607=AXIS2_PLACEMENT_3D('',#42336,#18170,#18171);
#14608=AXIS2_PLACEMENT_3D('',#42338,#18172,#18173);
#14609=AXIS2_PLACEMENT_3D('',#42340,#18174,#18175);
#14610=AXIS2_PLACEMENT_3D('',#42342,#18176,#18177);
#14611=AXIS2_PLACEMENT_3D('',#42343,#18178,#18179);
#14612=AXIS2_PLACEMENT_3D('',#42344,#18180,#18181);
#14613=AXIS2_PLACEMENT_3D('',#42346,#18182,#18183);
#14614=AXIS2_PLACEMENT_3D('',#42348,#18184,#18185);
#14615=AXIS2_PLACEMENT_3D('',#42349,#18186,#18187);
#14616=AXIS2_PLACEMENT_3D('',#42350,#18188,#18189);
#14617=AXIS2_PLACEMENT_3D('',#42352,#18190,#18191);
#14618=AXIS2_PLACEMENT_3D('',#42354,#18192,#18193);
#14619=AXIS2_PLACEMENT_3D('',#42355,#18194,#18195);
#14620=AXIS2_PLACEMENT_3D('',#42356,#18196,#18197);
#14621=AXIS2_PLACEMENT_3D('',#42359,#18198,#18199);
#14622=AXIS2_PLACEMENT_3D('',#42361,#18200,#18201);
#14623=AXIS2_PLACEMENT_3D('',#42362,#18202,#18203);
#14624=AXIS2_PLACEMENT_3D('',#42363,#18204,#18205);
#14625=AXIS2_PLACEMENT_3D('',#42364,#18206,#18207);
#14626=AXIS2_PLACEMENT_3D('',#42366,#18208,#18209);
#14627=AXIS2_PLACEMENT_3D('',#42369,#18211,#18212);
#14628=AXIS2_PLACEMENT_3D('',#42370,#18213,#18214);
#14629=AXIS2_PLACEMENT_3D('',#42373,#18216,#18217);
#14630=AXIS2_PLACEMENT_3D('',#42374,#18218,#18219);
#14631=AXIS2_PLACEMENT_3D('',#42376,#18220,#18221);
#14632=AXIS2_PLACEMENT_3D('',#42378,#18223,#18224);
#14633=AXIS2_PLACEMENT_3D('',#42380,#18225,#18226);
#14634=AXIS2_PLACEMENT_3D('',#42381,#18227,#18228);
#14635=AXIS2_PLACEMENT_3D('',#42382,#18229,#18230);
#14636=AXIS2_PLACEMENT_3D('',#42384,#18232,#18233);
#14637=AXIS2_PLACEMENT_3D('',#42386,#18234,#18235);
#14638=AXIS2_PLACEMENT_3D('',#42388,#18237,#18238);
#14639=AXIS2_PLACEMENT_3D('',#42390,#18239,#18240);
#14640=AXIS2_PLACEMENT_3D('',#42393,#18242,#18243);
#14641=AXIS2_PLACEMENT_3D('',#42394,#18244,#18245);
#14642=AXIS2_PLACEMENT_3D('',#42396,#18246,#18247);
#14643=AXIS2_PLACEMENT_3D('',#42399,#18249,#18250);
#14644=AXIS2_PLACEMENT_3D('',#42400,#18251,#18252);
#14645=AXIS2_PLACEMENT_3D('',#42403,#18253,#18254);
#14646=AXIS2_PLACEMENT_3D('',#42404,#18255,#18256);
#14647=AXIS2_PLACEMENT_3D('',#42407,#18258,#18259);
#14648=AXIS2_PLACEMENT_3D('',#42408,#18260,#18261);
#14649=AXIS2_PLACEMENT_3D('',#42410,#18263,#18264);
#14650=AXIS2_PLACEMENT_3D('',#42411,#18265,#18266);
#14651=AXIS2_PLACEMENT_3D('',#42412,#18267,#18268);
#14652=AXIS2_PLACEMENT_3D('',#42413,#18269,#18270);
#14653=AXIS2_PLACEMENT_3D('',#42414,#18271,#18272);
#14654=AXIS2_PLACEMENT_3D('',#42415,#18273,#18274);
#14655=AXIS2_PLACEMENT_3D('',#42416,#18275,#18276);
#14656=AXIS2_PLACEMENT_3D('',#42418,#18277,#18278);
#14657=AXIS2_PLACEMENT_3D('',#42420,#18279,#18280);
#14658=AXIS2_PLACEMENT_3D('',#42421,#18281,#18282);
#14659=AXIS2_PLACEMENT_3D('',#42530,#18283,#18284);
#14660=AXIS2_PLACEMENT_3D('',#42533,#18285,#18286);
#14661=AXIS2_PLACEMENT_3D('',#42542,#18287,#18288);
#14662=AXIS2_PLACEMENT_3D('',#42550,#18289,#18290);
#14663=AXIS2_PLACEMENT_3D('',#42552,#18291,#18292);
#14664=AXIS2_PLACEMENT_3D('',#42554,#18293,#18294);
#14665=AXIS2_PLACEMENT_3D('',#42564,#18295,#18296);
#14666=AXIS2_PLACEMENT_3D('',#42573,#18297,#18298);
#14667=AXIS2_PLACEMENT_3D('',#42575,#18299,#18300);
#14668=AXIS2_PLACEMENT_3D('',#42577,#18301,#18302);
#14669=AXIS2_PLACEMENT_3D('',#42578,#18303,#18304);
#14670=AXIS2_PLACEMENT_3D('',#42580,#18305,#18306);
#14671=AXIS2_PLACEMENT_3D('',#42582,#18307,#18308);
#14672=AXIS2_PLACEMENT_3D('',#42583,#18309,#18310);
#14673=AXIS2_PLACEMENT_3D('',#42692,#18311,#18312);
#14674=AXIS2_PLACEMENT_3D('',#42695,#18313,#18314);
#14675=AXIS2_PLACEMENT_3D('',#42704,#18315,#18316);
#14676=AXIS2_PLACEMENT_3D('',#42712,#18317,#18318);
#14677=AXIS2_PLACEMENT_3D('',#42714,#18319,#18320);
#14678=AXIS2_PLACEMENT_3D('',#42716,#18321,#18322);
#14679=AXIS2_PLACEMENT_3D('',#42726,#18323,#18324);
#14680=AXIS2_PLACEMENT_3D('',#42735,#18325,#18326);
#14681=AXIS2_PLACEMENT_3D('',#42737,#18327,#18328);
#14682=AXIS2_PLACEMENT_3D('',#42739,#18329,#18330);
#14683=AXIS2_PLACEMENT_3D('',#42740,#18331,#18332);
#14684=AXIS2_PLACEMENT_3D('',#42742,#18333,#18334);
#14685=AXIS2_PLACEMENT_3D('',#42744,#18335,#18336);
#14686=AXIS2_PLACEMENT_3D('',#42745,#18337,#18338);
#14687=AXIS2_PLACEMENT_3D('',#42854,#18339,#18340);
#14688=AXIS2_PLACEMENT_3D('',#42857,#18341,#18342);
#14689=AXIS2_PLACEMENT_3D('',#42866,#18343,#18344);
#14690=AXIS2_PLACEMENT_3D('',#42874,#18345,#18346);
#14691=AXIS2_PLACEMENT_3D('',#42876,#18347,#18348);
#14692=AXIS2_PLACEMENT_3D('',#42878,#18349,#18350);
#14693=AXIS2_PLACEMENT_3D('',#42888,#18351,#18352);
#14694=AXIS2_PLACEMENT_3D('',#42897,#18353,#18354);
#14695=AXIS2_PLACEMENT_3D('',#42899,#18355,#18356);
#14696=AXIS2_PLACEMENT_3D('',#42901,#18357,#18358);
#14697=AXIS2_PLACEMENT_3D('',#42902,#18359,#18360);
#14698=AXIS2_PLACEMENT_3D('',#42904,#18361,#18362);
#14699=AXIS2_PLACEMENT_3D('',#42906,#18363,#18364);
#14700=AXIS2_PLACEMENT_3D('',#42907,#18365,#18366);
#14701=AXIS2_PLACEMENT_3D('',#43016,#18367,#18368);
#14702=AXIS2_PLACEMENT_3D('',#43019,#18369,#18370);
#14703=AXIS2_PLACEMENT_3D('',#43028,#18371,#18372);
#14704=AXIS2_PLACEMENT_3D('',#43036,#18373,#18374);
#14705=AXIS2_PLACEMENT_3D('',#43038,#18375,#18376);
#14706=AXIS2_PLACEMENT_3D('',#43040,#18377,#18378);
#14707=AXIS2_PLACEMENT_3D('',#43050,#18379,#18380);
#14708=AXIS2_PLACEMENT_3D('',#43059,#18381,#18382);
#14709=AXIS2_PLACEMENT_3D('',#43061,#18383,#18384);
#14710=AXIS2_PLACEMENT_3D('',#43063,#18385,#18386);
#14711=AXIS2_PLACEMENT_3D('',#43064,#18387,#18388);
#14712=AXIS2_PLACEMENT_3D('',#43066,#18389,#18390);
#14713=AXIS2_PLACEMENT_3D('',#43068,#18391,#18392);
#14714=AXIS2_PLACEMENT_3D('',#43069,#18393,#18394);
#14715=AXIS2_PLACEMENT_3D('',#43178,#18395,#18396);
#14716=AXIS2_PLACEMENT_3D('',#43181,#18397,#18398);
#14717=AXIS2_PLACEMENT_3D('',#43190,#18399,#18400);
#14718=AXIS2_PLACEMENT_3D('',#43198,#18401,#18402);
#14719=AXIS2_PLACEMENT_3D('',#43200,#18403,#18404);
#14720=AXIS2_PLACEMENT_3D('',#43202,#18405,#18406);
#14721=AXIS2_PLACEMENT_3D('',#43212,#18407,#18408);
#14722=AXIS2_PLACEMENT_3D('',#43221,#18409,#18410);
#14723=AXIS2_PLACEMENT_3D('',#43223,#18411,#18412);
#14724=AXIS2_PLACEMENT_3D('',#43225,#18413,#18414);
#14725=AXIS2_PLACEMENT_3D('',#43226,#18415,#18416);
#14726=AXIS2_PLACEMENT_3D('',#43228,#18417,#18418);
#14727=AXIS2_PLACEMENT_3D('',#43230,#18419,#18420);
#14728=AXIS2_PLACEMENT_3D('',#43231,#18421,#18422);
#14729=AXIS2_PLACEMENT_3D('',#43340,#18423,#18424);
#14730=AXIS2_PLACEMENT_3D('',#43343,#18425,#18426);
#14731=AXIS2_PLACEMENT_3D('',#43345,#18427,#18428);
#14732=AXIS2_PLACEMENT_3D('',#43347,#18429,#18430);
#14733=AXIS2_PLACEMENT_3D('',#43357,#18431,#18432);
#14734=AXIS2_PLACEMENT_3D('',#43366,#18433,#18434);
#14735=AXIS2_PLACEMENT_3D('',#43368,#18435,#18436);
#14736=AXIS2_PLACEMENT_3D('',#43377,#18437,#18438);
#14737=AXIS2_PLACEMENT_3D('',#43385,#18439,#18440);
#14738=AXIS2_PLACEMENT_3D('',#43387,#18441,#18442);
#14739=AXIS2_PLACEMENT_3D('',#43388,#18443,#18444);
#14740=AXIS2_PLACEMENT_3D('',#43391,#18445,#18446);
#14741=AXIS2_PLACEMENT_3D('',#43400,#18447,#18448);
#14742=AXIS2_PLACEMENT_3D('',#43408,#18449,#18450);
#14743=AXIS2_PLACEMENT_3D('',#43410,#18451,#18452);
#14744=AXIS2_PLACEMENT_3D('',#43412,#18453,#18454);
#14745=AXIS2_PLACEMENT_3D('',#43422,#18455,#18456);
#14746=AXIS2_PLACEMENT_3D('',#43431,#18457,#18458);
#14747=AXIS2_PLACEMENT_3D('',#43433,#18459,#18460);
#14748=AXIS2_PLACEMENT_3D('',#43435,#18461,#18462);
#14749=AXIS2_PLACEMENT_3D('',#43436,#18463,#18464);
#14750=AXIS2_PLACEMENT_3D('',#43438,#18465,#18466);
#14751=AXIS2_PLACEMENT_3D('',#43440,#18467,#18468);
#14752=AXIS2_PLACEMENT_3D('',#43441,#18469,#18470);
#14753=AXIS2_PLACEMENT_3D('',#43550,#18471,#18472);
#14754=AXIS2_PLACEMENT_3D('',#43551,#18473,#18474);
#14755=AXIS2_PLACEMENT_3D('',#43552,#18475,#18476);
#14756=AXIS2_PLACEMENT_3D('',#43553,#18477,#18478);
#14757=AXIS2_PLACEMENT_3D('',#43554,#18479,#18480);
#14758=AXIS2_PLACEMENT_3D('',#43555,#18481,#18482);
#14759=AXIS2_PLACEMENT_3D('',#43556,#18483,#18484);
#14760=AXIS2_PLACEMENT_3D('',#43557,#18485,#18486);
#14761=AXIS2_PLACEMENT_3D('',#43558,#18487,#18488);
#14762=AXIS2_PLACEMENT_3D('',#43559,#18489,#18490);
#14763=AXIS2_PLACEMENT_3D('',#43560,#18491,#18492);
#14764=AXIS2_PLACEMENT_3D('',#43561,#18493,#18494);
#14765=AXIS2_PLACEMENT_3D('',#43562,#18495,#18496);
#14766=AXIS2_PLACEMENT_3D('',#43563,#18497,#18498);
#14767=AXIS2_PLACEMENT_3D('',#43564,#18499,#18500);
#14768=AXIS2_PLACEMENT_3D('',#43565,#18501,#18502);
#14769=AXIS2_PLACEMENT_3D('',#43566,#18503,#18504);
#14770=AXIS2_PLACEMENT_3D('',#43567,#18505,#18506);
#14771=AXIS2_PLACEMENT_3D('',#43568,#18507,#18508);
#14772=AXIS2_PLACEMENT_3D('',#43569,#18509,#18510);
#14773=AXIS2_PLACEMENT_3D('',#43570,#18511,#18512);
#14774=AXIS2_PLACEMENT_3D('',#43571,#18513,#18514);
#14775=AXIS2_PLACEMENT_3D('',#43572,#18515,#18516);
#14776=AXIS2_PLACEMENT_3D('',#43573,#18517,#18518);
#14777=AXIS2_PLACEMENT_3D('',#43574,#18519,#18520);
#14778=AXIS2_PLACEMENT_3D('',#43575,#18521,#18522);
#14779=AXIS2_PLACEMENT_3D('',#43576,#18523,#18524);
#14780=AXIS2_PLACEMENT_3D('',#43577,#18525,#18526);
#14781=AXIS2_PLACEMENT_3D('',#43578,#18527,#18528);
#14782=AXIS2_PLACEMENT_3D('',#43579,#18529,#18530);
#14783=AXIS2_PLACEMENT_3D('',#43580,#18531,#18532);
#14784=AXIS2_PLACEMENT_3D('',#43581,#18533,#18534);
#14785=AXIS2_PLACEMENT_3D('',#43582,#18535,#18536);
#14786=AXIS2_PLACEMENT_3D('',#43583,#18537,#18538);
#14787=AXIS2_PLACEMENT_3D('',#43584,#18539,#18540);
#14788=AXIS2_PLACEMENT_3D('',#43585,#18541,#18542);
#14789=AXIS2_PLACEMENT_3D('',#43586,#18543,#18544);
#14790=AXIS2_PLACEMENT_3D('',#43587,#18545,#18546);
#14791=AXIS2_PLACEMENT_3D('',#43588,#18547,#18548);
#14792=AXIS2_PLACEMENT_3D('',#43589,#18549,#18550);
#14793=AXIS2_PLACEMENT_3D('',#43590,#18551,#18552);
#14794=AXIS2_PLACEMENT_3D('',#43591,#18553,#18554);
#14795=AXIS2_PLACEMENT_3D('',#43592,#18555,#18556);
#14796=AXIS2_PLACEMENT_3D('',#43593,#18557,#18558);
#14797=AXIS2_PLACEMENT_3D('',#43594,#18559,#18560);
#14798=AXIS2_PLACEMENT_3D('',#43595,#18561,#18562);
#14799=AXIS2_PLACEMENT_3D('',#43596,#18563,#18564);
#14800=AXIS2_PLACEMENT_3D('',#43597,#18565,#18566);
#14801=AXIS2_PLACEMENT_3D('',#43598,#18567,#18568);
#14802=AXIS2_PLACEMENT_3D('',#43599,#18569,#18570);
#14803=AXIS2_PLACEMENT_3D('',#43600,#18571,#18572);
#14804=AXIS2_PLACEMENT_3D('',#43601,#18573,#18574);
#14805=AXIS2_PLACEMENT_3D('',#43602,#18575,#18576);
#14806=AXIS2_PLACEMENT_3D('',#43603,#18577,#18578);
#14807=AXIS2_PLACEMENT_3D('',#43604,#18579,#18580);
#14808=AXIS2_PLACEMENT_3D('',#43605,#18581,#18582);
#14809=AXIS2_PLACEMENT_3D('',#43606,#18583,#18584);
#14810=AXIS2_PLACEMENT_3D('',#43607,#18585,#18586);
#14811=AXIS2_PLACEMENT_3D('',#43608,#18587,#18588);
#14812=AXIS2_PLACEMENT_3D('',#43609,#18589,#18590);
#14813=AXIS2_PLACEMENT_3D('',#43610,#18591,#18592);
#14814=AXIS2_PLACEMENT_3D('',#43611,#18593,#18594);
#14815=AXIS2_PLACEMENT_3D('',#43612,#18595,#18596);
#14816=AXIS2_PLACEMENT_3D('',#43613,#18597,#18598);
#14817=AXIS2_PLACEMENT_3D('',#43614,#18599,#18600);
#14818=AXIS2_PLACEMENT_3D('',#43615,#18601,#18602);
#14819=AXIS2_PLACEMENT_3D('',#43616,#18603,#18604);
#14820=AXIS2_PLACEMENT_3D('',#43617,#18605,#18606);
#14821=AXIS2_PLACEMENT_3D('',#43618,#18607,#18608);
#14822=AXIS2_PLACEMENT_3D('',#43619,#18609,#18610);
#14823=AXIS2_PLACEMENT_3D('',#43620,#18611,#18612);
#14824=AXIS2_PLACEMENT_3D('',#43621,#18613,#18614);
#14825=AXIS2_PLACEMENT_3D('',#43622,#18615,#18616);
#14826=AXIS2_PLACEMENT_3D('',#43623,#18617,#18618);
#14827=AXIS2_PLACEMENT_3D('',#43624,#18619,#18620);
#14828=AXIS2_PLACEMENT_3D('',#43625,#18621,#18622);
#14829=AXIS2_PLACEMENT_3D('',#43626,#18623,#18624);
#14830=AXIS2_PLACEMENT_3D('',#43627,#18625,#18626);
#14831=AXIS2_PLACEMENT_3D('',#43628,#18627,#18628);
#14832=AXIS2_PLACEMENT_3D('',#43629,#18629,#18630);
#14833=AXIS2_PLACEMENT_3D('',#43630,#18631,#18632);
#14834=AXIS2_PLACEMENT_3D('',#43631,#18633,#18634);
#14835=AXIS2_PLACEMENT_3D('',#43632,#18635,#18636);
#14836=AXIS2_PLACEMENT_3D('',#43633,#18637,#18638);
#14837=AXIS2_PLACEMENT_3D('',#43634,#18639,#18640);
#14838=AXIS2_PLACEMENT_3D('',#43635,#18641,#18642);
#14839=AXIS2_PLACEMENT_3D('',#43636,#18643,#18644);
#14840=AXIS2_PLACEMENT_3D('',#43637,#18645,#18646);
#14841=AXIS2_PLACEMENT_3D('',#43638,#18647,#18648);
#14842=AXIS2_PLACEMENT_3D('',#43639,#18649,#18650);
#14843=AXIS2_PLACEMENT_3D('',#43640,#18651,#18652);
#14844=AXIS2_PLACEMENT_3D('',#43641,#18653,#18654);
#14845=AXIS2_PLACEMENT_3D('',#43642,#18655,#18656);
#14846=AXIS2_PLACEMENT_3D('',#43643,#18657,#18658);
#14847=AXIS2_PLACEMENT_3D('',#43644,#18659,#18660);
#14848=AXIS2_PLACEMENT_3D('',#43645,#18661,#18662);
#14849=AXIS2_PLACEMENT_3D('',#43646,#18663,#18664);
#14850=AXIS2_PLACEMENT_3D('',#43647,#18665,#18666);
#14851=AXIS2_PLACEMENT_3D('',#43648,#18667,#18668);
#14852=AXIS2_PLACEMENT_3D('',#43649,#18669,#18670);
#14853=AXIS2_PLACEMENT_3D('',#43650,#18671,#18672);
#14854=AXIS2_PLACEMENT_3D('',#43651,#18673,#18674);
#14855=AXIS2_PLACEMENT_3D('',#43652,#18675,#18676);
#14856=AXIS2_PLACEMENT_3D('',#43653,#18677,#18678);
#14857=AXIS2_PLACEMENT_3D('',#43654,#18679,#18680);
#14858=AXIS2_PLACEMENT_3D('',#43655,#18681,#18682);
#14859=AXIS2_PLACEMENT_3D('',#43656,#18683,#18684);
#14860=AXIS2_PLACEMENT_3D('',#43657,#18685,#18686);
#14861=AXIS2_PLACEMENT_3D('',#43658,#18687,#18688);
#14862=AXIS2_PLACEMENT_3D('',#43659,#18689,#18690);
#14863=AXIS2_PLACEMENT_3D('',#43660,#18691,#18692);
#14864=AXIS2_PLACEMENT_3D('',#43661,#18693,#18694);
#14865=AXIS2_PLACEMENT_3D('',#43662,#18695,#18696);
#14866=AXIS2_PLACEMENT_3D('',#43663,#18697,#18698);
#14867=AXIS2_PLACEMENT_3D('',#43664,#18699,#18700);
#14868=AXIS2_PLACEMENT_3D('',#43665,#18701,#18702);
#14869=AXIS2_PLACEMENT_3D('',#43666,#18703,#18704);
#14870=AXIS2_PLACEMENT_3D('',#43667,#18705,#18706);
#14871=AXIS2_PLACEMENT_3D('',#43668,#18707,#18708);
#14872=AXIS2_PLACEMENT_3D('',#43669,#18709,#18710);
#14873=AXIS2_PLACEMENT_3D('',#43670,#18711,#18712);
#14874=AXIS2_PLACEMENT_3D('',#43671,#18713,#18714);
#14875=AXIS2_PLACEMENT_3D('',#43672,#18715,#18716);
#14876=AXIS2_PLACEMENT_3D('',#43673,#18717,#18718);
#14877=AXIS2_PLACEMENT_3D('',#43674,#18719,#18720);
#14878=AXIS2_PLACEMENT_3D('',#43675,#18721,#18722);
#14879=AXIS2_PLACEMENT_3D('',#43676,#18723,#18724);
#14880=AXIS2_PLACEMENT_3D('',#43677,#18725,#18726);
#14881=AXIS2_PLACEMENT_3D('',#43679,#18727,#18728);
#14882=AXIS2_PLACEMENT_3D('',#43682,#18730,#18731);
#14883=AXIS2_PLACEMENT_3D('',#43683,#18732,#18733);
#14884=AXIS2_PLACEMENT_3D('',#43693,#18738,#18739);
#14885=AXIS2_PLACEMENT_3D('',#43694,#18740,#18741);
#14886=AXIS2_PLACEMENT_3D('',#43697,#18743,#18744);
#14887=AXIS2_PLACEMENT_3D('',#43698,#18745,#18746);
#14888=AXIS2_PLACEMENT_3D('',#43707,#18751,#18752);
#14889=AXIS2_PLACEMENT_3D('',#43710,#18755,#18756);
#14890=AXIS2_PLACEMENT_3D('',#43712,#18758,#18759);
#14891=AXIS2_PLACEMENT_3D('',#43714,#18761,#18762);
#14892=AXIS2_PLACEMENT_3D('',#43715,#18763,#18764);
#14893=AXIS2_PLACEMENT_3D('',#43716,#18765,#18766);
#14894=AXIS2_PLACEMENT_3D('',#43718,#18767,#18768);
#14895=AXIS2_PLACEMENT_3D('',#43721,#18770,#18771);
#14896=AXIS2_PLACEMENT_3D('',#43722,#18772,#18773);
#14897=AXIS2_PLACEMENT_3D('',#43724,#18774,#18775);
#14898=AXIS2_PLACEMENT_3D('',#43727,#18777,#18778);
#14899=AXIS2_PLACEMENT_3D('',#43728,#18779,#18780);
#14900=AXIS2_PLACEMENT_3D('',#43737,#18785,#18786);
#14901=AXIS2_PLACEMENT_3D('',#43743,#18790,#18791);
#14902=AXIS2_PLACEMENT_3D('',#43747,#18794,#18795);
#14903=AXIS2_PLACEMENT_3D('',#43751,#18798,#18799);
#14904=AXIS2_PLACEMENT_3D('',#43753,#18801,#18802);
#14905=AXIS2_PLACEMENT_3D('',#43754,#18803,#18804);
#14906=AXIS2_PLACEMENT_3D('',#43755,#18805,#18806);
#14907=AXIS2_PLACEMENT_3D('',#43756,#18807,#18808);
#14908=AXIS2_PLACEMENT_3D('',#43757,#18809,#18810);
#14909=AXIS2_PLACEMENT_3D('',#43758,#18811,#18812);
#14910=AXIS2_PLACEMENT_3D('',#43759,#18813,#18814);
#14911=AXIS2_PLACEMENT_3D('',#43760,#18815,#18816);
#14912=AXIS2_PLACEMENT_3D('',#43761,#18817,#18818);
#14913=DIRECTION('axis',(0.,0.,1.));
#14914=DIRECTION('refdir',(1.,0.,0.));
#14915=DIRECTION('axis',(0.,0.,1.));
#14916=DIRECTION('refdir',(1.,0.,0.));
#14917=DIRECTION('center_axis',(0.,-2.4980018054066E-16,-1.));
#14918=DIRECTION('ref_axis',(1.,0.,0.));
#14919=DIRECTION('center_axis',(0.,-2.4980018054066E-16,-1.));
#14920=DIRECTION('ref_axis',(1.,0.,0.));
#14921=DIRECTION('',(0.,2.4980018054066E-16,1.));
#14922=DIRECTION('center_axis',(0.,-2.4980018054066E-16,-1.));
#14923=DIRECTION('ref_axis',(1.,0.,0.));
#14924=DIRECTION('center_axis',(0.,-2.4980018054066E-16,-1.));
#14925=DIRECTION('ref_axis',(1.,0.,0.));
#14926=DIRECTION('center_axis',(0.,-2.4980018054066E-16,-1.));
#14927=DIRECTION('ref_axis',(1.,0.,0.));
#14928=DIRECTION('',(0.,2.4980018054066E-16,1.));
#14929=DIRECTION('center_axis',(0.,2.4980018054066E-16,1.));
#14930=DIRECTION('ref_axis',(1.,0.,0.));
#14931=DIRECTION('center_axis',(0.,-2.4980018054066E-16,-1.));
#14932=DIRECTION('ref_axis',(1.,0.,0.));
#14933=DIRECTION('center_axis',(0.,-2.4980018054066E-16,-1.));
#14934=DIRECTION('ref_axis',(1.,0.,0.));
#14935=DIRECTION('center_axis',(0.,0.,-1.));
#14936=DIRECTION('ref_axis',(-0.837321103817045,-0.546711412998307,0.));
#14937=DIRECTION('center_axis',(0.,0.,1.));
#14938=DIRECTION('ref_axis',(-0.837321103817045,-0.546711412998307,0.));
#14939=DIRECTION('',(0.,0.,-1.));
#14940=DIRECTION('center_axis',(0.,0.,-1.));
#14941=DIRECTION('ref_axis',(-0.837321103817045,-0.546711412998307,0.));
#14942=DIRECTION('',(0.,0.,1.));
#14943=DIRECTION('center_axis',(0.21892739748686,0.975741151448288,0.));
#14944=DIRECTION('ref_axis',(-0.975741151448288,0.21892739748686,0.));
#14945=DIRECTION('',(-0.975741151448288,0.218927397486859,0.));
#14946=DIRECTION('',(0.,0.,1.));
#14947=DIRECTION('',(0.975741151448288,-0.218927397486859,0.));
#14948=DIRECTION('center_axis',(0.,0.,1.));
#14949=DIRECTION('ref_axis',(-0.356058096916393,0.934463820391285,0.));
#14950=DIRECTION('center_axis',(0.,0.,-1.));
#14951=DIRECTION('ref_axis',(-0.356058096916393,0.934463820391285,0.));
#14952=DIRECTION('',(0.,0.,1.));
#14953=DIRECTION('center_axis',(0.,0.,1.));
#14954=DIRECTION('ref_axis',(-0.356058096916393,0.934463820391285,0.));
#14955=DIRECTION('',(0.,0.,-1.));
#14956=DIRECTION('center_axis',(-0.396410273775032,-0.918073469198192,0.));
#14957=DIRECTION('ref_axis',(0.918073469198192,-0.396410273775032,0.));
#14958=DIRECTION('',(0.918073469198192,-0.396410273775032,0.));
#14959=DIRECTION('',(0.,0.,1.));
#14960=DIRECTION('',(0.918073469198192,-0.396410273775032,0.));
#14961=DIRECTION('center_axis',(0.,0.,-1.));
#14962=DIRECTION('ref_axis',(-0.96528280965187,-0.261207001036709,0.));
#14963=DIRECTION('center_axis',(0.,0.,1.));
#14964=DIRECTION('ref_axis',(-0.96528280965187,-0.261207001036709,0.));
#14965=DIRECTION('',(0.,0.,-1.));
#14966=DIRECTION('center_axis',(0.,0.,-1.));
#14967=DIRECTION('ref_axis',(-0.96528280965187,-0.261207001036709,0.));
#14968=DIRECTION('',(0.,0.,1.));
#14969=DIRECTION('center_axis',(0.509732925883917,0.860332693944512,0.));
#14970=DIRECTION('ref_axis',(-0.860332693944512,0.509732925883917,0.));
#14971=DIRECTION('',(-0.860332693944512,0.509732925883917,0.));
#14972=DIRECTION('',(0.,0.,1.));
#14973=DIRECTION('',(0.860332693944512,-0.509732925883917,0.));
#14974=DIRECTION('center_axis',(0.,0.,1.));
#14975=DIRECTION('ref_axis',(-0.0498661721225461,0.998755908557163,0.));
#14976=DIRECTION('center_axis',(0.,0.,-1.));
#14977=DIRECTION('ref_axis',(-0.0498661721225461,0.998755908557163,0.));
#14978=DIRECTION('',(0.,0.,1.));
#14979=DIRECTION('center_axis',(0.,0.,1.));
#14980=DIRECTION('ref_axis',(-0.0498661721225461,0.998755908557163,0.));
#14981=DIRECTION('',(0.,0.,-1.));
#14982=DIRECTION('center_axis',(-0.660708878067096,-0.750642243977328,0.));
#14983=DIRECTION('ref_axis',(0.750642243977328,-0.660708878067096,0.));
#14984=DIRECTION('',(0.750642243977328,-0.660708878067096,0.));
#14985=DIRECTION('',(0.,0.,1.));
#14986=DIRECTION('',(0.750642243977328,-0.660708878067096,0.));
#14987=DIRECTION('center_axis',(0.,0.,-1.));
#14988=DIRECTION('ref_axis',(-0.998755908557163,0.0498661721225458,0.));
#14989=DIRECTION('center_axis',(0.,0.,1.));
#14990=DIRECTION('ref_axis',(-0.998755908557163,0.0498661721225458,0.));
#14991=DIRECTION('',(0.,0.,-1.));
#14992=DIRECTION('center_axis',(0.,0.,-1.));
#14993=DIRECTION('ref_axis',(-0.998755908557163,0.0498661721225458,0.));
#14994=DIRECTION('',(0.,0.,1.));
#14995=DIRECTION('center_axis',(0.750642243977329,0.660708878067096,0.));
#14996=DIRECTION('ref_axis',(-0.660708878067096,0.750642243977329,0.));
#14997=DIRECTION('',(-0.660708878067096,0.750642243977329,0.));
#14998=DIRECTION('',(0.,0.,1.));
#14999=DIRECTION('',(0.660708878067096,-0.750642243977329,0.));
#15000=DIRECTION('center_axis',(0.,0.,1.));
#15001=DIRECTION('ref_axis',(0.261207001036715,0.965282809651869,0.));
#15002=DIRECTION('center_axis',(0.,0.,-1.));
#15003=DIRECTION('ref_axis',(0.261207001036715,0.965282809651869,0.));
#15004=DIRECTION('',(0.,0.,1.));
#15005=DIRECTION('center_axis',(0.,0.,1.));
#15006=DIRECTION('ref_axis',(0.261207001036715,0.965282809651869,0.));
#15007=DIRECTION('',(0.,0.,-1.));
#15008=DIRECTION('center_axis',(-0.860332693944512,-0.509732925883917,0.));
#15009=DIRECTION('ref_axis',(0.509732925883917,-0.860332693944512,0.));
#15010=DIRECTION('',(0.509732925883917,-0.860332693944512,0.));
#15011=DIRECTION('',(0.,0.,1.));
#15012=DIRECTION('',(0.509732925883917,-0.860332693944512,0.));
#15013=DIRECTION('center_axis',(0.,0.,-1.));
#15014=DIRECTION('ref_axis',(-0.934463820391288,0.356058096916388,0.));
#15015=DIRECTION('center_axis',(0.,0.,1.));
#15016=DIRECTION('ref_axis',(-0.934463820391288,0.356058096916388,0.));
#15017=DIRECTION('',(0.,0.,-1.));
#15018=DIRECTION('center_axis',(0.,0.,-1.));
#15019=DIRECTION('ref_axis',(-0.934463820391288,0.356058096916388,0.));
#15020=DIRECTION('',(0.,0.,1.));
#15021=DIRECTION('center_axis',(0.918073469198192,0.396410273775032,0.));
#15022=DIRECTION('ref_axis',(-0.396410273775032,0.918073469198192,0.));
#15023=DIRECTION('',(-0.396410273775032,0.918073469198192,0.));
#15024=DIRECTION('',(0.,0.,1.));
#15025=DIRECTION('',(0.396410273775032,-0.918073469198192,0.));
#15026=DIRECTION('center_axis',(0.,0.,1.));
#15027=DIRECTION('ref_axis',(0.546711412998308,0.837321103817044,0.));
#15028=DIRECTION('center_axis',(0.,0.,-1.));
#15029=DIRECTION('ref_axis',(0.546711412998308,0.837321103817044,0.));
#15030=DIRECTION('',(0.,0.,1.));
#15031=DIRECTION('center_axis',(0.,0.,1.));
#15032=DIRECTION('ref_axis',(0.546711412998308,0.837321103817044,0.));
#15033=DIRECTION('',(0.,0.,-1.));
#15034=DIRECTION('center_axis',(-0.975741151448288,-0.218927397486859,0.));
#15035=DIRECTION('ref_axis',(0.218927397486859,-0.975741151448288,0.));
#15036=DIRECTION('',(0.218927397486859,-0.975741151448288,0.));
#15037=DIRECTION('',(0.,0.,1.));
#15038=DIRECTION('',(0.218927397486859,-0.975741151448288,0.));
#15039=DIRECTION('center_axis',(0.,0.,-1.));
#15040=DIRECTION('ref_axis',(-0.778699902693228,0.627396574381433,0.));
#15041=DIRECTION('center_axis',(0.,0.,1.));
#15042=DIRECTION('ref_axis',(-0.778699902693228,0.627396574381433,0.));
#15043=DIRECTION('',(0.,0.,-1.));
#15044=DIRECTION('center_axis',(0.,0.,-1.));
#15045=DIRECTION('ref_axis',(-0.778699902693228,0.627396574381433,0.));
#15046=DIRECTION('',(0.,0.,1.));
#15047=DIRECTION('center_axis',(0.995637266659949,0.0933082699330834,0.));
#15048=DIRECTION('ref_axis',(-0.0933082699330834,0.995637266659949,0.));
#15049=DIRECTION('',(-0.0933082699330834,0.995637266659949,0.));
#15050=DIRECTION('',(0.,0.,1.));
#15051=DIRECTION('',(0.0933082699330834,-0.995637266659949,0.));
#15052=DIRECTION('center_axis',(0.,0.,1.));
#15053=DIRECTION('ref_axis',(0.778699902693227,0.627396574381435,0.));
#15054=DIRECTION('center_axis',(0.,0.,-1.));
#15055=DIRECTION('ref_axis',(0.778699902693227,0.627396574381435,0.));
#15056=DIRECTION('',(0.,0.,1.));
#15057=DIRECTION('center_axis',(0.,0.,1.));
#15058=DIRECTION('ref_axis',(0.778699902693227,0.627396574381435,0.));
#15059=DIRECTION('',(0.,0.,-1.));
#15060=DIRECTION('center_axis',(-0.995637266659949,0.0933082699330838,0.));
#15061=DIRECTION('ref_axis',(-0.0933082699330838,-0.995637266659949,0.));
#15062=DIRECTION('',(-0.0933082699330838,-0.995637266659949,0.));
#15063=DIRECTION('',(0.,0.,1.));
#15064=DIRECTION('',(-0.0933082699330838,-0.995637266659949,0.));
#15065=DIRECTION('center_axis',(0.,0.,-1.));
#15066=DIRECTION('ref_axis',(-0.546711412998307,0.837321103817045,0.));
#15067=DIRECTION('center_axis',(0.,0.,1.));
#15068=DIRECTION('ref_axis',(-0.546711412998307,0.837321103817045,0.));
#15069=DIRECTION('',(0.,0.,-1.));
#15070=DIRECTION('center_axis',(0.,0.,-1.));
#15071=DIRECTION('ref_axis',(-0.546711412998307,0.837321103817045,0.));
#15072=DIRECTION('',(0.,0.,1.));
#15073=DIRECTION('center_axis',(0.975741151448288,-0.21892739748686,0.));
#15074=DIRECTION('ref_axis',(0.21892739748686,0.975741151448288,0.));
#15075=DIRECTION('',(0.218927397486859,0.975741151448288,0.));
#15076=DIRECTION('',(0.,0.,1.));
#15077=DIRECTION('',(-0.218927397486859,-0.975741151448288,0.));
#15078=DIRECTION('center_axis',(0.,0.,1.));
#15079=DIRECTION('ref_axis',(0.934463820391285,0.356058096916394,0.));
#15080=DIRECTION('center_axis',(0.,0.,-1.));
#15081=DIRECTION('ref_axis',(0.934463820391285,0.356058096916394,0.));
#15082=DIRECTION('',(0.,0.,1.));
#15083=DIRECTION('center_axis',(0.,0.,1.));
#15084=DIRECTION('ref_axis',(0.934463820391285,0.356058096916394,0.));
#15085=DIRECTION('',(0.,0.,-1.));
#15086=DIRECTION('center_axis',(-0.918073469198192,0.396410273775032,0.));
#15087=DIRECTION('ref_axis',(-0.396410273775032,-0.918073469198192,0.));
#15088=DIRECTION('',(-0.396410273775032,-0.918073469198192,0.));
#15089=DIRECTION('',(0.,0.,1.));
#15090=DIRECTION('',(-0.396410273775032,-0.918073469198192,0.));
#15091=DIRECTION('center_axis',(0.,0.,-1.));
#15092=DIRECTION('ref_axis',(-0.261207001036714,0.965282809651869,0.));
#15093=DIRECTION('center_axis',(0.,0.,1.));
#15094=DIRECTION('ref_axis',(-0.261207001036714,0.965282809651869,0.));
#15095=DIRECTION('',(0.,0.,-1.));
#15096=DIRECTION('center_axis',(0.,0.,-1.));
#15097=DIRECTION('ref_axis',(-0.261207001036714,0.965282809651869,0.));
#15098=DIRECTION('',(0.,0.,1.));
#15099=DIRECTION('center_axis',(0.860332693944512,-0.509732925883917,0.));
#15100=DIRECTION('ref_axis',(0.509732925883917,0.860332693944512,0.));
#15101=DIRECTION('',(0.509732925883917,0.860332693944512,0.));
#15102=DIRECTION('',(0.,0.,1.));
#15103=DIRECTION('',(-0.509732925883917,-0.860332693944512,0.));
#15104=DIRECTION('center_axis',(0.,0.,1.));
#15105=DIRECTION('ref_axis',(0.998755908557164,0.0498661721225399,0.));
#15106=DIRECTION('center_axis',(0.,0.,-1.));
#15107=DIRECTION('ref_axis',(0.998755908557164,0.0498661721225399,0.));
#15108=DIRECTION('',(0.,0.,1.));
#15109=DIRECTION('center_axis',(0.,0.,1.));
#15110=DIRECTION('ref_axis',(0.998755908557164,0.0498661721225399,0.));
#15111=DIRECTION('',(0.,0.,-1.));
#15112=DIRECTION('center_axis',(-0.750642243977328,0.660708878067096,0.));
#15113=DIRECTION('ref_axis',(-0.660708878067096,-0.750642243977328,0.));
#15114=DIRECTION('',(-0.660708878067096,-0.750642243977328,0.));
#15115=DIRECTION('',(0.,0.,1.));
#15116=DIRECTION('',(-0.660708878067096,-0.750642243977328,0.));
#15117=DIRECTION('center_axis',(0.,0.,-1.));
#15118=DIRECTION('ref_axis',(0.0498661721225523,0.998755908557163,0.));
#15119=DIRECTION('center_axis',(0.,0.,1.));
#15120=DIRECTION('ref_axis',(0.0498661721225523,0.998755908557163,0.));
#15121=DIRECTION('',(0.,0.,-1.));
#15122=DIRECTION('center_axis',(0.,0.,-1.));
#15123=DIRECTION('ref_axis',(0.0498661721225523,0.998755908557163,0.));
#15124=DIRECTION('',(0.,0.,1.));
#15125=DIRECTION('center_axis',(0.660708878067096,-0.750642243977329,0.));
#15126=DIRECTION('ref_axis',(0.750642243977329,0.660708878067096,0.));
#15127=DIRECTION('',(0.750642243977329,0.660708878067096,0.));
#15128=DIRECTION('',(0.,0.,1.));
#15129=DIRECTION('',(-0.750642243977329,-0.660708878067096,0.));
#15130=DIRECTION('center_axis',(0.,0.,1.));
#15131=DIRECTION('ref_axis',(0.96528280965187,-0.261207001036712,0.));
#15132=DIRECTION('center_axis',(0.,0.,-1.));
#15133=DIRECTION('ref_axis',(0.96528280965187,-0.261207001036712,0.));
#15134=DIRECTION('',(0.,0.,1.));
#15135=DIRECTION('center_axis',(0.,0.,1.));
#15136=DIRECTION('ref_axis',(0.96528280965187,-0.261207001036712,0.));
#15137=DIRECTION('',(0.,0.,-1.));
#15138=DIRECTION('center_axis',(-0.509732925883917,0.860332693944512,0.));
#15139=DIRECTION('ref_axis',(-0.860332693944512,-0.509732925883917,0.));
#15140=DIRECTION('',(-0.860332693944512,-0.509732925883917,0.));
#15141=DIRECTION('',(0.,0.,1.));
#15142=DIRECTION('',(-0.860332693944512,-0.509732925883917,0.));
#15143=DIRECTION('center_axis',(0.,0.,-1.));
#15144=DIRECTION('ref_axis',(0.356058096916394,0.934463820391285,0.));
#15145=DIRECTION('center_axis',(0.,0.,1.));
#15146=DIRECTION('ref_axis',(0.356058096916394,0.934463820391285,0.));
#15147=DIRECTION('',(0.,0.,-1.));
#15148=DIRECTION('center_axis',(0.,0.,-1.));
#15149=DIRECTION('ref_axis',(0.356058096916394,0.934463820391285,0.));
#15150=DIRECTION('',(0.,0.,1.));
#15151=DIRECTION('center_axis',(0.396410273775032,-0.918073469198192,0.));
#15152=DIRECTION('ref_axis',(0.918073469198192,0.396410273775032,0.));
#15153=DIRECTION('',(0.918073469198192,0.396410273775032,0.));
#15154=DIRECTION('',(0.,0.,1.));
#15155=DIRECTION('',(-0.918073469198192,-0.396410273775032,0.));
#15156=DIRECTION('center_axis',(0.,0.,1.));
#15157=DIRECTION('ref_axis',(0.837321103817046,-0.546711412998306,0.));
#15158=DIRECTION('center_axis',(0.,0.,-1.));
#15159=DIRECTION('ref_axis',(0.837321103817046,-0.546711412998306,0.));
#15160=DIRECTION('',(0.,0.,1.));
#15161=DIRECTION('center_axis',(0.,0.,1.));
#15162=DIRECTION('ref_axis',(0.837321103817046,-0.546711412998306,0.));
#15163=DIRECTION('',(0.,0.,-1.));
#15164=DIRECTION('center_axis',(-0.218927397486859,0.975741151448288,0.));
#15165=DIRECTION('ref_axis',(-0.975741151448288,-0.218927397486859,0.));
#15166=DIRECTION('',(-0.975741151448288,-0.218927397486859,0.));
#15167=DIRECTION('',(0.,0.,1.));
#15168=DIRECTION('',(-0.975741151448288,-0.218927397486859,0.));
#15169=DIRECTION('center_axis',(0.,0.,-1.));
#15170=DIRECTION('ref_axis',(0.627396574381434,0.778699902693227,0.));
#15171=DIRECTION('center_axis',(0.,0.,1.));
#15172=DIRECTION('ref_axis',(0.627396574381434,0.778699902693227,0.));
#15173=DIRECTION('',(0.,0.,-1.));
#15174=DIRECTION('center_axis',(0.,0.,-1.));
#15175=DIRECTION('ref_axis',(0.627396574381434,0.778699902693227,0.));
#15176=DIRECTION('',(0.,0.,1.));
#15177=DIRECTION('center_axis',(0.0933082699330835,-0.995637266659949,0.));
#15178=DIRECTION('ref_axis',(0.995637266659949,0.0933082699330835,0.));
#15179=DIRECTION('',(0.995637266659949,0.0933082699330835,0.));
#15180=DIRECTION('',(0.,0.,1.));
#15181=DIRECTION('',(-0.995637266659949,-0.0933082699330835,0.));
#15182=DIRECTION('center_axis',(0.,0.,1.));
#15183=DIRECTION('ref_axis',(0.627396574381432,-0.778699902693229,0.));
#15184=DIRECTION('center_axis',(0.,0.,-1.));
#15185=DIRECTION('ref_axis',(0.627396574381432,-0.778699902693229,0.));
#15186=DIRECTION('',(0.,0.,1.));
#15187=DIRECTION('center_axis',(0.,0.,1.));
#15188=DIRECTION('ref_axis',(0.627396574381432,-0.778699902693229,0.));
#15189=DIRECTION('',(0.,0.,-1.));
#15190=DIRECTION('center_axis',(0.0933082699330838,0.995637266659949,0.));
#15191=DIRECTION('ref_axis',(-0.995637266659949,0.0933082699330838,0.));
#15192=DIRECTION('',(-0.995637266659949,0.0933082699330838,0.));
#15193=DIRECTION('',(0.,0.,1.));
#15194=DIRECTION('',(-0.995637266659949,0.0933082699330838,0.));
#15195=DIRECTION('center_axis',(0.,0.,-1.));
#15196=DIRECTION('ref_axis',(0.837321103817041,0.546711412998313,0.));
#15197=DIRECTION('center_axis',(0.,0.,1.));
#15198=DIRECTION('ref_axis',(0.837321103817041,0.546711412998313,0.));
#15199=DIRECTION('',(0.,0.,-1.));
#15200=DIRECTION('center_axis',(0.,0.,-1.));
#15201=DIRECTION('ref_axis',(0.837321103817041,0.546711412998313,0.));
#15202=DIRECTION('',(0.,0.,1.));
#15203=DIRECTION('center_axis',(-0.218927397486859,-0.975741151448288,0.));
#15204=DIRECTION('ref_axis',(0.975741151448288,-0.218927397486859,0.));
#15205=DIRECTION('',(0.975741151448288,-0.218927397486859,0.));
#15206=DIRECTION('',(0.,0.,1.));
#15207=DIRECTION('',(-0.975741151448288,0.218927397486859,0.));
#15208=DIRECTION('center_axis',(0.,0.,1.));
#15209=DIRECTION('ref_axis',(0.356058096916391,-0.934463820391286,0.));
#15210=DIRECTION('center_axis',(0.,0.,-1.));
#15211=DIRECTION('ref_axis',(0.356058096916391,-0.934463820391286,0.));
#15212=DIRECTION('',(0.,0.,1.));
#15213=DIRECTION('center_axis',(0.,0.,1.));
#15214=DIRECTION('ref_axis',(0.356058096916391,-0.934463820391286,0.));
#15215=DIRECTION('',(0.,0.,-1.));
#15216=DIRECTION('center_axis',(0.396410273775032,0.918073469198192,0.));
#15217=DIRECTION('ref_axis',(-0.918073469198192,0.396410273775032,0.));
#15218=DIRECTION('',(-0.918073469198192,0.396410273775032,0.));
#15219=DIRECTION('',(0.,0.,1.));
#15220=DIRECTION('',(-0.918073469198192,0.396410273775032,0.));
#15221=DIRECTION('center_axis',(0.,0.,-1.));
#15222=DIRECTION('ref_axis',(0.96528280965187,0.261207001036711,0.));
#15223=DIRECTION('center_axis',(0.,0.,1.));
#15224=DIRECTION('ref_axis',(0.96528280965187,0.261207001036711,0.));
#15225=DIRECTION('',(0.,0.,-1.));
#15226=DIRECTION('center_axis',(0.,0.,-1.));
#15227=DIRECTION('ref_axis',(0.96528280965187,0.261207001036711,0.));
#15228=DIRECTION('',(0.,0.,1.));
#15229=DIRECTION('center_axis',(-0.509732925883917,-0.860332693944512,0.));
#15230=DIRECTION('ref_axis',(0.860332693944512,-0.509732925883917,0.));
#15231=DIRECTION('',(0.860332693944512,-0.509732925883917,0.));
#15232=DIRECTION('',(0.,0.,1.));
#15233=DIRECTION('',(-0.860332693944512,0.509732925883917,0.));
#15234=DIRECTION('center_axis',(0.,0.,1.));
#15235=DIRECTION('ref_axis',(0.0498661721225523,-0.998755908557163,0.));
#15236=DIRECTION('center_axis',(0.,0.,-1.));
#15237=DIRECTION('ref_axis',(0.0498661721225523,-0.998755908557163,0.));
#15238=DIRECTION('',(0.,0.,1.));
#15239=DIRECTION('center_axis',(0.,0.,1.));
#15240=DIRECTION('ref_axis',(0.0498661721225523,-0.998755908557163,0.));
#15241=DIRECTION('',(0.,0.,-1.));
#15242=DIRECTION('center_axis',(0.660708878067096,0.750642243977328,0.));
#15243=DIRECTION('ref_axis',(-0.750642243977328,0.660708878067096,0.));
#15244=DIRECTION('',(-0.750642243977328,0.660708878067096,0.));
#15245=DIRECTION('',(0.,0.,1.));
#15246=DIRECTION('',(-0.750642243977328,0.660708878067096,0.));
#15247=DIRECTION('center_axis',(0.,0.,-1.));
#15248=DIRECTION('ref_axis',(0.998755908557164,-0.0498661721225396,0.));
#15249=DIRECTION('center_axis',(0.,0.,1.));
#15250=DIRECTION('ref_axis',(0.998755908557164,-0.0498661721225396,0.));
#15251=DIRECTION('',(0.,0.,-1.));
#15252=DIRECTION('center_axis',(0.,0.,-1.));
#15253=DIRECTION('ref_axis',(0.998755908557164,-0.0498661721225396,0.));
#15254=DIRECTION('',(0.,0.,1.));
#15255=DIRECTION('center_axis',(-0.750642243977329,-0.660708878067096,0.));
#15256=DIRECTION('ref_axis',(0.660708878067096,-0.750642243977329,0.));
#15257=DIRECTION('',(0.660708878067096,-0.750642243977329,0.));
#15258=DIRECTION('',(0.,0.,1.));
#15259=DIRECTION('',(-0.660708878067096,0.750642243977329,0.));
#15260=DIRECTION('center_axis',(0.,0.,1.));
#15261=DIRECTION('ref_axis',(-0.261207001036715,-0.965282809651869,0.));
#15262=DIRECTION('center_axis',(0.,0.,-1.));
#15263=DIRECTION('ref_axis',(-0.261207001036715,-0.965282809651869,0.));
#15264=DIRECTION('',(0.,0.,1.));
#15265=DIRECTION('center_axis',(0.,0.,1.));
#15266=DIRECTION('ref_axis',(-0.261207001036715,-0.965282809651869,0.));
#15267=DIRECTION('',(0.,0.,-1.));
#15268=DIRECTION('center_axis',(0.860332693944512,0.509732925883917,0.));
#15269=DIRECTION('ref_axis',(-0.509732925883917,0.860332693944512,0.));
#15270=DIRECTION('',(-0.509732925883917,0.860332693944512,0.));
#15271=DIRECTION('',(0.,0.,1.));
#15272=DIRECTION('',(-0.509732925883917,0.860332693944512,0.));
#15273=DIRECTION('center_axis',(0.,0.,-1.));
#15274=DIRECTION('ref_axis',(0.934463820391286,-0.356058096916392,0.));
#15275=DIRECTION('center_axis',(0.,0.,1.));
#15276=DIRECTION('ref_axis',(0.934463820391286,-0.356058096916392,0.));
#15277=DIRECTION('',(0.,0.,-1.));
#15278=DIRECTION('center_axis',(0.,0.,-1.));
#15279=DIRECTION('ref_axis',(0.934463820391286,-0.356058096916392,0.));
#15280=DIRECTION('',(0.,0.,1.));
#15281=DIRECTION('center_axis',(-0.918073469198192,-0.396410273775032,0.));
#15282=DIRECTION('ref_axis',(0.396410273775032,-0.918073469198192,0.));
#15283=DIRECTION('',(0.396410273775032,-0.918073469198192,0.));
#15284=DIRECTION('',(0.,0.,1.));
#15285=DIRECTION('',(-0.396410273775032,0.918073469198192,0.));
#15286=DIRECTION('center_axis',(0.,0.,1.));
#15287=DIRECTION('ref_axis',(-0.546711412998308,-0.837321103817044,0.));
#15288=DIRECTION('center_axis',(0.,0.,-1.));
#15289=DIRECTION('ref_axis',(-0.546711412998308,-0.837321103817044,0.));
#15290=DIRECTION('',(0.,0.,1.));
#15291=DIRECTION('center_axis',(0.,0.,1.));
#15292=DIRECTION('ref_axis',(-0.546711412998308,-0.837321103817044,0.));
#15293=DIRECTION('',(0.,0.,-1.));
#15294=DIRECTION('center_axis',(0.975741151448288,0.218927397486859,0.));
#15295=DIRECTION('ref_axis',(-0.218927397486859,0.975741151448288,0.));
#15296=DIRECTION('',(-0.218927397486859,0.975741151448288,0.));
#15297=DIRECTION('',(0.,0.,1.));
#15298=DIRECTION('',(-0.218927397486859,0.975741151448288,0.));
#15299=DIRECTION('center_axis',(0.,0.,-1.));
#15300=DIRECTION('ref_axis',(0.77869990269323,-0.627396574381431,0.));
#15301=DIRECTION('center_axis',(0.,0.,1.));
#15302=DIRECTION('ref_axis',(0.77869990269323,-0.627396574381431,0.));
#15303=DIRECTION('',(0.,0.,-1.));
#15304=DIRECTION('center_axis',(0.,0.,-1.));
#15305=DIRECTION('ref_axis',(0.77869990269323,-0.627396574381431,0.));
#15306=DIRECTION('',(0.,0.,1.));
#15307=DIRECTION('center_axis',(-0.995637266659949,-0.0933082699330835,
0.));
#15308=DIRECTION('ref_axis',(0.0933082699330835,-0.995637266659949,0.));
#15309=DIRECTION('',(0.0933082699330835,-0.995637266659949,0.));
#15310=DIRECTION('',(0.,0.,1.));
#15311=DIRECTION('',(-0.0933082699330835,0.995637266659949,0.));
#15312=DIRECTION('center_axis',(0.,0.,1.));
#15313=DIRECTION('ref_axis',(-0.77869990269323,-0.627396574381431,0.));
#15314=DIRECTION('center_axis',(0.,0.,-1.));
#15315=DIRECTION('ref_axis',(-0.77869990269323,-0.627396574381431,0.));
#15316=DIRECTION('',(0.,0.,1.));
#15317=DIRECTION('center_axis',(0.,0.,1.));
#15318=DIRECTION('ref_axis',(-0.77869990269323,-0.627396574381431,0.));
#15319=DIRECTION('',(0.,0.,-1.));
#15320=DIRECTION('center_axis',(0.995637266659949,-0.0933082699330837,0.));
#15321=DIRECTION('ref_axis',(0.0933082699330837,0.995637266659949,0.));
#15322=DIRECTION('',(0.0933082699330836,0.995637266659949,0.));
#15323=DIRECTION('',(0.,0.,1.));
#15324=DIRECTION('',(0.0933082699330836,0.995637266659949,0.));
#15325=DIRECTION('center_axis',(0.,0.,-1.));
#15326=DIRECTION('ref_axis',(0.546711412998308,-0.837321103817044,0.));
#15327=DIRECTION('center_axis',(0.,0.,1.));
#15328=DIRECTION('ref_axis',(0.546711412998308,-0.837321103817044,0.));
#15329=DIRECTION('',(0.,0.,-1.));
#15330=DIRECTION('center_axis',(0.,0.,-1.));
#15331=DIRECTION('ref_axis',(0.546711412998308,-0.837321103817044,0.));
#15332=DIRECTION('',(0.,0.,1.));
#15333=DIRECTION('center_axis',(-0.975741151448288,0.218927397486859,0.));
#15334=DIRECTION('ref_axis',(-0.218927397486859,-0.975741151448288,0.));
#15335=DIRECTION('',(-0.218927397486859,-0.975741151448288,0.));
#15336=DIRECTION('',(0.,0.,1.));
#15337=DIRECTION('',(0.218927397486859,0.975741151448288,0.));
#15338=DIRECTION('center_axis',(0.,0.,1.));
#15339=DIRECTION('ref_axis',(-0.934463820391285,-0.356058096916394,0.));
#15340=DIRECTION('center_axis',(0.,0.,-1.));
#15341=DIRECTION('ref_axis',(-0.934463820391285,-0.356058096916394,0.));
#15342=DIRECTION('',(0.,0.,1.));
#15343=DIRECTION('center_axis',(0.,0.,1.));
#15344=DIRECTION('ref_axis',(-0.934463820391285,-0.356058096916394,0.));
#15345=DIRECTION('',(0.,0.,-1.));
#15346=DIRECTION('center_axis',(0.918073469198192,-0.396410273775032,0.));
#15347=DIRECTION('ref_axis',(0.396410273775032,0.918073469198192,0.));
#15348=DIRECTION('',(0.396410273775032,0.918073469198192,0.));
#15349=DIRECTION('',(0.,0.,1.));
#15350=DIRECTION('',(0.396410273775032,0.918073469198192,0.));
#15351=DIRECTION('center_axis',(0.,0.,-1.));
#15352=DIRECTION('ref_axis',(0.261207001036715,-0.965282809651869,0.));
#15353=DIRECTION('center_axis',(0.,0.,1.));
#15354=DIRECTION('ref_axis',(0.261207001036715,-0.965282809651869,0.));
#15355=DIRECTION('',(0.,0.,-1.));
#15356=DIRECTION('center_axis',(0.,0.,-1.));
#15357=DIRECTION('ref_axis',(0.261207001036715,-0.965282809651869,0.));
#15358=DIRECTION('',(0.,0.,1.));
#15359=DIRECTION('center_axis',(-0.860332693944512,0.509732925883917,0.));
#15360=DIRECTION('ref_axis',(-0.509732925883917,-0.860332693944512,0.));
#15361=DIRECTION('',(-0.509732925883917,-0.860332693944512,0.));
#15362=DIRECTION('',(0.,0.,1.));
#15363=DIRECTION('',(0.509732925883917,0.860332693944512,0.));
#15364=DIRECTION('center_axis',(0.,0.,1.));
#15365=DIRECTION('ref_axis',(-0.998755908557164,-0.0498661721225396,0.));
#15366=DIRECTION('center_axis',(0.,0.,-1.));
#15367=DIRECTION('ref_axis',(-0.998755908557164,-0.0498661721225396,0.));
#15368=DIRECTION('',(0.,0.,1.));
#15369=DIRECTION('center_axis',(0.,0.,1.));
#15370=DIRECTION('ref_axis',(-0.998755908557164,-0.0498661721225396,0.));
#15371=DIRECTION('',(0.,0.,-1.));
#15372=DIRECTION('center_axis',(0.750642243977328,-0.660708878067096,0.));
#15373=DIRECTION('ref_axis',(0.660708878067096,0.750642243977328,0.));
#15374=DIRECTION('',(0.660708878067096,0.750642243977328,0.));
#15375=DIRECTION('',(0.,0.,1.));
#15376=DIRECTION('',(0.660708878067096,0.750642243977328,0.));
#15377=DIRECTION('center_axis',(0.,0.,-1.));
#15378=DIRECTION('ref_axis',(-0.0498661721225396,-0.998755908557164,0.));
#15379=DIRECTION('center_axis',(0.,0.,1.));
#15380=DIRECTION('ref_axis',(-0.0498661721225396,-0.998755908557164,0.));
#15381=DIRECTION('',(0.,0.,-1.));
#15382=DIRECTION('center_axis',(0.,0.,-1.));
#15383=DIRECTION('ref_axis',(-0.0498661721225396,-0.998755908557164,0.));
#15384=DIRECTION('',(0.,0.,1.));
#15385=DIRECTION('center_axis',(-0.660708878067096,0.750642243977328,0.));
#15386=DIRECTION('ref_axis',(-0.750642243977328,-0.660708878067096,0.));
#15387=DIRECTION('',(-0.750642243977328,-0.660708878067096,0.));
#15388=DIRECTION('',(0.,0.,1.));
#15389=DIRECTION('',(0.750642243977328,0.660708878067096,0.));
#15390=DIRECTION('center_axis',(0.,0.,1.));
#15391=DIRECTION('ref_axis',(-0.96528280965187,0.261207001036712,0.));
#15392=DIRECTION('center_axis',(0.,0.,-1.));
#15393=DIRECTION('ref_axis',(-0.96528280965187,0.261207001036712,0.));
#15394=DIRECTION('',(0.,0.,1.));
#15395=DIRECTION('center_axis',(0.,0.,1.));
#15396=DIRECTION('ref_axis',(-0.96528280965187,0.261207001036712,0.));
#15397=DIRECTION('',(0.,0.,-1.));
#15398=DIRECTION('center_axis',(0.509732925883917,-0.860332693944512,0.));
#15399=DIRECTION('ref_axis',(0.860332693944512,0.509732925883917,0.));
#15400=DIRECTION('',(0.860332693944512,0.509732925883917,0.));
#15401=DIRECTION('',(0.,0.,1.));
#15402=DIRECTION('',(0.860332693944512,0.509732925883917,0.));
#15403=DIRECTION('center_axis',(0.,0.,-1.));
#15404=DIRECTION('ref_axis',(-0.356058096916394,-0.934463820391285,0.));
#15405=DIRECTION('center_axis',(0.,0.,1.));
#15406=DIRECTION('ref_axis',(-0.356058096916394,-0.934463820391285,0.));
#15407=DIRECTION('',(0.,0.,-1.));
#15408=DIRECTION('center_axis',(0.,0.,-1.));
#15409=DIRECTION('ref_axis',(-0.356058096916394,-0.934463820391285,0.));
#15410=DIRECTION('',(0.,0.,1.));
#15411=DIRECTION('center_axis',(-0.396410273775032,0.918073469198192,0.));
#15412=DIRECTION('ref_axis',(-0.918073469198192,-0.396410273775032,0.));
#15413=DIRECTION('',(-0.918073469198192,-0.396410273775032,0.));
#15414=DIRECTION('',(0.,0.,1.));
#15415=DIRECTION('',(0.918073469198192,0.396410273775032,0.));
#15416=DIRECTION('center_axis',(0.,0.,1.));
#15417=DIRECTION('ref_axis',(-0.837321103817043,0.546711412998309,0.));
#15418=DIRECTION('center_axis',(0.,0.,-1.));
#15419=DIRECTION('ref_axis',(-0.837321103817043,0.546711412998309,0.));
#15420=DIRECTION('',(0.,0.,1.));
#15421=DIRECTION('center_axis',(0.,0.,1.));
#15422=DIRECTION('ref_axis',(-0.837321103817043,0.546711412998309,0.));
#15423=DIRECTION('',(0.,0.,-1.));
#15424=DIRECTION('center_axis',(0.218927397486859,-0.975741151448288,0.));
#15425=DIRECTION('ref_axis',(0.975741151448288,0.218927397486859,0.));
#15426=DIRECTION('',(0.975741151448288,0.218927397486859,0.));
#15427=DIRECTION('',(0.,0.,1.));
#15428=DIRECTION('',(0.975741151448288,0.218927397486859,0.));
#15429=DIRECTION('',(0.,0.,1.));
#15430=DIRECTION('center_axis',(0.,0.,1.));
#15431=DIRECTION('ref_axis',(0.940823330106451,-0.338897420361099,0.));
#15432=DIRECTION('center_axis',(0.,0.,1.));
#15433=DIRECTION('ref_axis',(0.940823330106451,-0.338897420361099,0.));
#15434=DIRECTION('center_axis',(0.,0.,1.));
#15435=DIRECTION('ref_axis',(0.940823330106451,-0.338897420361099,0.));
#15436=DIRECTION('',(0.,0.,1.));
#15437=DIRECTION('',(0.,0.,1.));
#15438=DIRECTION('center_axis',(0.,0.,1.));
#15439=DIRECTION('ref_axis',(0.790051096538837,-0.613040997697366,0.));
#15440=DIRECTION('center_axis',(0.,0.,1.));
#15441=DIRECTION('ref_axis',(0.790051096538837,-0.613040997697366,0.));
#15442=DIRECTION('center_axis',(0.,0.,1.));
#15443=DIRECTION('ref_axis',(0.790051096538837,-0.613040997697366,0.));
#15444=DIRECTION('',(0.,0.,1.));
#15445=DIRECTION('',(0.,0.,1.));
#15446=DIRECTION('center_axis',(0.,0.,1.));
#15447=DIRECTION('ref_axis',(0.561943157032333,-0.827175850871225,0.));
#15448=DIRECTION('center_axis',(0.,0.,1.));
#15449=DIRECTION('ref_axis',(0.561943157032333,-0.827175850871225,0.));
#15450=DIRECTION('center_axis',(0.,0.,1.));
#15451=DIRECTION('ref_axis',(0.561943157032333,-0.827175850871225,0.));
#15452=DIRECTION('',(0.,0.,1.));
#15453=DIRECTION('',(0.,0.,1.));
#15454=DIRECTION('center_axis',(0.,0.,1.));
#15455=DIRECTION('ref_axis',(0.278828306027306,-0.960340968488767,0.));
#15456=DIRECTION('center_axis',(0.,0.,1.));
#15457=DIRECTION('ref_axis',(0.278828306027306,-0.960340968488767,0.));
#15458=DIRECTION('center_axis',(0.,0.,1.));
#15459=DIRECTION('ref_axis',(0.278828306027306,-0.960340968488767,0.));
#15460=DIRECTION('',(0.,0.,1.));
#15461=DIRECTION('',(0.,0.,1.));
#15462=DIRECTION('center_axis',(0.,0.,1.));
#15463=DIRECTION('ref_axis',(-0.0315802022827165,-0.999501221021657,0.));
#15464=DIRECTION('center_axis',(0.,0.,1.));
#15465=DIRECTION('ref_axis',(-0.0315802022827165,-0.999501221021657,0.));
#15466=DIRECTION('center_axis',(0.,0.,1.));
#15467=DIRECTION('ref_axis',(-0.0315802022827165,-0.999501221021657,0.));
#15468=DIRECTION('',(0.,0.,1.));
#15469=DIRECTION('',(0.,0.,1.));
#15470=DIRECTION('center_axis',(0.,0.,1.));
#15471=DIRECTION('ref_axis',(-0.338897420361099,-0.940823330106451,0.));
#15472=DIRECTION('center_axis',(0.,0.,1.));
#15473=DIRECTION('ref_axis',(-0.338897420361099,-0.940823330106451,0.));
#15474=DIRECTION('center_axis',(0.,0.,1.));
#15475=DIRECTION('ref_axis',(-0.338897420361099,-0.940823330106451,0.));
#15476=DIRECTION('',(0.,0.,1.));
#15477=DIRECTION('',(0.,0.,1.));
#15478=DIRECTION('center_axis',(0.,0.,1.));
#15479=DIRECTION('ref_axis',(-0.613040997697366,-0.790051096538837,0.));
#15480=DIRECTION('center_axis',(0.,0.,1.));
#15481=DIRECTION('ref_axis',(-0.613040997697366,-0.790051096538837,0.));
#15482=DIRECTION('center_axis',(0.,0.,1.));
#15483=DIRECTION('ref_axis',(-0.613040997697366,-0.790051096538837,0.));
#15484=DIRECTION('',(0.,0.,1.));
#15485=DIRECTION('',(0.,0.,1.));
#15486=DIRECTION('center_axis',(0.,0.,1.));
#15487=DIRECTION('ref_axis',(-0.827175850871225,-0.561943157032333,0.));
#15488=DIRECTION('center_axis',(0.,0.,1.));
#15489=DIRECTION('ref_axis',(-0.827175850871225,-0.561943157032333,0.));
#15490=DIRECTION('center_axis',(0.,0.,1.));
#15491=DIRECTION('ref_axis',(-0.827175850871225,-0.561943157032333,0.));
#15492=DIRECTION('',(0.,0.,1.));
#15493=DIRECTION('',(0.,0.,1.));
#15494=DIRECTION('center_axis',(0.,0.,1.));
#15495=DIRECTION('ref_axis',(-0.960340968488767,-0.278828306027306,0.));
#15496=DIRECTION('center_axis',(0.,0.,1.));
#15497=DIRECTION('ref_axis',(-0.960340968488767,-0.278828306027306,0.));
#15498=DIRECTION('center_axis',(0.,0.,1.));
#15499=DIRECTION('ref_axis',(-0.960340968488767,-0.278828306027306,0.));
#15500=DIRECTION('',(0.,0.,1.));
#15501=DIRECTION('',(0.,0.,1.));
#15502=DIRECTION('center_axis',(0.,0.,1.));
#15503=DIRECTION('ref_axis',(-0.999501221021657,0.0315802022827165,0.));
#15504=DIRECTION('center_axis',(0.,0.,1.));
#15505=DIRECTION('ref_axis',(-0.999501221021657,0.0315802022827165,0.));
#15506=DIRECTION('center_axis',(0.,0.,1.));
#15507=DIRECTION('ref_axis',(-0.999501221021657,0.0315802022827165,0.));
#15508=DIRECTION('',(0.,0.,1.));
#15509=DIRECTION('',(0.,0.,1.));
#15510=DIRECTION('center_axis',(0.,0.,1.));
#15511=DIRECTION('ref_axis',(-0.940823330106451,0.338897420361099,0.));
#15512=DIRECTION('center_axis',(0.,0.,1.));
#15513=DIRECTION('ref_axis',(-0.940823330106451,0.338897420361099,0.));
#15514=DIRECTION('center_axis',(0.,0.,1.));
#15515=DIRECTION('ref_axis',(-0.940823330106451,0.338897420361099,0.));
#15516=DIRECTION('',(0.,0.,1.));
#15517=DIRECTION('',(0.,0.,1.));
#15518=DIRECTION('center_axis',(0.,0.,1.));
#15519=DIRECTION('ref_axis',(-0.790051096538837,0.613040997697366,0.));
#15520=DIRECTION('center_axis',(0.,0.,1.));
#15521=DIRECTION('ref_axis',(-0.790051096538837,0.613040997697366,0.));
#15522=DIRECTION('center_axis',(0.,0.,1.));
#15523=DIRECTION('ref_axis',(-0.790051096538837,0.613040997697366,0.));
#15524=DIRECTION('',(0.,0.,1.));
#15525=DIRECTION('',(0.,0.,1.));
#15526=DIRECTION('center_axis',(0.,0.,1.));
#15527=DIRECTION('ref_axis',(-0.561943157032333,0.827175850871225,0.));
#15528=DIRECTION('center_axis',(0.,0.,1.));
#15529=DIRECTION('ref_axis',(-0.561943157032333,0.827175850871225,0.));
#15530=DIRECTION('center_axis',(0.,0.,1.));
#15531=DIRECTION('ref_axis',(-0.561943157032333,0.827175850871225,0.));
#15532=DIRECTION('',(0.,0.,1.));
#15533=DIRECTION('',(0.,0.,1.));
#15534=DIRECTION('center_axis',(0.,0.,1.));
#15535=DIRECTION('ref_axis',(-0.278828306027306,0.960340968488767,0.));
#15536=DIRECTION('center_axis',(0.,0.,1.));
#15537=DIRECTION('ref_axis',(-0.278828306027306,0.960340968488767,0.));
#15538=DIRECTION('center_axis',(0.,0.,1.));
#15539=DIRECTION('ref_axis',(-0.278828306027306,0.960340968488767,0.));
#15540=DIRECTION('',(0.,0.,1.));
#15541=DIRECTION('',(0.,0.,1.));
#15542=DIRECTION('center_axis',(0.,0.,1.));
#15543=DIRECTION('ref_axis',(0.0315802022827164,0.999501221021657,0.));
#15544=DIRECTION('center_axis',(0.,0.,1.));
#15545=DIRECTION('ref_axis',(0.0315802022827164,0.999501221021657,0.));
#15546=DIRECTION('center_axis',(0.,0.,1.));
#15547=DIRECTION('ref_axis',(0.0315802022827164,0.999501221021657,0.));
#15548=DIRECTION('',(0.,0.,1.));
#15549=DIRECTION('',(0.,0.,1.));
#15550=DIRECTION('center_axis',(0.,0.,1.));
#15551=DIRECTION('ref_axis',(0.338897420361099,0.940823330106451,0.));
#15552=DIRECTION('center_axis',(0.,0.,1.));
#15553=DIRECTION('ref_axis',(0.338897420361099,0.940823330106451,0.));
#15554=DIRECTION('center_axis',(0.,0.,1.));
#15555=DIRECTION('ref_axis',(0.338897420361099,0.940823330106451,0.));
#15556=DIRECTION('',(0.,0.,1.));
#15557=DIRECTION('',(0.,0.,1.));
#15558=DIRECTION('center_axis',(0.,0.,1.));
#15559=DIRECTION('ref_axis',(0.613040997697366,0.790051096538837,0.));
#15560=DIRECTION('center_axis',(0.,0.,1.));
#15561=DIRECTION('ref_axis',(0.613040997697366,0.790051096538837,0.));
#15562=DIRECTION('center_axis',(0.,0.,1.));
#15563=DIRECTION('ref_axis',(0.613040997697366,0.790051096538837,0.));
#15564=DIRECTION('',(0.,0.,1.));
#15565=DIRECTION('',(0.,0.,1.));
#15566=DIRECTION('center_axis',(0.,0.,1.));
#15567=DIRECTION('ref_axis',(0.827175850871225,0.561943157032333,0.));
#15568=DIRECTION('center_axis',(0.,0.,1.));
#15569=DIRECTION('ref_axis',(0.827175850871225,0.561943157032333,0.));
#15570=DIRECTION('center_axis',(0.,0.,1.));
#15571=DIRECTION('ref_axis',(0.827175850871225,0.561943157032333,0.));
#15572=DIRECTION('',(0.,0.,1.));
#15573=DIRECTION('',(0.,0.,1.));
#15574=DIRECTION('center_axis',(0.,0.,1.));
#15575=DIRECTION('ref_axis',(0.960340968488767,0.278828306027306,0.));
#15576=DIRECTION('center_axis',(0.,0.,1.));
#15577=DIRECTION('ref_axis',(0.960340968488767,0.278828306027306,0.));
#15578=DIRECTION('center_axis',(0.,0.,1.));
#15579=DIRECTION('ref_axis',(0.960340968488767,0.278828306027306,0.));
#15580=DIRECTION('',(0.,0.,1.));
#15581=DIRECTION('center_axis',(0.,0.,1.));
#15582=DIRECTION('ref_axis',(1.,0.,0.));
#15583=DIRECTION('center_axis',(0.,0.,1.));
#15584=DIRECTION('ref_axis',(1.,0.,0.));
#15585=DIRECTION('center_axis',(0.,0.,1.));
#15586=DIRECTION('ref_axis',(1.,0.,0.));
#15587=DIRECTION('center_axis',(0.,0.,1.));
#15588=DIRECTION('ref_axis',(1.,0.,0.));
#15589=DIRECTION('center_axis',(0.,0.,1.));
#15590=DIRECTION('ref_axis',(1.,0.,0.));
#15591=DIRECTION('center_axis',(0.,0.,1.));
#15592=DIRECTION('ref_axis',(1.,0.,0.));
#15593=DIRECTION('center_axis',(0.,0.,1.));
#15594=DIRECTION('ref_axis',(1.,0.,0.));
#15595=DIRECTION('center_axis',(0.,0.,1.));
#15596=DIRECTION('ref_axis',(1.,0.,0.));
#15597=DIRECTION('center_axis',(0.,0.,1.));
#15598=DIRECTION('ref_axis',(1.,0.,0.));
#15599=DIRECTION('center_axis',(0.,0.,1.));
#15600=DIRECTION('ref_axis',(1.,0.,0.));
#15601=DIRECTION('center_axis',(0.,0.,1.));
#15602=DIRECTION('ref_axis',(1.,0.,0.));
#15603=DIRECTION('center_axis',(0.,0.,1.));
#15604=DIRECTION('ref_axis',(1.,0.,0.));
#15605=DIRECTION('center_axis',(0.,0.,1.));
#15606=DIRECTION('ref_axis',(1.,0.,0.));
#15607=DIRECTION('center_axis',(0.,0.,1.));
#15608=DIRECTION('ref_axis',(1.,0.,0.));
#15609=DIRECTION('center_axis',(0.,0.,1.));
#15610=DIRECTION('ref_axis',(1.,0.,0.));
#15611=DIRECTION('center_axis',(0.,0.,1.));
#15612=DIRECTION('ref_axis',(1.,0.,0.));
#15613=DIRECTION('center_axis',(0.,0.,1.));
#15614=DIRECTION('ref_axis',(1.,0.,0.));
#15615=DIRECTION('center_axis',(0.,0.,1.));
#15616=DIRECTION('ref_axis',(1.,0.,0.));
#15617=DIRECTION('center_axis',(0.,0.,1.));
#15618=DIRECTION('ref_axis',(1.,0.,0.));
#15619=DIRECTION('center_axis',(0.,0.,-1.));
#15620=DIRECTION('ref_axis',(-0.627396574381432,-0.778699902693229,0.));
#15621=DIRECTION('',(0.995637266659949,0.0933082699330836,0.));
#15622=DIRECTION('center_axis',(0.,0.,1.));
#15623=DIRECTION('ref_axis',(0.999501221021657,-0.0315802022827163,0.));
#15624=DIRECTION('',(0.995637266659949,-0.0933082699330836,0.));
#15625=DIRECTION('center_axis',(0.,0.,-1.));
#15626=DIRECTION('ref_axis',(-0.627396574381432,0.778699902693229,0.));
#15627=DIRECTION('center_axis',(0.,0.,1.));
#15628=DIRECTION('ref_axis',(1.,0.,0.));
#15629=DIRECTION('center_axis',(0.,0.,1.));
#15630=DIRECTION('ref_axis',(1.,0.,0.));
#15631=DIRECTION('center_axis',(0.,0.,1.));
#15632=DIRECTION('ref_axis',(1.,0.,0.));
#15633=DIRECTION('center_axis',(0.,0.,1.));
#15634=DIRECTION('ref_axis',(1.,0.,0.));
#15635=DIRECTION('center_axis',(0.,0.,1.));
#15636=DIRECTION('ref_axis',(-0.627396574381432,0.778699902693229,0.));
#15637=DIRECTION('',(0.995637266659949,-0.0933082699330836,0.));
#15638=DIRECTION('center_axis',(0.,0.,1.));
#15639=DIRECTION('ref_axis',(0.999501221021657,-0.0315802022827163,0.));
#15640=DIRECTION('',(-0.995637266659949,-0.0933082699330836,0.));
#15641=DIRECTION('center_axis',(0.,0.,1.));
#15642=DIRECTION('ref_axis',(-0.627396574381432,-0.778699902693229,0.));
#15643=DIRECTION('center_axis',(0.,0.,1.));
#15644=DIRECTION('ref_axis',(1.,0.,0.));
#15645=DIRECTION('center_axis',(0.,0.,1.));
#15646=DIRECTION('ref_axis',(1.,0.,0.));
#15647=DIRECTION('center_axis',(0.,0.,1.));
#15648=DIRECTION('ref_axis',(1.,0.,0.));
#15649=DIRECTION('center_axis',(0.,0.,1.));
#15650=DIRECTION('ref_axis',(1.,0.,0.));
#15651=DIRECTION('center_axis',(0.,0.,1.));
#15652=DIRECTION('ref_axis',(1.,0.,0.));
#15653=DIRECTION('center_axis',(0.,0.,1.));
#15654=DIRECTION('ref_axis',(1.,0.,0.));
#15655=DIRECTION('center_axis',(0.,0.,1.));
#15656=DIRECTION('ref_axis',(1.,0.,0.));
#15657=DIRECTION('center_axis',(0.,0.,1.));
#15658=DIRECTION('ref_axis',(1.,0.,0.));
#15659=DIRECTION('center_axis',(0.,0.,1.));
#15660=DIRECTION('ref_axis',(1.,0.,0.));
#15661=DIRECTION('center_axis',(0.,0.,1.));
#15662=DIRECTION('ref_axis',(1.,0.,0.));
#15663=DIRECTION('center_axis',(0.,0.,1.));
#15664=DIRECTION('ref_axis',(1.,0.,0.));
#15665=DIRECTION('center_axis',(0.,0.,1.));
#15666=DIRECTION('ref_axis',(1.,0.,0.));
#15667=DIRECTION('center_axis',(0.,0.,1.));
#15668=DIRECTION('ref_axis',(1.,0.,0.));
#15669=DIRECTION('center_axis',(0.,0.,1.));
#15670=DIRECTION('ref_axis',(1.,0.,0.));
#15671=DIRECTION('center_axis',(0.,0.,1.));
#15672=DIRECTION('ref_axis',(1.,0.,0.));
#15673=DIRECTION('center_axis',(0.,0.,1.));
#15674=DIRECTION('ref_axis',(1.,0.,0.));
#15675=DIRECTION('center_axis',(0.,0.,1.));
#15676=DIRECTION('ref_axis',(1.,0.,0.));
#15677=DIRECTION('center_axis',(0.,0.,1.));
#15678=DIRECTION('ref_axis',(1.,0.,0.));
#15679=DIRECTION('center_axis',(0.,0.,1.));
#15680=DIRECTION('ref_axis',(1.,0.,0.));
#15681=DIRECTION('center_axis',(0.,0.,1.));
#15682=DIRECTION('ref_axis',(1.,0.,0.));
#15683=DIRECTION('',(0.,0.,1.));
#15684=DIRECTION('center_axis',(0.,0.,1.));
#15685=DIRECTION('ref_axis',(1.,0.,0.));
#15686=DIRECTION('center_axis',(0.,0.,1.));
#15687=DIRECTION('ref_axis',(1.,0.,0.));
#15688=DIRECTION('center_axis',(0.,0.,1.));
#15689=DIRECTION('ref_axis',(1.,0.,0.));
#15690=DIRECTION('center_axis',(0.,0.,1.));
#15691=DIRECTION('ref_axis',(1.,0.,0.));
#15692=DIRECTION('center_axis',(0.,0.,1.));
#15693=DIRECTION('ref_axis',(1.,0.,0.));
#15694=DIRECTION('center_axis',(0.,0.,1.));
#15695=DIRECTION('ref_axis',(1.,0.,0.));
#15696=DIRECTION('center_axis',(0.,0.,1.));
#15697=DIRECTION('ref_axis',(1.,0.,0.));
#15698=DIRECTION('center_axis',(0.,0.,1.));
#15699=DIRECTION('ref_axis',(1.,0.,0.));
#15700=DIRECTION('center_axis',(0.,0.,1.));
#15701=DIRECTION('ref_axis',(1.,0.,0.));
#15702=DIRECTION('center_axis',(0.,0.,1.));
#15703=DIRECTION('ref_axis',(1.,0.,0.));
#15704=DIRECTION('center_axis',(0.,0.,1.));
#15705=DIRECTION('ref_axis',(1.,0.,0.));
#15706=DIRECTION('center_axis',(0.,0.,1.));
#15707=DIRECTION('ref_axis',(1.,0.,0.));
#15708=DIRECTION('center_axis',(0.,0.,1.));
#15709=DIRECTION('ref_axis',(1.,0.,0.));
#15710=DIRECTION('center_axis',(0.,0.,1.));
#15711=DIRECTION('ref_axis',(1.,0.,0.));
#15712=DIRECTION('center_axis',(0.,0.,1.));
#15713=DIRECTION('ref_axis',(1.,0.,0.));
#15714=DIRECTION('center_axis',(0.,0.,1.));
#15715=DIRECTION('ref_axis',(1.,0.,0.));
#15716=DIRECTION('center_axis',(0.,0.,1.));
#15717=DIRECTION('ref_axis',(1.,0.,0.));
#15718=DIRECTION('center_axis',(0.,0.,1.));
#15719=DIRECTION('ref_axis',(1.,0.,0.));
#15720=DIRECTION('center_axis',(0.,0.,-1.));
#15721=DIRECTION('ref_axis',(-0.627396574381432,-0.778699902693229,0.));
#15722=DIRECTION('',(0.,0.,-1.));
#15723=DIRECTION('center_axis',(-0.0933082699330836,0.995637266659949,0.));
#15724=DIRECTION('ref_axis',(-0.995637266659949,-0.0933082699330836,0.));
#15725=DIRECTION('',(0.,0.,1.));
#15726=DIRECTION('center_axis',(0.,0.,1.));
#15727=DIRECTION('ref_axis',(-0.627396574381432,0.778699902693229,0.));
#15728=DIRECTION('',(0.,0.,1.));
#15729=DIRECTION('',(0.,0.,-1.));
#15730=DIRECTION('center_axis',(-0.0933082699330836,-0.995637266659949,
0.));
#15731=DIRECTION('ref_axis',(0.995637266659949,-0.0933082699330836,0.));
#15732=DIRECTION('',(0.,0.,1.));
#15733=DIRECTION('',(0.,0.,1.));
#15734=DIRECTION('center_axis',(0.,0.,1.));
#15735=DIRECTION('ref_axis',(0.999501221021657,-0.0315802022827163,0.));
#15736=DIRECTION('',(0.,0.,1.));
#15737=DIRECTION('center_axis',(0.,0.,1.));
#15738=DIRECTION('ref_axis',(1.,0.,0.));
#15739=DIRECTION('axis',(0.,0.,1.));
#15740=DIRECTION('refdir',(1.,0.,0.));
#15741=DIRECTION('center_axis',(0.,9.02056207507939E-16,-1.));
#15742=DIRECTION('ref_axis',(1.,0.,0.));
#15743=DIRECTION('center_axis',(0.,8.7430063189231E-16,-1.));
#15744=DIRECTION('ref_axis',(1.,0.,0.));
#15745=DIRECTION('',(0.,-9.02056207507939E-16,1.));
#15746=DIRECTION('center_axis',(0.,8.7430063189231E-16,-1.));
#15747=DIRECTION('ref_axis',(1.,0.,0.));
#15748=DIRECTION('center_axis',(0.,9.02056207507939E-16,-1.));
#15749=DIRECTION('ref_axis',(1.,0.,0.));
#15750=DIRECTION('center_axis',(0.,8.7430063189231E-16,-1.));
#15751=DIRECTION('ref_axis',(1.,0.,0.));
#15752=DIRECTION('',(0.,-9.02056207507939E-16,1.));
#15753=DIRECTION('center_axis',(0.,-8.7430063189231E-16,1.));
#15754=DIRECTION('ref_axis',(1.,0.,0.));
#15755=DIRECTION('center_axis',(0.,8.7430063189231E-16,-1.));
#15756=DIRECTION('ref_axis',(1.,0.,0.));
#15757=DIRECTION('center_axis',(0.,8.7430063189231E-16,-1.));
#15758=DIRECTION('ref_axis',(1.,0.,0.));
#15759=DIRECTION('center_axis',(0.,0.,-1.));
#15760=DIRECTION('ref_axis',(-0.936029699362847,-0.351921016579996,0.));
#15761=DIRECTION('center_axis',(0.,0.,1.));
#15762=DIRECTION('ref_axis',(-0.936029699362847,-0.351921016579996,0.));
#15763=DIRECTION('',(0.,0.,-1.));
#15764=DIRECTION('center_axis',(0.,0.,-1.));
#15765=DIRECTION('ref_axis',(-0.936029699362847,-0.351921016579996,0.));
#15766=DIRECTION('',(0.,0.,1.));
#15767=DIRECTION('center_axis',(0.440660664196194,0.897673759798163,0.));
#15768=DIRECTION('ref_axis',(-0.897673759798163,0.440660664196194,0.));
#15769=DIRECTION('',(-0.897673759798163,0.440660664196194,0.));
#15770=DIRECTION('',(0.,0.,1.));
#15771=DIRECTION('',(0.897673759798163,-0.440660664196194,0.));
#15772=DIRECTION('center_axis',(0.,0.,1.));
#15773=DIRECTION('ref_axis',(0.0454476916968278,0.998966719825756,0.));
#15774=DIRECTION('center_axis',(0.,0.,-1.));
#15775=DIRECTION('ref_axis',(0.0454476916968278,0.998966719825756,0.));
#15776=DIRECTION('',(0.,0.,1.));
#15777=DIRECTION('center_axis',(0.,0.,1.));
#15778=DIRECTION('ref_axis',(0.0454476916968278,0.998966719825756,0.));
#15779=DIRECTION('',(0.,0.,-1.));
#15780=DIRECTION('center_axis',(-0.717566844774038,-0.696489643340827,0.));
#15781=DIRECTION('ref_axis',(0.696489643340827,-0.717566844774038,0.));
#15782=DIRECTION('',(0.696489643340827,-0.717566844774038,0.));
#15783=DIRECTION('',(0.,0.,1.));
#15784=DIRECTION('',(0.696489643340827,-0.717566844774038,0.));
#15785=DIRECTION('center_axis',(0.,0.,-1.));
#15786=DIRECTION('ref_axis',(-0.964117917541714,0.265474369902311,0.));
#15787=DIRECTION('center_axis',(0.,0.,1.));
#15788=DIRECTION('ref_axis',(-0.964117917541714,0.265474369902311,0.));
#15789=DIRECTION('',(0.,0.,-1.));
#15790=DIRECTION('center_axis',(0.,0.,-1.));
#15791=DIRECTION('ref_axis',(-0.964117917541714,0.265474369902311,0.));
#15792=DIRECTION('',(0.,0.,1.));
#15793=DIRECTION('center_axis',(0.884141363466569,0.46721948740124,0.));
#15794=DIRECTION('ref_axis',(-0.46721948740124,0.884141363466569,0.));
#15795=DIRECTION('',(-0.46721948740124,0.884141363466569,0.));
#15796=DIRECTION('',(0.,0.,1.));
#15797=DIRECTION('',(0.46721948740124,-0.884141363466569,0.));
#15798=DIRECTION('center_axis',(0.,0.,1.));
#15799=DIRECTION('ref_axis',(0.623945860382415,0.781467570223901,0.));
#15800=DIRECTION('center_axis',(0.,0.,-1.));
#15801=DIRECTION('ref_axis',(0.623945860382415,0.781467570223901,0.));
#15802=DIRECTION('',(0.,0.,1.));
#15803=DIRECTION('center_axis',(0.,0.,1.));
#15804=DIRECTION('ref_axis',(0.623945860382415,0.781467570223901,0.));
#15805=DIRECTION('',(0.,0.,-1.));
#15806=DIRECTION('center_axis',(-0.989910112752389,-0.141696748976653,0.));
#15807=DIRECTION('ref_axis',(0.141696748976653,-0.989910112752389,0.));
#15808=DIRECTION('',(0.141696748976653,-0.989910112752389,0.));
#15809=DIRECTION('',(0.,0.,1.));
#15810=DIRECTION('',(0.141696748976653,-0.989910112752389,0.));
#15811=DIRECTION('center_axis',(0.,0.,-1.));
#15812=DIRECTION('ref_axis',(-0.623945860382415,0.781467570223901,0.));
#15813=DIRECTION('center_axis',(0.,0.,1.));
#15814=DIRECTION('ref_axis',(-0.623945860382415,0.781467570223901,0.));
#15815=DIRECTION('',(0.,0.,-1.));
#15816=DIRECTION('center_axis',(0.,0.,-1.));
#15817=DIRECTION('ref_axis',(-0.623945860382415,0.781467570223901,0.));
#15818=DIRECTION('',(0.,0.,1.));
#15819=DIRECTION('center_axis',(0.989910112752389,-0.141696748976654,0.));
#15820=DIRECTION('ref_axis',(0.141696748976654,0.989910112752389,0.));
#15821=DIRECTION('',(0.141696748976654,0.989910112752389,0.));
#15822=DIRECTION('',(0.,0.,1.));
#15823=DIRECTION('',(-0.141696748976654,-0.989910112752389,0.));
#15824=DIRECTION('center_axis',(0.,0.,1.));
#15825=DIRECTION('ref_axis',(0.964117917541713,0.265474369902315,0.));
#15826=DIRECTION('center_axis',(0.,0.,-1.));
#15827=DIRECTION('ref_axis',(0.964117917541713,0.265474369902315,0.));
#15828=DIRECTION('',(0.,0.,1.));
#15829=DIRECTION('center_axis',(0.,0.,1.));
#15830=DIRECTION('ref_axis',(0.964117917541713,0.265474369902315,0.));
#15831=DIRECTION('',(0.,0.,-1.));
#15832=DIRECTION('center_axis',(-0.884141363466568,0.46721948740124,0.));
#15833=DIRECTION('ref_axis',(-0.46721948740124,-0.884141363466568,0.));
#15834=DIRECTION('',(-0.46721948740124,-0.884141363466568,0.));
#15835=DIRECTION('',(0.,0.,1.));
#15836=DIRECTION('',(-0.46721948740124,-0.884141363466568,0.));
#15837=DIRECTION('center_axis',(0.,0.,-1.));
#15838=DIRECTION('ref_axis',(-0.0454476916968278,0.998966719825756,0.));
#15839=DIRECTION('center_axis',(0.,0.,1.));
#15840=DIRECTION('ref_axis',(-0.0454476916968278,0.998966719825756,0.));
#15841=DIRECTION('',(0.,0.,-1.));
#15842=DIRECTION('center_axis',(0.,0.,-1.));
#15843=DIRECTION('ref_axis',(-0.0454476916968278,0.998966719825756,0.));
#15844=DIRECTION('',(0.,0.,1.));
#15845=DIRECTION('center_axis',(0.717566844774037,-0.696489643340827,0.));
#15846=DIRECTION('ref_axis',(0.696489643340827,0.717566844774037,0.));
#15847=DIRECTION('',(0.696489643340827,0.717566844774037,0.));
#15848=DIRECTION('',(0.,0.,1.));
#15849=DIRECTION('',(-0.696489643340827,-0.717566844774037,0.));
#15850=DIRECTION('center_axis',(0.,0.,1.));
#15851=DIRECTION('ref_axis',(0.936029699362847,-0.351921016579998,0.));
#15852=DIRECTION('center_axis',(0.,0.,-1.));
#15853=DIRECTION('ref_axis',(0.936029699362847,-0.351921016579998,0.));
#15854=DIRECTION('',(0.,0.,1.));
#15855=DIRECTION('center_axis',(0.,0.,1.));
#15856=DIRECTION('ref_axis',(0.936029699362847,-0.351921016579998,0.));
#15857=DIRECTION('',(0.,0.,-1.));
#15858=DIRECTION('center_axis',(-0.440660664196193,0.897673759798163,0.));
#15859=DIRECTION('ref_axis',(-0.897673759798163,-0.440660664196193,0.));
#15860=DIRECTION('',(-0.897673759798163,-0.440660664196193,0.));
#15861=DIRECTION('',(0.,0.,1.));
#15862=DIRECTION('',(-0.897673759798163,-0.440660664196193,0.));
#15863=DIRECTION('center_axis',(0.,0.,-1.));
#15864=DIRECTION('ref_axis',(0.550409950506719,0.834894536084164,0.));
#15865=DIRECTION('center_axis',(0.,0.,1.));
#15866=DIRECTION('ref_axis',(0.550409950506719,0.834894536084164,0.));
#15867=DIRECTION('',(0.,0.,-1.));
#15868=DIRECTION('center_axis',(0.,0.,-1.));
#15869=DIRECTION('ref_axis',(0.550409950506719,0.834894536084164,0.));
#15870=DIRECTION('',(0.,0.,1.));
#15871=DIRECTION('center_axis',(0.171137431292023,-0.985247166761097,0.));
#15872=DIRECTION('ref_axis',(0.985247166761097,0.171137431292023,0.));
#15873=DIRECTION('',(0.985247166761096,0.171137431292023,0.));
#15874=DIRECTION('',(0.,0.,1.));
#15875=DIRECTION('',(-0.985247166761096,-0.171137431292023,0.));
#15876=DIRECTION('center_axis',(0.,0.,1.));
#15877=DIRECTION('ref_axis',(0.550409950506721,-0.834894536084163,0.));
#15878=DIRECTION('center_axis',(0.,0.,-1.));
#15879=DIRECTION('ref_axis',(0.550409950506721,-0.834894536084163,0.));
#15880=DIRECTION('',(0.,0.,1.));
#15881=DIRECTION('center_axis',(0.,0.,1.));
#15882=DIRECTION('ref_axis',(0.550409950506721,-0.834894536084163,0.));
#15883=DIRECTION('',(0.,0.,-1.));
#15884=DIRECTION('center_axis',(0.171137431292024,0.985247166761096,0.));
#15885=DIRECTION('ref_axis',(-0.985247166761096,0.171137431292024,0.));
#15886=DIRECTION('',(-0.985247166761096,0.171137431292024,0.));
#15887=DIRECTION('',(0.,0.,1.));
#15888=DIRECTION('',(-0.985247166761096,0.171137431292024,0.));
#15889=DIRECTION('center_axis',(0.,0.,-1.));
#15890=DIRECTION('ref_axis',(0.936029699362847,0.351921016579996,0.));
#15891=DIRECTION('center_axis',(0.,0.,1.));
#15892=DIRECTION('ref_axis',(0.936029699362847,0.351921016579996,0.));
#15893=DIRECTION('',(0.,0.,-1.));
#15894=DIRECTION('center_axis',(0.,0.,-1.));
#15895=DIRECTION('ref_axis',(0.936029699362847,0.351921016579996,0.));
#15896=DIRECTION('',(0.,0.,1.));
#15897=DIRECTION('center_axis',(-0.440660664196194,-0.897673759798163,0.));
#15898=DIRECTION('ref_axis',(0.897673759798163,-0.440660664196194,0.));
#15899=DIRECTION('',(0.897673759798163,-0.440660664196194,0.));
#15900=DIRECTION('',(0.,0.,1.));
#15901=DIRECTION('',(-0.897673759798163,0.440660664196194,0.));
#15902=DIRECTION('center_axis',(0.,0.,1.));
#15903=DIRECTION('ref_axis',(-0.0454476916968339,-0.998966719825755,0.));
#15904=DIRECTION('center_axis',(0.,0.,-1.));
#15905=DIRECTION('ref_axis',(-0.0454476916968339,-0.998966719825755,0.));
#15906=DIRECTION('',(0.,0.,1.));
#15907=DIRECTION('center_axis',(0.,0.,1.));
#15908=DIRECTION('ref_axis',(-0.0454476916968339,-0.998966719825755,0.));
#15909=DIRECTION('',(0.,0.,-1.));
#15910=DIRECTION('center_axis',(0.717566844774038,0.696489643340827,0.));
#15911=DIRECTION('ref_axis',(-0.696489643340827,0.717566844774038,0.));
#15912=DIRECTION('',(-0.696489643340827,0.717566844774038,0.));
#15913=DIRECTION('',(0.,0.,1.));
#15914=DIRECTION('',(-0.696489643340827,0.717566844774038,0.));
#15915=DIRECTION('center_axis',(0.,0.,-1.));
#15916=DIRECTION('ref_axis',(0.964117917541713,-0.265474369902315,0.));
#15917=DIRECTION('center_axis',(0.,0.,1.));
#15918=DIRECTION('ref_axis',(0.964117917541713,-0.265474369902315,0.));
#15919=DIRECTION('',(0.,0.,-1.));
#15920=DIRECTION('center_axis',(0.,0.,-1.));
#15921=DIRECTION('ref_axis',(0.964117917541713,-0.265474369902315,0.));
#15922=DIRECTION('',(0.,0.,1.));
#15923=DIRECTION('center_axis',(-0.884141363466569,-0.46721948740124,0.));
#15924=DIRECTION('ref_axis',(0.46721948740124,-0.884141363466569,0.));
#15925=DIRECTION('',(0.46721948740124,-0.884141363466568,0.));
#15926=DIRECTION('',(0.,0.,1.));
#15927=DIRECTION('',(-0.46721948740124,0.884141363466568,0.));
#15928=DIRECTION('center_axis',(0.,0.,1.));
#15929=DIRECTION('ref_axis',(-0.623945860382415,-0.781467570223901,0.));
#15930=DIRECTION('center_axis',(0.,0.,-1.));
#15931=DIRECTION('ref_axis',(-0.623945860382415,-0.781467570223901,0.));
#15932=DIRECTION('',(0.,0.,1.));
#15933=DIRECTION('center_axis',(0.,0.,1.));
#15934=DIRECTION('ref_axis',(-0.623945860382415,-0.781467570223901,0.));
#15935=DIRECTION('',(0.,0.,-1.));
#15936=DIRECTION('center_axis',(0.989910112752389,0.141696748976653,0.));
#15937=DIRECTION('ref_axis',(-0.141696748976653,0.989910112752389,0.));
#15938=DIRECTION('',(-0.141696748976653,0.989910112752389,0.));
#15939=DIRECTION('',(0.,0.,1.));
#15940=DIRECTION('',(-0.141696748976653,0.989910112752389,0.));
#15941=DIRECTION('center_axis',(0.,0.,-1.));
#15942=DIRECTION('ref_axis',(0.623945860382414,-0.781467570223902,0.));
#15943=DIRECTION('center_axis',(0.,0.,1.));
#15944=DIRECTION('ref_axis',(0.623945860382414,-0.781467570223902,0.));
#15945=DIRECTION('',(0.,0.,-1.));
#15946=DIRECTION('center_axis',(0.,0.,-1.));
#15947=DIRECTION('ref_axis',(0.623945860382414,-0.781467570223902,0.));
#15948=DIRECTION('',(0.,0.,1.));
#15949=DIRECTION('center_axis',(-0.989910112752389,0.141696748976654,0.));
#15950=DIRECTION('ref_axis',(-0.141696748976654,-0.989910112752389,0.));
#15951=DIRECTION('',(-0.141696748976654,-0.989910112752389,0.));
#15952=DIRECTION('',(0.,0.,1.));
#15953=DIRECTION('',(0.141696748976654,0.989910112752389,0.));
#15954=DIRECTION('center_axis',(0.,0.,1.));
#15955=DIRECTION('ref_axis',(-0.964117917541714,-0.265474369902312,0.));
#15956=DIRECTION('center_axis',(0.,0.,-1.));
#15957=DIRECTION('ref_axis',(-0.964117917541714,-0.265474369902312,0.));
#15958=DIRECTION('',(0.,0.,1.));
#15959=DIRECTION('center_axis',(0.,0.,1.));
#15960=DIRECTION('ref_axis',(-0.964117917541714,-0.265474369902312,0.));
#15961=DIRECTION('',(0.,0.,-1.));
#15962=DIRECTION('center_axis',(0.884141363466569,-0.46721948740124,0.));
#15963=DIRECTION('ref_axis',(0.46721948740124,0.884141363466569,0.));
#15964=DIRECTION('',(0.46721948740124,0.884141363466568,0.));
#15965=DIRECTION('',(0.,0.,1.));
#15966=DIRECTION('',(0.46721948740124,0.884141363466568,0.));
#15967=DIRECTION('center_axis',(0.,0.,-1.));
#15968=DIRECTION('ref_axis',(0.0454476916968278,-0.998966719825756,0.));
#15969=DIRECTION('center_axis',(0.,0.,1.));
#15970=DIRECTION('ref_axis',(0.0454476916968278,-0.998966719825756,0.));
#15971=DIRECTION('',(0.,0.,-1.));
#15972=DIRECTION('center_axis',(0.,0.,-1.));
#15973=DIRECTION('ref_axis',(0.0454476916968278,-0.998966719825756,0.));
#15974=DIRECTION('',(0.,0.,1.));
#15975=DIRECTION('center_axis',(-0.717566844774037,0.696489643340827,0.));
#15976=DIRECTION('ref_axis',(-0.696489643340827,-0.717566844774037,0.));
#15977=DIRECTION('',(-0.696489643340827,-0.717566844774037,0.));
#15978=DIRECTION('',(0.,0.,1.));
#15979=DIRECTION('',(0.696489643340827,0.717566844774037,0.));
#15980=DIRECTION('center_axis',(0.,0.,1.));
#15981=DIRECTION('ref_axis',(-0.936029699362846,0.351921016579999,0.));
#15982=DIRECTION('center_axis',(0.,0.,-1.));
#15983=DIRECTION('ref_axis',(-0.936029699362846,0.351921016579999,0.));
#15984=DIRECTION('',(0.,0.,1.));
#15985=DIRECTION('center_axis',(0.,0.,1.));
#15986=DIRECTION('ref_axis',(-0.936029699362846,0.351921016579999,0.));
#15987=DIRECTION('',(0.,0.,-1.));
#15988=DIRECTION('center_axis',(0.440660664196194,-0.897673759798163,0.));
#15989=DIRECTION('ref_axis',(0.897673759798163,0.440660664196194,0.));
#15990=DIRECTION('',(0.897673759798163,0.440660664196194,0.));
#15991=DIRECTION('',(0.,0.,1.));
#15992=DIRECTION('',(0.897673759798163,0.440660664196194,0.));
#15993=DIRECTION('',(0.,0.,1.));
#15994=DIRECTION('center_axis',(0.,0.,1.));
#15995=DIRECTION('ref_axis',(0.779271010009485,-0.62668707738296,0.));
#15996=DIRECTION('center_axis',(0.,0.,1.));
#15997=DIRECTION('ref_axis',(0.779271010009485,-0.62668707738296,0.));
#15998=DIRECTION('center_axis',(0.,0.,1.));
#15999=DIRECTION('ref_axis',(0.779271010009485,-0.62668707738296,0.));
#16000=DIRECTION('',(0.,0.,1.));
#16001=DIRECTION('',(0.,0.,1.));
#16002=DIRECTION('center_axis',(0.,0.,1.));
#16003=DIRECTION('ref_axis',(0.262086068433427,-0.965044502980618,0.));
#16004=DIRECTION('center_axis',(0.,0.,1.));
#16005=DIRECTION('ref_axis',(0.262086068433427,-0.965044502980618,0.));
#16006=DIRECTION('center_axis',(0.,0.,1.));
#16007=DIRECTION('ref_axis',(0.262086068433427,-0.965044502980618,0.));
#16008=DIRECTION('',(0.,0.,1.));
#16009=DIRECTION('',(0.,0.,1.));
#16010=DIRECTION('center_axis',(0.,0.,1.));
#16011=DIRECTION('ref_axis',(-0.355206843306369,-0.934787729095929,0.));
#16012=DIRECTION('center_axis',(0.,0.,1.));
#16013=DIRECTION('ref_axis',(-0.355206843306369,-0.934787729095929,0.));
#16014=DIRECTION('center_axis',(0.,0.,1.));
#16015=DIRECTION('ref_axis',(-0.355206843306369,-0.934787729095929,0.));
#16016=DIRECTION('',(0.,0.,1.));
#16017=DIRECTION('',(0.,0.,1.));
#16018=DIRECTION('center_axis',(0.,0.,1.));
#16019=DIRECTION('ref_axis',(-0.83682281393969,-0.547473814962924,0.));
#16020=DIRECTION('center_axis',(0.,0.,1.));
#16021=DIRECTION('ref_axis',(-0.83682281393969,-0.547473814962924,0.));
#16022=DIRECTION('center_axis',(0.,0.,1.));
#16023=DIRECTION('ref_axis',(-0.83682281393969,-0.547473814962924,0.));
#16024=DIRECTION('',(0.,0.,1.));
#16025=DIRECTION('',(0.,0.,1.));
#16026=DIRECTION('center_axis',(0.,0.,1.));
#16027=DIRECTION('ref_axis',(-0.998800912209379,0.048956488535347,0.));
#16028=DIRECTION('center_axis',(0.,0.,1.));
#16029=DIRECTION('ref_axis',(-0.998800912209379,0.048956488535347,0.));
#16030=DIRECTION('center_axis',(0.,0.,1.));
#16031=DIRECTION('ref_axis',(-0.998800912209379,0.048956488535347,0.));
#16032=DIRECTION('',(0.,0.,1.));
#16033=DIRECTION('',(0.,0.,1.));
#16034=DIRECTION('center_axis',(0.,0.,1.));
#16035=DIRECTION('ref_axis',(-0.779271010009485,0.62668707738296,0.));
#16036=DIRECTION('center_axis',(0.,0.,1.));
#16037=DIRECTION('ref_axis',(-0.779271010009485,0.62668707738296,0.));
#16038=DIRECTION('center_axis',(0.,0.,1.));
#16039=DIRECTION('ref_axis',(-0.779271010009485,0.62668707738296,0.));
#16040=DIRECTION('',(0.,0.,1.));
#16041=DIRECTION('',(0.,0.,1.));
#16042=DIRECTION('center_axis',(0.,0.,1.));
#16043=DIRECTION('ref_axis',(-0.262086068433428,0.965044502980618,0.));
#16044=DIRECTION('center_axis',(0.,0.,1.));
#16045=DIRECTION('ref_axis',(-0.262086068433428,0.965044502980618,0.));
#16046=DIRECTION('center_axis',(0.,0.,1.));
#16047=DIRECTION('ref_axis',(-0.262086068433428,0.965044502980618,0.));
#16048=DIRECTION('',(0.,0.,1.));
#16049=DIRECTION('',(0.,0.,1.));
#16050=DIRECTION('center_axis',(0.,0.,1.));
#16051=DIRECTION('ref_axis',(0.355206843306369,0.934787729095929,0.));
#16052=DIRECTION('center_axis',(0.,0.,1.));
#16053=DIRECTION('ref_axis',(0.355206843306369,0.934787729095929,0.));
#16054=DIRECTION('center_axis',(0.,0.,1.));
#16055=DIRECTION('ref_axis',(0.355206843306369,0.934787729095929,0.));
#16056=DIRECTION('',(0.,0.,1.));
#16057=DIRECTION('',(0.,0.,1.));
#16058=DIRECTION('center_axis',(0.,0.,1.));
#16059=DIRECTION('ref_axis',(0.83682281393969,0.547473814962924,0.));
#16060=DIRECTION('center_axis',(0.,0.,1.));
#16061=DIRECTION('ref_axis',(0.83682281393969,0.547473814962924,0.));
#16062=DIRECTION('center_axis',(0.,0.,1.));
#16063=DIRECTION('ref_axis',(0.83682281393969,0.547473814962924,0.));
#16064=DIRECTION('',(0.,0.,1.));
#16065=DIRECTION('center_axis',(0.,0.,1.));
#16066=DIRECTION('ref_axis',(1.,0.,0.));
#16067=DIRECTION('center_axis',(0.,0.,1.));
#16068=DIRECTION('ref_axis',(1.,0.,0.));
#16069=DIRECTION('center_axis',(0.,0.,1.));
#16070=DIRECTION('ref_axis',(1.,0.,0.));
#16071=DIRECTION('center_axis',(0.,0.,1.));
#16072=DIRECTION('ref_axis',(1.,0.,0.));
#16073=DIRECTION('center_axis',(0.,0.,1.));
#16074=DIRECTION('ref_axis',(1.,0.,0.));
#16075=DIRECTION('center_axis',(0.,0.,1.));
#16076=DIRECTION('ref_axis',(1.,0.,0.));
#16077=DIRECTION('center_axis',(0.,0.,1.));
#16078=DIRECTION('ref_axis',(1.,0.,0.));
#16079=DIRECTION('center_axis',(0.,0.,1.));
#16080=DIRECTION('ref_axis',(1.,0.,0.));
#16081=DIRECTION('center_axis',(0.,0.,1.));
#16082=DIRECTION('ref_axis',(1.,0.,0.));
#16083=DIRECTION('center_axis',(0.,0.,-1.));
#16084=DIRECTION('ref_axis',(-0.55040995050672,-0.834894536084163,0.));
#16085=DIRECTION('',(0.985247166761096,0.171137431292024,0.));
#16086=DIRECTION('center_axis',(0.,0.,1.));
#16087=DIRECTION('ref_axis',(0.998800912209379,-0.0489564885353468,0.));
#16088=DIRECTION('',(0.985247166761096,-0.171137431292024,0.));
#16089=DIRECTION('center_axis',(0.,0.,-1.));
#16090=DIRECTION('ref_axis',(-0.55040995050672,0.834894536084163,0.));
#16091=DIRECTION('center_axis',(0.,0.,1.));
#16092=DIRECTION('ref_axis',(1.,0.,0.));
#16093=DIRECTION('center_axis',(0.,0.,1.));
#16094=DIRECTION('ref_axis',(1.,0.,0.));
#16095=DIRECTION('center_axis',(0.,0.,1.));
#16096=DIRECTION('ref_axis',(1.,0.,0.));
#16097=DIRECTION('center_axis',(0.,0.,1.));
#16098=DIRECTION('ref_axis',(1.,0.,0.));
#16099=DIRECTION('center_axis',(0.,0.,1.));
#16100=DIRECTION('ref_axis',(-0.55040995050672,0.834894536084163,0.));
#16101=DIRECTION('',(0.985247166761096,-0.171137431292024,0.));
#16102=DIRECTION('center_axis',(0.,0.,1.));
#16103=DIRECTION('ref_axis',(0.998800912209379,-0.0489564885353468,0.));
#16104=DIRECTION('',(-0.985247166761096,-0.171137431292024,0.));
#16105=DIRECTION('center_axis',(0.,0.,1.));
#16106=DIRECTION('ref_axis',(-0.55040995050672,-0.834894536084163,0.));
#16107=DIRECTION('center_axis',(0.,0.,1.));
#16108=DIRECTION('ref_axis',(1.,0.,0.));
#16109=DIRECTION('center_axis',(0.,0.,1.));
#16110=DIRECTION('ref_axis',(1.,0.,0.));
#16111=DIRECTION('center_axis',(0.,0.,1.));
#16112=DIRECTION('ref_axis',(1.,0.,0.));
#16113=DIRECTION('center_axis',(0.,0.,1.));
#16114=DIRECTION('ref_axis',(1.,0.,0.));
#16115=DIRECTION('center_axis',(0.,0.,1.));
#16116=DIRECTION('ref_axis',(1.,0.,0.));
#16117=DIRECTION('center_axis',(0.,0.,1.));
#16118=DIRECTION('ref_axis',(1.,0.,0.));
#16119=DIRECTION('center_axis',(0.,0.,1.));
#16120=DIRECTION('ref_axis',(1.,0.,0.));
#16121=DIRECTION('center_axis',(0.,0.,1.));
#16122=DIRECTION('ref_axis',(1.,0.,0.));
#16123=DIRECTION('center_axis',(0.,0.,1.));
#16124=DIRECTION('ref_axis',(1.,0.,0.));
#16125=DIRECTION('center_axis',(0.,0.,1.));
#16126=DIRECTION('ref_axis',(1.,0.,0.));
#16127=DIRECTION('',(0.,0.,1.));
#16128=DIRECTION('center_axis',(0.,0.,1.));
#16129=DIRECTION('ref_axis',(1.,0.,0.));
#16130=DIRECTION('center_axis',(0.,0.,1.));
#16131=DIRECTION('ref_axis',(1.,0.,0.));
#16132=DIRECTION('center_axis',(0.,0.,1.));
#16133=DIRECTION('ref_axis',(1.,0.,0.));
#16134=DIRECTION('center_axis',(0.,0.,1.));
#16135=DIRECTION('ref_axis',(1.,0.,0.));
#16136=DIRECTION('center_axis',(0.,0.,1.));
#16137=DIRECTION('ref_axis',(1.,0.,0.));
#16138=DIRECTION('center_axis',(0.,0.,1.));
#16139=DIRECTION('ref_axis',(1.,0.,0.));
#16140=DIRECTION('center_axis',(0.,0.,1.));
#16141=DIRECTION('ref_axis',(1.,0.,0.));
#16142=DIRECTION('center_axis',(0.,0.,1.));
#16143=DIRECTION('ref_axis',(1.,0.,0.));
#16144=DIRECTION('center_axis',(0.,0.,-1.));
#16145=DIRECTION('ref_axis',(-0.55040995050672,-0.834894536084163,0.));
#16146=DIRECTION('',(0.,0.,-1.));
#16147=DIRECTION('center_axis',(-0.171137431292024,0.985247166761097,0.));
#16148=DIRECTION('ref_axis',(-0.985247166761096,-0.171137431292024,0.));
#16149=DIRECTION('',(0.,0.,1.));
#16150=DIRECTION('center_axis',(0.,0.,1.));
#16151=DIRECTION('ref_axis',(-0.55040995050672,0.834894536084163,0.));
#16152=DIRECTION('',(0.,0.,1.));
#16153=DIRECTION('',(0.,0.,-1.));
#16154=DIRECTION('center_axis',(-0.171137431292024,-0.985247166761097,0.));
#16155=DIRECTION('ref_axis',(0.985247166761096,-0.171137431292024,0.));
#16156=DIRECTION('',(0.,0.,1.));
#16157=DIRECTION('',(0.,0.,1.));
#16158=DIRECTION('center_axis',(0.,0.,1.));
#16159=DIRECTION('ref_axis',(0.998800912209379,-0.0489564885353468,0.));
#16160=DIRECTION('',(0.,0.,1.));
#16161=DIRECTION('center_axis',(0.,0.,1.));
#16162=DIRECTION('ref_axis',(1.,0.,0.));
#16163=DIRECTION('axis',(0.,0.,1.));
#16164=DIRECTION('refdir',(1.,0.,0.));
#16165=DIRECTION('center_axis',(0.,-1.83697019872103E-16,1.));
#16166=DIRECTION('ref_axis',(0.,-1.,-1.83697019872103E-16));
#16167=DIRECTION('center_axis',(0.,-1.83697019872103E-16,1.));
#16168=DIRECTION('ref_axis',(0.,-1.,-1.83697019872103E-16));
#16169=DIRECTION('center_axis',(1.,1.22464679914735E-16,2.24963967399279E-32));
#16170=DIRECTION('ref_axis',(-1.22464679914735E-16,1.,1.83697019872103E-16));
#16171=DIRECTION('center_axis',(0.,-1.83697019872103E-16,1.));
#16172=DIRECTION('ref_axis',(0.,-1.,-1.83697019872103E-16));
#16173=DIRECTION('center_axis',(0.,1.83697019872103E-16,-1.));
#16174=DIRECTION('ref_axis',(0.,1.,2.09599627067876E-16));
#16175=DIRECTION('center_axis',(0.,1.83697019872103E-16,-1.));
#16176=DIRECTION('ref_axis',(0.,1.,1.83697019872103E-16));
#16177=DIRECTION('center_axis',(0.,1.83697019872103E-16,-1.));
#16178=DIRECTION('ref_axis',(0.,1.,1.83697019872103E-16));
#16179=DIRECTION('center_axis',(-1.,1.22464679914735E-16,2.24963967399279E-32));
#16180=DIRECTION('ref_axis',(-1.22464679914735E-16,-1.,-1.30999766917423E-16));
#16181=DIRECTION('center_axis',(0.,-1.83697019872103E-16,1.));
#16182=DIRECTION('ref_axis',(0.,1.,1.83697019872103E-16));
#16183=DIRECTION('center_axis',(0.,-1.83697019872103E-16,1.));
#16184=DIRECTION('ref_axis',(0.,1.,1.83697019872103E-16));
#16185=DIRECTION('center_axis',(0.,1.83697019872103E-16,-1.));
#16186=DIRECTION('ref_axis',(0.,1.,2.09599627067876E-16));
#16187=DIRECTION('center_axis',(0.,1.83697019872103E-16,-1.));
#16188=DIRECTION('ref_axis',(0.,1.,1.83697019872103E-16));
#16189=DIRECTION('center_axis',(0.,1.83697019872103E-16,-1.));
#16190=DIRECTION('ref_axis',(0.,1.,1.83697019872103E-16));
#16191=DIRECTION('center_axis',(-1.,1.22464679914735E-16,2.24963967399279E-32));
#16192=DIRECTION('ref_axis',(-1.22464679914735E-16,-1.,-1.30999766917423E-16));
#16193=DIRECTION('center_axis',(0.,-1.83697019872103E-16,1.));
#16194=DIRECTION('ref_axis',(0.,-1.,-1.83697019872103E-16));
#16195=DIRECTION('center_axis',(0.,-1.83697019872103E-16,1.));
#16196=DIRECTION('ref_axis',(0.,-1.,-1.83697019872103E-16));
#16197=DIRECTION('',(-8.65956056235483E-17,0.707106781186539,0.707106781186556));
#16198=DIRECTION('center_axis',(0.,-1.83697019872103E-16,1.));
#16199=DIRECTION('ref_axis',(0.,-1.,-1.83697019872103E-16));
#16200=DIRECTION('center_axis',(0.,-1.83697019872103E-16,1.));
#16201=DIRECTION('ref_axis',(0.,-1.,-1.83697019872103E-16));
#16202=DIRECTION('',(0.,-1.83697019872103E-16,1.));
#16203=DIRECTION('center_axis',(0.,1.83697019872103E-16,-1.));
#16204=DIRECTION('ref_axis',(0.,1.,1.83697019872103E-16));
#16205=DIRECTION('',(-8.65956056235483E-17,-0.707106781186539,-0.707106781186556));
#16206=DIRECTION('center_axis',(0.,-1.83697019872103E-16,1.));
#16207=DIRECTION('ref_axis',(0.,-1.,-1.83697019872103E-16));
#16208=DIRECTION('center_axis',(0.,-1.83697019872103E-16,1.));
#16209=DIRECTION('ref_axis',(0.,-1.,-1.83697019872103E-16));
#16210=DIRECTION('',(0.,1.83697019872103E-16,-1.));
#16211=DIRECTION('center_axis',(0.,-1.83697019872103E-16,1.));
#16212=DIRECTION('ref_axis',(0.,-1.,-1.83697019872103E-16));
#16213=DIRECTION('center_axis',(0.,-1.83697019872103E-16,1.));
#16214=DIRECTION('ref_axis',(0.,-1.,-1.83697019872103E-16));
#16215=DIRECTION('center_axis',(0.,-1.83697019872103E-16,1.));
#16216=DIRECTION('ref_axis',(0.,-1.,-1.83697019872103E-16));
#16217=DIRECTION('',(0.,1.83697019872103E-16,-1.));
#16218=DIRECTION('center_axis',(0.,1.83697019872103E-16,-1.));
#16219=DIRECTION('ref_axis',(0.,1.,1.83697019872103E-16));
#16220=DIRECTION('center_axis',(0.,-1.83697019872103E-16,1.));
#16221=DIRECTION('ref_axis',(0.,-1.,-1.83697019872103E-16));
#16222=DIRECTION('center_axis',(-1.,0.,0.));
#16223=DIRECTION('ref_axis',(0.,1.,0.));
#16224=DIRECTION('center_axis',(0.,1.22464679914735E-16,1.));
#16225=DIRECTION('ref_axis',(0.,-1.,1.22464679914735E-16));
#16226=DIRECTION('center_axis',(-0.623489801858732,0.781831482468031,1.43620113371566E-16));
#16227=DIRECTION('ref_axis',(0.781831482468031,0.623489801858732,-6.91638013500061E-17));
#16228=DIRECTION('center_axis',(2.39366855619276E-16,7.19167766472515E-18,
1.));
#16229=DIRECTION('ref_axis',(-0.781831482468031,-0.623489801858732,1.91628481264741E-16));
#16230=DIRECTION('center_axis',(0.222520933956319,0.974927912181823,1.79091352057932E-16));
#16231=DIRECTION('ref_axis',(0.974927912181823,-0.222520933956319,-2.24573452299036E-16));
#16232=DIRECTION('center_axis',(2.98485586763221E-16,-2.51824407250324E-16,
1.));
#16233=DIRECTION('ref_axis',(-0.974927912181823,0.222520933956319,3.47038132213772E-16));
#16234=DIRECTION('center_axis',(0.900968867902422,0.433883739117552,7.97031498468594E-17));
#16235=DIRECTION('ref_axis',(0.433883739117552,-0.900968867902422,-3.4920231590332E-16));
#16236=DIRECTION('center_axis',(1.32838583078098E-16,-4.59539179924132E-16,
1.));
#16237=DIRECTION('ref_axis',(-0.433883739117552,0.900968867902422,4.71666995818055E-16));
#16238=DIRECTION('center_axis',(0.900968867902416,-0.433883739117565,-7.97031498468616E-17));
#16239=DIRECTION('ref_axis',(-0.433883739117565,-0.900968867902416,-3.49202315903319E-16));
#16240=DIRECTION('center_axis',(-1.32838583078103E-16,-4.5953917992413E-16,
1.));
#16241=DIRECTION('ref_axis',(0.433883739117565,0.900968867902416,4.71666995818054E-16));
#16242=DIRECTION('center_axis',(0.222520933956305,-0.974927912181826,-1.79091352057933E-16));
#16243=DIRECTION('ref_axis',(-0.974927912181826,-0.222520933956305,-2.24573452299033E-16));
#16244=DIRECTION('center_axis',(-2.98485586763221E-16,-2.5182440725032E-16,
1.));
#16245=DIRECTION('ref_axis',(0.974927912181826,0.222520933956305,3.47038132213768E-16));
#16246=DIRECTION('center_axis',(-0.623489801858743,-0.781831482468022,-1.43620113371564E-16));
#16247=DIRECTION('ref_axis',(-0.781831482468022,0.623489801858743,-6.91638013500039E-17));
#16248=DIRECTION('center_axis',(-2.39366855619273E-16,7.19167766472869E-18,
1.));
#16249=DIRECTION('ref_axis',(0.781831482468022,-0.623489801858743,1.91628481264739E-16));
#16250=DIRECTION('center_axis',(0.,1.83697019872103E-16,-1.));
#16251=DIRECTION('ref_axis',(0.,1.,1.62614292875575E-16));
#16252=DIRECTION('center_axis',(0.,1.83697019872103E-16,-1.));
#16253=DIRECTION('ref_axis',(0.,1.,1.83697019872103E-16));
#16254=DIRECTION('center_axis',(-1.,1.22464679914735E-16,2.24963967399279E-32));
#16255=DIRECTION('ref_axis',(-1.22464679914735E-16,-1.,-2.03267866094469E-16));
#16256=DIRECTION('center_axis',(0.,-1.83697019872103E-16,1.));
#16257=DIRECTION('ref_axis',(0.,1.,1.83697019872103E-16));
#16258=DIRECTION('center_axis',(0.,-1.83697019872103E-16,1.));
#16259=DIRECTION('ref_axis',(0.,1.,1.83697019872103E-16));
#16260=DIRECTION('center_axis',(0.,-1.83697019872103E-16,1.));
#16261=DIRECTION('ref_axis',(0.,-1.,-1.64970202400831E-16));
#16262=DIRECTION('center_axis',(0.,-1.83697019872103E-16,1.));
#16263=DIRECTION('ref_axis',(0.,-1.,-1.83697019872103E-16));
#16264=DIRECTION('center_axis',(-1.,-1.22464679914735E-16,-2.24963967399279E-32));
#16265=DIRECTION('ref_axis',(-1.22464679914735E-16,1.,2.06212753001039E-16));
#16266=DIRECTION('center_axis',(0.,1.83697019872103E-16,-1.));
#16267=DIRECTION('ref_axis',(0.,-1.,-1.83697019872103E-16));
#16268=DIRECTION('center_axis',(0.,-1.83697019872103E-16,1.));
#16269=DIRECTION('ref_axis',(0.,-1.,-1.62614292875575E-16));
#16270=DIRECTION('center_axis',(0.,-1.83697019872103E-16,1.));
#16271=DIRECTION('ref_axis',(0.,-1.,-1.83697019872103E-16));
#16272=DIRECTION('center_axis',(-1.,-1.22464679914735E-16,-2.24963967399279E-32));
#16273=DIRECTION('ref_axis',(-1.22464679914735E-16,1.,2.03267866094469E-16));
#16274=DIRECTION('center_axis',(0.,1.83697019872103E-16,-1.));
#16275=DIRECTION('ref_axis',(0.,-1.,-1.83697019872103E-16));
#16276=DIRECTION('center_axis',(0.,1.83697019872103E-16,-1.));
#16277=DIRECTION('ref_axis',(0.,1.,1.64970202400831E-16));
#16278=DIRECTION('center_axis',(0.,1.83697019872103E-16,-1.));
#16279=DIRECTION('ref_axis',(0.,1.,1.83697019872103E-16));
#16280=DIRECTION('center_axis',(0.,1.83697019872103E-16,-1.));
#16281=DIRECTION('ref_axis',(0.,1.,1.83697019872103E-16));
#16282=DIRECTION('center_axis',(-1.,1.22464679914735E-16,2.24963967399279E-32));
#16283=DIRECTION('ref_axis',(-1.22464679914735E-16,-1.,-2.06212753001039E-16));
#16284=DIRECTION('center_axis',(0.,-1.83697019872103E-16,1.));
#16285=DIRECTION('ref_axis',(0.,1.,1.83697019872103E-16));
#16286=DIRECTION('center_axis',(0.,-1.83697019872103E-16,1.));
#16287=DIRECTION('ref_axis',(0.,-1.,-1.83697019872103E-16));
#16288=DIRECTION('center_axis',(0.,-1.83697019872103E-16,1.));
#16289=DIRECTION('ref_axis',(0.,-1.,-1.83697019872103E-16));
#16290=DIRECTION('',(0.,-1.83697019872103E-16,1.));
#16291=DIRECTION('center_axis',(0.,-1.83697019872103E-16,1.));
#16292=DIRECTION('ref_axis',(0.,-1.,-1.83697019872103E-16));
#16293=DIRECTION('center_axis',(0.,-1.83697019872103E-16,1.));
#16294=DIRECTION('ref_axis',(0.,-1.,-1.83697019872103E-16));
#16295=DIRECTION('center_axis',(0.,-1.83697019872103E-16,1.));
#16296=DIRECTION('ref_axis',(0.,-1.,-1.83697019872103E-16));
#16297=DIRECTION('',(0.,-1.83697019872103E-16,1.));
#16298=DIRECTION('center_axis',(0.,-1.83697019872103E-16,1.));
#16299=DIRECTION('ref_axis',(0.,-1.,-1.83697019872103E-16));
#16300=DIRECTION('',(0.,-1.83697019872103E-16,1.));
#16301=DIRECTION('center_axis',(0.,-1.83697019872103E-16,1.));
#16302=DIRECTION('ref_axis',(0.,-1.,-1.83697019872103E-16));
#16303=DIRECTION('center_axis',(0.,-1.83697019872103E-16,1.));
#16304=DIRECTION('ref_axis',(0.,-1.,-1.83697019872103E-16));
#16305=DIRECTION('center_axis',(1.,1.22464679914735E-16,2.24963967399279E-32));
#16306=DIRECTION('ref_axis',(-1.22464679914735E-16,1.,1.83697019872103E-16));
#16307=DIRECTION('center_axis',(0.,-1.83697019872103E-16,1.));
#16308=DIRECTION('ref_axis',(0.,-1.,-1.83697019872103E-16));
#16309=DIRECTION('center_axis',(0.,-1.83697019872103E-16,1.));
#16310=DIRECTION('ref_axis',(0.,-1.,-1.83697019872103E-16));
#16311=DIRECTION('',(0.,-1.83697019872103E-16,1.));
#16312=DIRECTION('center_axis',(0.,-1.83697019872103E-16,1.));
#16313=DIRECTION('ref_axis',(0.,-1.,-1.83697019872103E-16));
#16314=DIRECTION('',(0.,-1.83697019872103E-16,1.));
#16315=DIRECTION('center_axis',(0.,-1.83697019872103E-16,1.));
#16316=DIRECTION('ref_axis',(0.,-1.,-1.83697019872103E-16));
#16317=DIRECTION('center_axis',(0.,-1.83697019872103E-16,1.));
#16318=DIRECTION('ref_axis',(0.,-1.,-1.83697019872103E-16));
#16319=DIRECTION('center_axis',(0.,-1.83697019872103E-16,1.));
#16320=DIRECTION('ref_axis',(0.,-1.,-1.83697019872103E-16));
#16321=DIRECTION('',(0.,-1.83697019872103E-16,1.));
#16322=DIRECTION('center_axis',(0.,-1.83697019872103E-16,1.));
#16323=DIRECTION('ref_axis',(0.,-1.,-1.83697019872103E-16));
#16324=DIRECTION('center_axis',(0.,-1.83697019872103E-16,1.));
#16325=DIRECTION('ref_axis',(0.,-1.,-1.83697019872103E-16));
#16326=DIRECTION('center_axis',(0.,-1.83697019872103E-16,1.));
#16327=DIRECTION('ref_axis',(0.,-1.,-1.83697019872103E-16));
#16328=DIRECTION('',(8.65956056235488E-17,-0.707106781186543,-0.707106781186552));
#16329=DIRECTION('center_axis',(0.,-1.83697019872103E-16,1.));
#16330=DIRECTION('ref_axis',(0.,-1.,-1.83697019872103E-16));
#16331=DIRECTION('center_axis',(0.,1.83697019872103E-16,-1.));
#16332=DIRECTION('ref_axis',(0.,1.,1.83697019872103E-16));
#16333=DIRECTION('center_axis',(0.,-1.83697019872103E-16,1.));
#16334=DIRECTION('ref_axis',(0.,-1.,-1.83697019872103E-16));
#16335=DIRECTION('',(8.65956056235488E-17,0.707106781186543,0.707106781186552));
#16336=DIRECTION('center_axis',(0.,-1.83697019872103E-16,1.));
#16337=DIRECTION('ref_axis',(0.,-1.,-1.83697019872103E-16));
#16338=DIRECTION('center_axis',(0.,-1.83697019872103E-16,1.));
#16339=DIRECTION('ref_axis',(0.,-1.,-1.83697019872103E-16));
#16340=DIRECTION('center_axis',(0.,-1.83697019872103E-16,1.));
#16341=DIRECTION('ref_axis',(0.,-1.,-1.83697019872103E-16));
#16342=DIRECTION('',(0.,1.83697019872103E-16,-1.));
#16343=DIRECTION('center_axis',(0.,1.83697019872103E-16,-1.));
#16344=DIRECTION('ref_axis',(0.,1.,1.83697019872103E-16));
#16345=DIRECTION('center_axis',(0.,-1.83697019872103E-16,1.));
#16346=DIRECTION('ref_axis',(0.,-1.,-1.83697019872103E-16));
#16347=DIRECTION('center_axis',(0.,1.83697019872103E-16,-1.));
#16348=DIRECTION('ref_axis',(0.,1.,1.83697019872103E-16));
#16349=DIRECTION('center_axis',(0.,-1.83697019872103E-16,1.));
#16350=DIRECTION('ref_axis',(0.,-1.,-1.83697019872103E-16));
#16351=DIRECTION('center_axis',(0.,1.83697019872103E-16,-1.));
#16352=DIRECTION('ref_axis',(0.,1.,1.83697019872103E-16));
#16353=DIRECTION('center_axis',(0.,-1.83697019872103E-16,1.));
#16354=DIRECTION('ref_axis',(0.,-1.,-1.83697019872103E-16));
#16355=DIRECTION('center_axis',(-0.781831482468031,0.623489801858732,-6.91638013500059E-17));
#16356=DIRECTION('ref_axis',(0.,0.,1.));
#16357=DIRECTION('center_axis',(-0.781831482468031,0.623489801858732,-6.91638013500059E-17));
#16358=DIRECTION('ref_axis',(-5.40744373425995E-17,4.31229247995119E-17,
1.));
#16359=DIRECTION('center_axis',(-0.623489801858732,-0.781831482468031,2.05955304247937E-16));
#16360=DIRECTION('ref_axis',(0.,-2.63426721571497E-16,-1.));
#16361=DIRECTION('center_axis',(-0.781831482468031,0.623489801858732,-6.91638013500059E-17));
#16362=DIRECTION('ref_axis',(-5.40744373425995E-17,4.31229247995119E-17,
1.));
#16363=DIRECTION('center_axis',(0.623489801858732,0.781831482468031,1.22464679914735E-16));
#16364=DIRECTION('ref_axis',(0.,0.,1.));
#16365=DIRECTION('center_axis',(-1.79091352057932E-16,-2.24573452299036E-16,
1.));
#16366=DIRECTION('ref_axis',(-5.50003967499518E-33,-1.,-2.24573452299036E-16));
#16367=DIRECTION('center_axis',(0.781831482468031,-0.623489801858732,0.));
#16368=DIRECTION('ref_axis',(0.,0.,-1.));
#16369=DIRECTION('center_axis',(-1.43620113371566E-16,-6.91638013500059E-17,
1.));
#16370=DIRECTION('ref_axis',(0.623489801858732,0.781831482468031,1.43620113371566E-16));
#16371=DIRECTION('center_axis',(-1.43620113371566E-16,-6.91638013500059E-17,
1.));
#16372=DIRECTION('ref_axis',(0.623489801858732,0.781831482468031,1.43620113371566E-16));
#16373=DIRECTION('center_axis',(-1.43620113371566E-16,-6.91638013500059E-17,
1.));
#16374=DIRECTION('ref_axis',(0.623489801858732,0.781831482468031,1.43620113371566E-16));
#16375=DIRECTION('center_axis',(-1.79091352057932E-16,-2.24573452299036E-16,
1.));
#16376=DIRECTION('ref_axis',(-5.50003967499518E-33,-1.,-2.24573452299036E-16));
#16377=DIRECTION('center_axis',(-1.79091352057932E-16,-2.24573452299036E-16,
1.));
#16378=DIRECTION('ref_axis',(-5.5000396749952E-33,-1.,-2.24573452299036E-16));
#16379=DIRECTION('center_axis',(-0.781831482468031,0.623489801858732,-6.91638013500059E-17));
#16380=DIRECTION('ref_axis',(-5.40744373425995E-17,4.31229247995119E-17,
1.));
#16381=DIRECTION('center_axis',(-0.781831482468031,0.623489801858732,-6.91638013500059E-17));
#16382=DIRECTION('ref_axis',(-5.40744373425995E-17,4.31229247995119E-17,
1.));
#16383=DIRECTION('center_axis',(-0.974927912181823,-0.222520933956318,-2.24573452299036E-16));
#16384=DIRECTION('ref_axis',(0.,-2.10741377257197E-16,1.));
#16385=DIRECTION('center_axis',(-0.974927912181823,-0.222520933956318,-2.24573452299036E-16));
#16386=DIRECTION('ref_axis',(-1.71433215598957E-16,-2.58125940401653E-16,
1.));
#16387=DIRECTION('center_axis',(0.222520933956318,-0.974927912181823,-1.28411031837301E-16));
#16388=DIRECTION('ref_axis',(0.,1.31713360785748E-16,-1.));
#16389=DIRECTION('center_axis',(-0.974927912181823,-0.222520933956318,-2.24573452299036E-16));
#16390=DIRECTION('ref_axis',(-1.71433215598957E-16,-2.58125940401653E-16,
1.));
#16391=DIRECTION('center_axis',(-0.222520933956318,0.974927912181823,3.59586625308286E-16));
#16392=DIRECTION('ref_axis',(0.,-2.4905725751517E-16,1.));
#16393=DIRECTION('center_axis',(-7.97031498468594E-17,-3.4920231590332E-16,
1.));
#16394=DIRECTION('ref_axis',(2.39882519785021E-33,-1.,-3.4920231590332E-16));
#16395=DIRECTION('center_axis',(0.974927912181823,0.222520933956318,6.92755669385935E-17));
#16396=DIRECTION('ref_axis',(0.,3.11321571893962E-16,-1.));
#16397=DIRECTION('center_axis',(-1.79091352057932E-16,-2.24573452299036E-16,
1.));
#16398=DIRECTION('ref_axis',(-0.222520933956318,0.974927912181823,1.79091352057933E-16));
#16399=DIRECTION('center_axis',(-1.79091352057932E-16,-2.24573452299036E-16,
1.));
#16400=DIRECTION('ref_axis',(-0.222520933956318,0.974927912181823,1.79091352057933E-16));
#16401=DIRECTION('center_axis',(-1.79091352057932E-16,-2.24573452299036E-16,
1.));
#16402=DIRECTION('ref_axis',(-0.222520933956318,0.974927912181823,1.79091352057933E-16));
#16403=DIRECTION('center_axis',(-7.97031498468594E-17,-3.4920231590332E-16,
1.));
#16404=DIRECTION('ref_axis',(2.39882519785021E-33,-1.,-3.4920231590332E-16));
#16405=DIRECTION('center_axis',(-7.97031498468594E-17,-3.4920231590332E-16,
1.));
#16406=DIRECTION('ref_axis',(2.39882519785021E-33,-1.,-3.4920231590332E-16));
#16407=DIRECTION('center_axis',(-0.974927912181823,-0.222520933956318,-2.24573452299036E-16));
#16408=DIRECTION('ref_axis',(-1.64444757441796E-16,-2.88744376156862E-16,
1.));
#16409=DIRECTION('center_axis',(-0.974927912181823,-0.222520933956318,-2.24573452299036E-16));
#16410=DIRECTION('ref_axis',(-1.64444757441796E-16,-2.88744376156862E-16,
1.));
#16411=DIRECTION('center_axis',(-0.433883739117553,-0.900968867902422,-3.4920231590332E-16));
#16412=DIRECTION('ref_axis',(0.,-4.21482754514395E-16,1.));
#16413=DIRECTION('center_axis',(-0.433883739117553,-0.900968867902422,-3.4920231590332E-16));
#16414=DIRECTION('ref_axis',(1.97058769816641E-17,-3.97075180104293E-16,
1.));
#16415=DIRECTION('center_axis',(0.900968867902422,-0.433883739117553,-2.28593141877839E-16));
#16416=DIRECTION('ref_axis',(0.,5.26853443142994E-16,-1.));
#16417=DIRECTION('center_axis',(-0.433883739117553,-0.900968867902422,-3.4920231590332E-16));
#16418=DIRECTION('ref_axis',(1.97058769816641E-17,-3.97075180104293E-16,
1.));
#16419=DIRECTION('center_axis',(-0.900968867902422,0.433883739117552,3.33523066916777E-16));
#16420=DIRECTION('ref_axis',(0.,-4.9811451503034E-16,1.));
#16421=DIRECTION('center_axis',(7.97031498468617E-17,-3.49202315903319E-16,
1.));
#16422=DIRECTION('ref_axis',(-2.39882519785018E-33,-1.,-3.49202315903319E-16));
#16423=DIRECTION('center_axis',(0.433883739117552,0.900968867902422,5.60982088365811E-16));
#16424=DIRECTION('ref_axis',(0.,6.22643143787925E-16,-1.));
#16425=DIRECTION('center_axis',(-7.97031498468594E-17,-3.4920231590332E-16,
1.));
#16426=DIRECTION('ref_axis',(-0.900968867902422,0.433883739117553,7.97031498468594E-17));
#16427=DIRECTION('center_axis',(-7.97031498468594E-17,-3.4920231590332E-16,
1.));
#16428=DIRECTION('ref_axis',(-0.900968867902422,0.433883739117553,7.97031498468594E-17));
#16429=DIRECTION('center_axis',(-7.97031498468594E-17,-3.4920231590332E-16,
1.));
#16430=DIRECTION('ref_axis',(-0.900968867902422,0.433883739117553,7.97031498468594E-17));
#16431=DIRECTION('center_axis',(7.97031498468617E-17,-3.49202315903319E-16,
1.));
#16432=DIRECTION('ref_axis',(-2.39882519785018E-33,-1.,-3.49202315903319E-16));
#16433=DIRECTION('center_axis',(7.97031498468617E-17,-3.49202315903319E-16,
1.));
#16434=DIRECTION('ref_axis',(-2.39882519785018E-33,-1.,-3.49202315903319E-16));
#16435=DIRECTION('center_axis',(-0.433883739117553,-0.900968867902422,-3.4920231590332E-16));
#16436=DIRECTION('ref_axis',(4.4891409918625E-17,-4.09203893527874E-16,
1.));
#16437=DIRECTION('center_axis',(-0.433883739117553,-0.900968867902422,-3.4920231590332E-16));
#16438=DIRECTION('ref_axis',(4.48914099186251E-17,-4.09203893527874E-16,
1.));
#16439=DIRECTION('center_axis',(0.433883739117565,-0.900968867902416,-3.49202315903319E-16));
#16440=DIRECTION('ref_axis',(0.,-4.21482754514395E-16,1.));
#16441=DIRECTION('center_axis',(0.433883739117565,-0.900968867902416,-3.49202315903319E-16));
#16442=DIRECTION('ref_axis',(-1.97058769816642E-17,-3.97075180104295E-16,
1.));
#16443=DIRECTION('center_axis',(0.900968867902416,0.433883739117565,2.28593141877845E-16));
#16444=DIRECTION('ref_axis',(0.,5.26853443142994E-16,-1.));
#16445=DIRECTION('center_axis',(0.433883739117565,-0.900968867902416,-3.49202315903319E-16));
#16446=DIRECTION('ref_axis',(-1.97058769816642E-17,-3.97075180104295E-16,
1.));
#16447=DIRECTION('center_axis',(-0.900968867902416,-0.433883739117565,-8.85937070873124E-17));
#16448=DIRECTION('ref_axis',(0.,-4.9811451503034E-16,1.));
#16449=DIRECTION('center_axis',(1.79091352057933E-16,-2.24573452299033E-16,
1.));
#16450=DIRECTION('ref_axis',(5.50003967499563E-33,-1.,-2.24573452299033E-16));
#16451=DIRECTION('center_axis',(-0.433883739117565,0.900968867902416,5.60982088365808E-16));
#16452=DIRECTION('ref_axis',(0.,6.22643143787925E-16,-1.));
#16453=DIRECTION('center_axis',(7.97031498468617E-17,-3.49202315903319E-16,
1.));
#16454=DIRECTION('ref_axis',(-0.900968867902416,-0.433883739117565,-7.97031498468616E-17));
#16455=DIRECTION('center_axis',(7.97031498468617E-17,-3.49202315903319E-16,
1.));
#16456=DIRECTION('ref_axis',(-0.900968867902416,-0.433883739117565,-7.97031498468616E-17));
#16457=DIRECTION('center_axis',(7.97031498468617E-17,-3.49202315903319E-16,
1.));
#16458=DIRECTION('ref_axis',(-0.900968867902416,-0.433883739117565,-7.97031498468616E-17));
#16459=DIRECTION('center_axis',(1.79091352057933E-16,-2.24573452299033E-16,
1.));
#16460=DIRECTION('ref_axis',(5.50003967499563E-33,-1.,-2.24573452299033E-16));
#16461=DIRECTION('center_axis',(1.79091352057933E-16,-2.24573452299033E-16,
1.));
#16462=DIRECTION('ref_axis',(5.50003967499563E-33,-1.,-2.24573452299033E-16));
#16463=DIRECTION('center_axis',(0.433883739117565,-0.900968867902416,-3.49202315903319E-16));
#16464=DIRECTION('ref_axis',(-4.48914099186257E-17,-4.09203893527877E-16,
1.));
#16465=DIRECTION('center_axis',(0.433883739117565,-0.900968867902416,-3.49202315903319E-16));
#16466=DIRECTION('ref_axis',(-4.48914099186258E-17,-4.09203893527877E-16,
1.));
#16467=DIRECTION('center_axis',(0.974927912181826,-0.222520933956305,-2.24573452299033E-16));
#16468=DIRECTION('ref_axis',(0.,-2.10741377257197E-16,1.));
#16469=DIRECTION('center_axis',(0.974927912181826,-0.222520933956305,-2.24573452299033E-16));
#16470=DIRECTION('ref_axis',(1.71433215598957E-16,-2.58125940401651E-16,
1.));
#16471=DIRECTION('center_axis',(0.222520933956305,0.974927912181826,3.85233095511904E-16));
#16472=DIRECTION('ref_axis',(0.,3.95140082357245E-16,-1.));
#16473=DIRECTION('center_axis',(0.974927912181826,-0.222520933956305,-2.24573452299033E-16));
#16474=DIRECTION('ref_axis',(1.71433215598957E-16,-2.58125940401651E-16,
1.));
#16475=DIRECTION('center_axis',(-0.222520933956305,-0.974927912181826,-1.14657265478815E-16));
#16476=DIRECTION('ref_axis',(0.,-1.24528628757585E-16,1.));
#16477=DIRECTION('center_axis',(1.43620113371564E-16,-6.91638013500039E-17,
1.));
#16478=DIRECTION('ref_axis',(1.,1.10509814492259E-33,-1.43620113371564E-16));
#16479=DIRECTION('center_axis',(-0.974927912181826,0.222520933956305,3.46377834692947E-17));
#16480=DIRECTION('ref_axis',(0.,1.55660785946981E-16,-1.));
#16481=DIRECTION('center_axis',(1.79091352057933E-16,-2.24573452299033E-16,
1.));
#16482=DIRECTION('ref_axis',(-0.222520933956305,-0.974927912181826,-1.79091352057932E-16));
#16483=DIRECTION('center_axis',(1.79091352057933E-16,-2.24573452299033E-16,
1.));
#16484=DIRECTION('ref_axis',(-0.222520933956305,-0.974927912181826,-1.79091352057932E-16));
#16485=DIRECTION('center_axis',(1.79091352057933E-16,-2.24573452299033E-16,
1.));
#16486=DIRECTION('ref_axis',(-0.222520933956305,-0.974927912181826,-1.79091352057932E-16));
#16487=DIRECTION('center_axis',(1.43620113371564E-16,-6.91638013500039E-17,
1.));
#16488=DIRECTION('ref_axis',(1.,1.10509814492259E-33,-1.43620113371564E-16));
#16489=DIRECTION('center_axis',(1.43620113371564E-16,-6.91638013500039E-17,
1.));
#16490=DIRECTION('ref_axis',(1.,1.10509814492259E-33,-1.43620113371564E-16));
#16491=DIRECTION('center_axis',(0.974927912181826,-0.222520933956305,-2.24573452299033E-16));
#16492=DIRECTION('ref_axis',(1.64444757441797E-16,-2.8874437615686E-16,
1.));
#16493=DIRECTION('center_axis',(0.974927912181826,-0.222520933956305,-2.24573452299033E-16));
#16494=DIRECTION('ref_axis',(1.64444757441797E-16,-2.8874437615686E-16,
1.));
#16495=DIRECTION('center_axis',(0.781831482468022,0.623489801858743,-6.91638013500039E-17));
#16496=DIRECTION('ref_axis',(0.,0.,1.));
#16497=DIRECTION('center_axis',(0.781831482468022,0.623489801858743,-6.91638013500039E-17));
#16498=DIRECTION('ref_axis',(5.40744373425973E-17,4.31229247995114E-17,
1.));
#16499=DIRECTION('center_axis',(-0.623489801858743,0.781831482468022,0.));
#16500=DIRECTION('ref_axis',(0.,0.,-1.));
#16501=DIRECTION('center_axis',(0.781831482468022,0.623489801858743,-6.91638013500039E-17));
#16502=DIRECTION('ref_axis',(5.40744373425973E-17,4.31229247995114E-17,
1.));
#16503=DIRECTION('center_axis',(0.623489801858743,-0.781831482468022,1.22464679914735E-16));
#16504=DIRECTION('ref_axis',(0.,0.,1.));
#16505=DIRECTION('center_axis',(0.,0.,-1.));
#16506=DIRECTION('ref_axis',(1.,0.,0.));
#16507=DIRECTION('center_axis',(0.,0.,-1.));
#16508=DIRECTION('ref_axis',(1.,0.,0.));
#16509=DIRECTION('center_axis',(0.,0.,-1.));
#16510=DIRECTION('ref_axis',(1.,0.,0.));
#16511=DIRECTION('center_axis',(-0.781831482468022,-0.623489801858743,0.));
#16512=DIRECTION('ref_axis',(0.,0.,-1.));
#16513=DIRECTION('center_axis',(1.43620113371564E-16,-6.91638013500039E-17,
1.));
#16514=DIRECTION('ref_axis',(0.623489801858743,-0.781831482468022,-1.43620113371564E-16));
#16515=DIRECTION('center_axis',(1.43620113371564E-16,-6.91638013500039E-17,
1.));
#16516=DIRECTION('ref_axis',(0.623489801858743,-0.781831482468022,-1.43620113371564E-16));
#16517=DIRECTION('center_axis',(1.43620113371564E-16,-6.91638013500039E-17,
1.));
#16518=DIRECTION('ref_axis',(0.623489801858743,-0.781831482468022,-1.43620113371564E-16));
#16519=DIRECTION('center_axis',(0.781831482468022,0.623489801858743,-6.91638013500039E-17));
#16520=DIRECTION('ref_axis',(5.40744373425973E-17,4.31229247995114E-17,
1.));
#16521=DIRECTION('center_axis',(0.781831482468022,0.623489801858743,-6.91638013500039E-17));
#16522=DIRECTION('ref_axis',(5.40744373425973E-17,4.31229247995114E-17,
1.));
#16523=DIRECTION('center_axis',(1.,0.,1.22464679914735E-16));
#16524=DIRECTION('ref_axis',(-6.12323399573677E-17,0.,1.));
#16525=DIRECTION('center_axis',(-1.43620113371566E-16,-6.91638013500059E-17,
1.));
#16526=DIRECTION('ref_axis',(1.,-1.10509814492274E-33,1.43620113371566E-16));
#16527=DIRECTION('center_axis',(0.,-1.,0.));
#16528=DIRECTION('ref_axis',(6.12323399573677E-17,0.,-1.));
#16529=DIRECTION('center_axis',(0.,0.,1.));
#16530=DIRECTION('ref_axis',(1.,0.,0.));
#16531=DIRECTION('center_axis',(0.,0.,1.));
#16532=DIRECTION('ref_axis',(1.,0.,0.));
#16533=DIRECTION('center_axis',(0.,0.,1.));
#16534=DIRECTION('ref_axis',(1.,0.,0.));
#16535=DIRECTION('center_axis',(-1.43620113371566E-16,-6.91638013500059E-17,
1.));
#16536=DIRECTION('ref_axis',(1.,-1.10509814492274E-33,1.43620113371566E-16));
#16537=DIRECTION('center_axis',(-1.43620113371566E-16,-6.91638013500059E-17,
1.));
#16538=DIRECTION('ref_axis',(1.,-1.10509814492274E-33,1.43620113371566E-16));
#16539=DIRECTION('center_axis',(0.,1.,0.));
#16540=DIRECTION('ref_axis',(0.,0.,1.));
#16541=DIRECTION('center_axis',(0.,1.,0.));
#16542=DIRECTION('ref_axis',(0.,0.,1.));
#16543=DIRECTION('center_axis',(0.,1.,0.));
#16544=DIRECTION('ref_axis',(0.,0.,1.));
#16545=DIRECTION('center_axis',(0.,1.,0.));
#16546=DIRECTION('ref_axis',(0.,0.,1.));
#16547=DIRECTION('center_axis',(-1.,0.,1.22464679914735E-16));
#16548=DIRECTION('ref_axis',(-1.22464679914735E-16,0.,-1.));
#16549=DIRECTION('center_axis',(0.,1.,0.));
#16550=DIRECTION('ref_axis',(0.,0.,1.));
#16551=DIRECTION('center_axis',(0.,0.,-1.));
#16552=DIRECTION('ref_axis',(-1.,0.,0.));
#16553=DIRECTION('center_axis',(0.,0.,-1.));
#16554=DIRECTION('ref_axis',(1.,0.,0.));
#16555=DIRECTION('center_axis',(0.,0.,-1.));
#16556=DIRECTION('ref_axis',(1.,0.,0.));
#16557=DIRECTION('center_axis',(0.,0.,-1.));
#16558=DIRECTION('ref_axis',(-1.,0.,0.));
#16559=DIRECTION('center_axis',(0.,0.,1.));
#16560=DIRECTION('ref_axis',(1.,0.,0.));
#16561=DIRECTION('center_axis',(0.,0.,1.));
#16562=DIRECTION('ref_axis',(1.,0.,0.));
#16563=DIRECTION('center_axis',(0.,0.,1.));
#16564=DIRECTION('ref_axis',(1.,0.,0.));
#16565=DIRECTION('center_axis',(0.,0.,1.));
#16566=DIRECTION('ref_axis',(1.,0.,0.));
#16567=DIRECTION('center_axis',(0.,1.,0.));
#16568=DIRECTION('ref_axis',(0.,0.,1.));
#16569=DIRECTION('center_axis',(0.,-1.,0.));
#16570=DIRECTION('ref_axis',(0.,0.,-1.));
#16571=DIRECTION('center_axis',(0.,0.,1.));
#16572=DIRECTION('ref_axis',(1.,0.,0.));
#16573=DIRECTION('center_axis',(0.,0.,-1.));
#16574=DIRECTION('ref_axis',(1.,0.,0.));
#16575=DIRECTION('center_axis',(0.,0.,1.));
#16576=DIRECTION('ref_axis',(1.,0.,0.));
#16577=DIRECTION('center_axis',(0.,0.,1.));
#16578=DIRECTION('ref_axis',(1.,0.,0.));
#16579=DIRECTION('center_axis',(0.,0.,-1.));
#16580=DIRECTION('ref_axis',(1.,0.,0.));
#16581=DIRECTION('center_axis',(0.,0.,1.));
#16582=DIRECTION('ref_axis',(1.,0.,0.));
#16583=DIRECTION('center_axis',(0.,0.,-1.));
#16584=DIRECTION('ref_axis',(-1.,0.,0.));
#16585=DIRECTION('center_axis',(0.,0.,-1.));
#16586=DIRECTION('ref_axis',(-1.,0.,0.));
#16587=DIRECTION('center_axis',(-0.781831482468022,-0.623489801858743,6.91638013500039E-17));
#16588=DIRECTION('ref_axis',(-1.43620113371564E-16,6.91638013500039E-17,
-1.));
#16589=DIRECTION('center_axis',(0.781831482468022,0.623489801858743,-6.91638013500039E-17));
#16590=DIRECTION('ref_axis',(1.43620113371564E-16,-6.91638013500039E-17,
1.));
#16591=DIRECTION('center_axis',(1.43620113371564E-16,-6.91638013500039E-17,
1.));
#16592=DIRECTION('ref_axis',(0.623489801858743,-0.781831482468022,-1.43620113371564E-16));
#16593=DIRECTION('center_axis',(-1.43620113371564E-16,6.91638013500039E-17,
-1.));
#16594=DIRECTION('ref_axis',(0.623489801858743,-0.781831482468022,-1.43620113371564E-16));
#16595=DIRECTION('center_axis',(1.43620113371564E-16,-6.91638013500039E-17,
1.));
#16596=DIRECTION('ref_axis',(0.623489801858743,-0.781831482468022,-1.43620113371564E-16));
#16597=DIRECTION('center_axis',(1.43620113371564E-16,-6.91638013500039E-17,
1.));
#16598=DIRECTION('ref_axis',(0.623489801858743,-0.781831482468022,-1.43620113371564E-16));
#16599=DIRECTION('center_axis',(-1.43620113371564E-16,6.91638013500039E-17,
-1.));
#16600=DIRECTION('ref_axis',(0.623489801858743,-0.781831482468022,-1.43620113371564E-16));
#16601=DIRECTION('center_axis',(1.43620113371564E-16,-6.91638013500039E-17,
1.));
#16602=DIRECTION('ref_axis',(0.623489801858743,-0.781831482468022,-1.43620113371564E-16));
#16603=DIRECTION('center_axis',(-1.43620113371564E-16,6.91638013500039E-17,
-1.));
#16604=DIRECTION('ref_axis',(-0.623489801858743,0.781831482468022,1.43620113371564E-16));
#16605=DIRECTION('center_axis',(-1.43620113371564E-16,6.91638013500039E-17,
-1.));
#16606=DIRECTION('ref_axis',(-0.623489801858743,0.781831482468022,1.43620113371564E-16));
#16607=DIRECTION('center_axis',(-1.79091352057933E-16,2.24573452299033E-16,
-1.));
#16608=DIRECTION('ref_axis',(0.222520933956305,0.974927912181826,1.79091352057932E-16));
#16609=DIRECTION('center_axis',(-1.79091352057933E-16,2.24573452299033E-16,
-1.));
#16610=DIRECTION('ref_axis',(-0.222520933956305,-0.974927912181826,-1.79091352057932E-16));
#16611=DIRECTION('center_axis',(-1.79091352057933E-16,2.24573452299033E-16,
-1.));
#16612=DIRECTION('ref_axis',(-0.222520933956305,-0.974927912181826,-1.79091352057932E-16));
#16613=DIRECTION('center_axis',(-1.79091352057933E-16,2.24573452299033E-16,
-1.));
#16614=DIRECTION('ref_axis',(0.222520933956305,0.974927912181826,1.79091352057932E-16));
#16615=DIRECTION('center_axis',(1.79091352057933E-16,-2.24573452299033E-16,
1.));
#16616=DIRECTION('ref_axis',(-0.222520933956305,-0.974927912181826,-1.79091352057932E-16));
#16617=DIRECTION('center_axis',(1.79091352057933E-16,-2.24573452299033E-16,
1.));
#16618=DIRECTION('ref_axis',(-0.222520933956305,-0.974927912181826,-1.79091352057932E-16));
#16619=DIRECTION('center_axis',(1.79091352057933E-16,-2.24573452299033E-16,
1.));
#16620=DIRECTION('ref_axis',(-0.222520933956305,-0.974927912181826,-1.79091352057932E-16));
#16621=DIRECTION('center_axis',(1.79091352057933E-16,-2.24573452299033E-16,
1.));
#16622=DIRECTION('ref_axis',(-0.222520933956305,-0.974927912181826,-1.79091352057932E-16));
#16623=DIRECTION('center_axis',(-0.974927912181826,0.222520933956305,2.24573452299033E-16));
#16624=DIRECTION('ref_axis',(-1.79091352057933E-16,2.24573452299033E-16,
-1.));
#16625=DIRECTION('center_axis',(0.974927912181826,-0.222520933956305,-2.24573452299033E-16));
#16626=DIRECTION('ref_axis',(1.79091352057933E-16,-2.24573452299033E-16,
1.));
#16627=DIRECTION('center_axis',(1.79091352057933E-16,-2.24573452299033E-16,
1.));
#16628=DIRECTION('ref_axis',(-0.222520933956305,-0.974927912181826,-1.79091352057932E-16));
#16629=DIRECTION('center_axis',(-1.79091352057933E-16,2.24573452299033E-16,
-1.));
#16630=DIRECTION('ref_axis',(-0.222520933956305,-0.974927912181826,-1.79091352057932E-16));
#16631=DIRECTION('center_axis',(1.79091352057933E-16,-2.24573452299033E-16,
1.));
#16632=DIRECTION('ref_axis',(-0.222520933956305,-0.974927912181826,-1.79091352057932E-16));
#16633=DIRECTION('center_axis',(1.79091352057933E-16,-2.24573452299033E-16,
1.));
#16634=DIRECTION('ref_axis',(-0.222520933956305,-0.974927912181826,-1.79091352057932E-16));
#16635=DIRECTION('center_axis',(-1.79091352057933E-16,2.24573452299033E-16,
-1.));
#16636=DIRECTION('ref_axis',(-0.222520933956305,-0.974927912181826,-1.79091352057932E-16));
#16637=DIRECTION('center_axis',(1.79091352057933E-16,-2.24573452299033E-16,
1.));
#16638=DIRECTION('ref_axis',(-0.222520933956305,-0.974927912181826,-1.79091352057932E-16));
#16639=DIRECTION('center_axis',(-1.79091352057933E-16,2.24573452299033E-16,
-1.));
#16640=DIRECTION('ref_axis',(0.222520933956305,0.974927912181826,1.79091352057932E-16));
#16641=DIRECTION('center_axis',(-1.79091352057933E-16,2.24573452299033E-16,
-1.));
#16642=DIRECTION('ref_axis',(0.222520933956305,0.974927912181826,1.79091352057932E-16));
#16643=DIRECTION('center_axis',(-7.97031498468617E-17,3.49202315903319E-16,
-1.));
#16644=DIRECTION('ref_axis',(0.900968867902416,0.433883739117565,7.97031498468616E-17));
#16645=DIRECTION('center_axis',(-7.97031498468617E-17,3.49202315903319E-16,
-1.));
#16646=DIRECTION('ref_axis',(-0.900968867902416,-0.433883739117565,-7.97031498468616E-17));
#16647=DIRECTION('center_axis',(-7.97031498468617E-17,3.49202315903319E-16,
-1.));
#16648=DIRECTION('ref_axis',(-0.900968867902416,-0.433883739117565,-7.97031498468616E-17));
#16649=DIRECTION('center_axis',(-7.97031498468617E-17,3.49202315903319E-16,
-1.));
#16650=DIRECTION('ref_axis',(0.900968867902416,0.433883739117565,7.97031498468616E-17));
#16651=DIRECTION('center_axis',(7.97031498468617E-17,-3.49202315903319E-16,
1.));
#16652=DIRECTION('ref_axis',(-0.900968867902416,-0.433883739117565,-7.97031498468616E-17));
#16653=DIRECTION('center_axis',(7.97031498468617E-17,-3.49202315903319E-16,
1.));
#16654=DIRECTION('ref_axis',(-0.900968867902416,-0.433883739117565,-7.97031498468616E-17));
#16655=DIRECTION('center_axis',(7.97031498468617E-17,-3.49202315903319E-16,
1.));
#16656=DIRECTION('ref_axis',(-0.900968867902416,-0.433883739117565,-7.97031498468616E-17));
#16657=DIRECTION('center_axis',(7.97031498468617E-17,-3.49202315903319E-16,
1.));
#16658=DIRECTION('ref_axis',(-0.900968867902416,-0.433883739117565,-7.97031498468616E-17));
#16659=DIRECTION('center_axis',(-0.433883739117565,0.900968867902416,3.49202315903319E-16));
#16660=DIRECTION('ref_axis',(-7.97031498468617E-17,3.49202315903319E-16,
-1.));
#16661=DIRECTION('center_axis',(0.433883739117565,-0.900968867902416,-3.49202315903319E-16));
#16662=DIRECTION('ref_axis',(7.97031498468617E-17,-3.49202315903319E-16,
1.));
#16663=DIRECTION('center_axis',(7.97031498468617E-17,-3.49202315903319E-16,
1.));
#16664=DIRECTION('ref_axis',(-0.900968867902416,-0.433883739117565,-7.97031498468616E-17));
#16665=DIRECTION('center_axis',(-7.97031498468617E-17,3.49202315903319E-16,
-1.));
#16666=DIRECTION('ref_axis',(-0.900968867902416,-0.433883739117565,-7.97031498468616E-17));
#16667=DIRECTION('center_axis',(7.97031498468617E-17,-3.49202315903319E-16,
1.));
#16668=DIRECTION('ref_axis',(-0.900968867902416,-0.433883739117565,-7.97031498468616E-17));
#16669=DIRECTION('center_axis',(7.97031498468617E-17,-3.49202315903319E-16,
1.));
#16670=DIRECTION('ref_axis',(-0.900968867902416,-0.433883739117565,-7.97031498468616E-17));
#16671=DIRECTION('center_axis',(-7.97031498468617E-17,3.49202315903319E-16,
-1.));
#16672=DIRECTION('ref_axis',(-0.900968867902416,-0.433883739117565,-7.97031498468616E-17));
#16673=DIRECTION('center_axis',(7.97031498468617E-17,-3.49202315903319E-16,
1.));
#16674=DIRECTION('ref_axis',(-0.900968867902416,-0.433883739117565,-7.97031498468616E-17));
#16675=DIRECTION('center_axis',(-7.97031498468617E-17,3.49202315903319E-16,
-1.));
#16676=DIRECTION('ref_axis',(0.900968867902416,0.433883739117565,7.97031498468616E-17));
#16677=DIRECTION('center_axis',(-7.97031498468617E-17,3.49202315903319E-16,
-1.));
#16678=DIRECTION('ref_axis',(0.900968867902416,0.433883739117565,7.97031498468616E-17));
#16679=DIRECTION('center_axis',(7.97031498468594E-17,3.4920231590332E-16,
-1.));
#16680=DIRECTION('ref_axis',(0.900968867902422,-0.433883739117553,-7.97031498468594E-17));
#16681=DIRECTION('center_axis',(7.97031498468594E-17,3.4920231590332E-16,
-1.));
#16682=DIRECTION('ref_axis',(-0.900968867902422,0.433883739117553,7.97031498468594E-17));
#16683=DIRECTION('center_axis',(7.97031498468594E-17,3.4920231590332E-16,
-1.));
#16684=DIRECTION('ref_axis',(-0.900968867902422,0.433883739117553,7.97031498468594E-17));
#16685=DIRECTION('center_axis',(7.97031498468594E-17,3.4920231590332E-16,
-1.));
#16686=DIRECTION('ref_axis',(0.900968867902422,-0.433883739117553,-7.97031498468594E-17));
#16687=DIRECTION('center_axis',(-7.97031498468594E-17,-3.4920231590332E-16,
1.));
#16688=DIRECTION('ref_axis',(-0.900968867902422,0.433883739117553,7.97031498468594E-17));
#16689=DIRECTION('center_axis',(-7.97031498468594E-17,-3.4920231590332E-16,
1.));
#16690=DIRECTION('ref_axis',(-0.900968867902422,0.433883739117553,7.97031498468594E-17));
#16691=DIRECTION('center_axis',(-7.97031498468594E-17,-3.4920231590332E-16,
1.));
#16692=DIRECTION('ref_axis',(-0.900968867902422,0.433883739117553,7.97031498468594E-17));
#16693=DIRECTION('center_axis',(-7.97031498468594E-17,-3.4920231590332E-16,
1.));
#16694=DIRECTION('ref_axis',(-0.900968867902422,0.433883739117553,7.97031498468594E-17));
#16695=DIRECTION('center_axis',(0.433883739117553,0.900968867902422,3.4920231590332E-16));
#16696=DIRECTION('ref_axis',(7.97031498468594E-17,3.4920231590332E-16,-1.));
#16697=DIRECTION('center_axis',(-0.433883739117553,-0.900968867902422,-3.4920231590332E-16));
#16698=DIRECTION('ref_axis',(-7.97031498468594E-17,-3.4920231590332E-16,
1.));
#16699=DIRECTION('center_axis',(-7.97031498468594E-17,-3.4920231590332E-16,
1.));
#16700=DIRECTION('ref_axis',(-0.900968867902422,0.433883739117553,7.97031498468594E-17));
#16701=DIRECTION('center_axis',(7.97031498468594E-17,3.4920231590332E-16,
-1.));
#16702=DIRECTION('ref_axis',(-0.900968867902422,0.433883739117553,7.97031498468594E-17));
#16703=DIRECTION('center_axis',(-7.97031498468594E-17,-3.4920231590332E-16,
1.));
#16704=DIRECTION('ref_axis',(-0.900968867902422,0.433883739117553,7.97031498468594E-17));
#16705=DIRECTION('center_axis',(-7.97031498468594E-17,-3.4920231590332E-16,
1.));
#16706=DIRECTION('ref_axis',(-0.900968867902422,0.433883739117553,7.97031498468594E-17));
#16707=DIRECTION('center_axis',(7.97031498468594E-17,3.4920231590332E-16,
-1.));
#16708=DIRECTION('ref_axis',(-0.900968867902422,0.433883739117553,7.97031498468594E-17));
#16709=DIRECTION('center_axis',(-7.97031498468594E-17,-3.4920231590332E-16,
1.));
#16710=DIRECTION('ref_axis',(-0.900968867902422,0.433883739117553,7.97031498468594E-17));
#16711=DIRECTION('center_axis',(7.97031498468594E-17,3.4920231590332E-16,
-1.));
#16712=DIRECTION('ref_axis',(0.900968867902422,-0.433883739117553,-7.97031498468594E-17));
#16713=DIRECTION('center_axis',(7.97031498468594E-17,3.4920231590332E-16,
-1.));
#16714=DIRECTION('ref_axis',(0.900968867902422,-0.433883739117553,-7.97031498468594E-17));
#16715=DIRECTION('center_axis',(1.79091352057932E-16,2.24573452299036E-16,
-1.));
#16716=DIRECTION('ref_axis',(0.222520933956318,-0.974927912181823,-1.79091352057933E-16));
#16717=DIRECTION('center_axis',(1.79091352057932E-16,2.24573452299036E-16,
-1.));
#16718=DIRECTION('ref_axis',(-0.222520933956318,0.974927912181823,1.79091352057933E-16));
#16719=DIRECTION('center_axis',(1.79091352057932E-16,2.24573452299036E-16,
-1.));
#16720=DIRECTION('ref_axis',(-0.222520933956318,0.974927912181823,1.79091352057933E-16));
#16721=DIRECTION('center_axis',(1.79091352057932E-16,2.24573452299036E-16,
-1.));
#16722=DIRECTION('ref_axis',(0.222520933956318,-0.974927912181823,-1.79091352057933E-16));
#16723=DIRECTION('center_axis',(-1.79091352057932E-16,-2.24573452299036E-16,
1.));
#16724=DIRECTION('ref_axis',(-0.222520933956318,0.974927912181823,1.79091352057933E-16));
#16725=DIRECTION('center_axis',(-1.79091352057932E-16,-2.24573452299036E-16,
1.));
#16726=DIRECTION('ref_axis',(-0.222520933956318,0.974927912181823,1.79091352057933E-16));
#16727=DIRECTION('center_axis',(-1.79091352057932E-16,-2.24573452299036E-16,
1.));
#16728=DIRECTION('ref_axis',(-0.222520933956318,0.974927912181823,1.79091352057933E-16));
#16729=DIRECTION('center_axis',(-1.79091352057932E-16,-2.24573452299036E-16,
1.));
#16730=DIRECTION('ref_axis',(-0.222520933956318,0.974927912181823,1.79091352057933E-16));
#16731=DIRECTION('center_axis',(0.974927912181823,0.222520933956318,2.24573452299036E-16));
#16732=DIRECTION('ref_axis',(1.79091352057932E-16,2.24573452299036E-16,
-1.));
#16733=DIRECTION('center_axis',(-0.974927912181823,-0.222520933956318,-2.24573452299036E-16));
#16734=DIRECTION('ref_axis',(-1.79091352057932E-16,-2.24573452299036E-16,
1.));
#16735=DIRECTION('center_axis',(-1.79091352057932E-16,-2.24573452299036E-16,
1.));
#16736=DIRECTION('ref_axis',(-0.222520933956318,0.974927912181823,1.79091352057933E-16));
#16737=DIRECTION('center_axis',(1.79091352057932E-16,2.24573452299036E-16,
-1.));
#16738=DIRECTION('ref_axis',(-0.222520933956318,0.974927912181823,1.79091352057933E-16));
#16739=DIRECTION('center_axis',(-1.79091352057932E-16,-2.24573452299036E-16,
1.));
#16740=DIRECTION('ref_axis',(-0.222520933956318,0.974927912181823,1.79091352057933E-16));
#16741=DIRECTION('center_axis',(-1.79091352057932E-16,-2.24573452299036E-16,
1.));
#16742=DIRECTION('ref_axis',(-0.222520933956318,0.974927912181823,1.79091352057933E-16));
#16743=DIRECTION('center_axis',(1.79091352057932E-16,2.24573452299036E-16,
-1.));
#16744=DIRECTION('ref_axis',(-0.222520933956318,0.974927912181823,1.79091352057933E-16));
#16745=DIRECTION('center_axis',(-1.79091352057932E-16,-2.24573452299036E-16,
1.));
#16746=DIRECTION('ref_axis',(-0.222520933956318,0.974927912181823,1.79091352057933E-16));
#16747=DIRECTION('center_axis',(1.79091352057932E-16,2.24573452299036E-16,
-1.));
#16748=DIRECTION('ref_axis',(0.222520933956318,-0.974927912181823,-1.79091352057933E-16));
#16749=DIRECTION('center_axis',(1.79091352057932E-16,2.24573452299036E-16,
-1.));
#16750=DIRECTION('ref_axis',(0.222520933956318,-0.974927912181823,-1.79091352057933E-16));
#16751=DIRECTION('center_axis',(1.43620113371566E-16,6.91638013500059E-17,
-1.));
#16752=DIRECTION('ref_axis',(-0.623489801858732,-0.781831482468031,-1.43620113371566E-16));
#16753=DIRECTION('center_axis',(1.43620113371566E-16,6.91638013500059E-17,
-1.));
#16754=DIRECTION('ref_axis',(0.623489801858732,0.781831482468031,1.43620113371566E-16));
#16755=DIRECTION('center_axis',(1.43620113371566E-16,6.91638013500059E-17,
-1.));
#16756=DIRECTION('ref_axis',(0.623489801858732,0.781831482468031,1.43620113371566E-16));
#16757=DIRECTION('center_axis',(1.43620113371566E-16,6.91638013500059E-17,
-1.));
#16758=DIRECTION('ref_axis',(-0.623489801858732,-0.781831482468031,-1.43620113371566E-16));
#16759=DIRECTION('center_axis',(-1.43620113371566E-16,-6.91638013500059E-17,
1.));
#16760=DIRECTION('ref_axis',(0.623489801858732,0.781831482468031,1.43620113371566E-16));
#16761=DIRECTION('center_axis',(-1.43620113371566E-16,-6.91638013500059E-17,
1.));
#16762=DIRECTION('ref_axis',(0.623489801858732,0.781831482468031,1.43620113371566E-16));
#16763=DIRECTION('center_axis',(-1.43620113371566E-16,-6.91638013500059E-17,
1.));
#16764=DIRECTION('ref_axis',(0.623489801858732,0.781831482468031,1.43620113371566E-16));
#16765=DIRECTION('center_axis',(-1.43620113371566E-16,-6.91638013500059E-17,
1.));
#16766=DIRECTION('ref_axis',(0.623489801858732,0.781831482468031,1.43620113371566E-16));
#16767=DIRECTION('center_axis',(0.781831482468031,-0.623489801858732,6.91638013500059E-17));
#16768=DIRECTION('ref_axis',(1.43620113371566E-16,6.91638013500061E-17,
-1.));
#16769=DIRECTION('center_axis',(-0.781831482468031,0.623489801858732,-6.91638013500059E-17));
#16770=DIRECTION('ref_axis',(-1.43620113371566E-16,-6.91638013500061E-17,
1.));
#16771=DIRECTION('center_axis',(-1.43620113371566E-16,-6.91638013500059E-17,
1.));
#16772=DIRECTION('ref_axis',(0.623489801858732,0.781831482468031,1.43620113371566E-16));
#16773=DIRECTION('center_axis',(1.43620113371566E-16,6.91638013500059E-17,
-1.));
#16774=DIRECTION('ref_axis',(0.623489801858732,0.781831482468031,1.43620113371566E-16));
#16775=DIRECTION('center_axis',(-1.43620113371566E-16,-6.91638013500059E-17,
1.));
#16776=DIRECTION('ref_axis',(0.623489801858732,0.781831482468031,1.43620113371566E-16));
#16777=DIRECTION('center_axis',(-1.43620113371566E-16,-6.91638013500059E-17,
1.));
#16778=DIRECTION('ref_axis',(0.623489801858732,0.781831482468031,1.43620113371566E-16));
#16779=DIRECTION('center_axis',(1.43620113371566E-16,6.91638013500059E-17,
-1.));
#16780=DIRECTION('ref_axis',(0.623489801858732,0.781831482468031,1.43620113371566E-16));
#16781=DIRECTION('center_axis',(-1.43620113371566E-16,-6.91638013500059E-17,
1.));
#16782=DIRECTION('ref_axis',(0.623489801858732,0.781831482468031,1.43620113371566E-16));
#16783=DIRECTION('center_axis',(1.43620113371566E-16,6.91638013500059E-17,
-1.));
#16784=DIRECTION('ref_axis',(-0.623489801858732,-0.781831482468031,-1.43620113371566E-16));
#16785=DIRECTION('center_axis',(1.43620113371566E-16,6.91638013500059E-17,
-1.));
#16786=DIRECTION('ref_axis',(-0.623489801858732,-0.781831482468031,-1.43620113371566E-16));
#16787=DIRECTION('center_axis',(0.,0.,1.));
#16788=DIRECTION('ref_axis',(1.,0.,0.));
#16789=DIRECTION('center_axis',(0.,0.,-1.));
#16790=DIRECTION('ref_axis',(1.,0.,0.));
#16791=DIRECTION('center_axis',(0.,0.,1.));
#16792=DIRECTION('ref_axis',(1.,0.,0.));
#16793=DIRECTION('center_axis',(0.,0.,1.));
#16794=DIRECTION('ref_axis',(1.,0.,0.));
#16795=DIRECTION('center_axis',(0.,0.,-1.));
#16796=DIRECTION('ref_axis',(1.,0.,0.));
#16797=DIRECTION('center_axis',(0.,0.,1.));
#16798=DIRECTION('ref_axis',(1.,0.,0.));
#16799=DIRECTION('center_axis',(0.,0.,-1.));
#16800=DIRECTION('ref_axis',(-1.,0.,0.));
#16801=DIRECTION('center_axis',(0.,0.,-1.));
#16802=DIRECTION('ref_axis',(-1.,0.,0.));
#16803=DIRECTION('axis',(0.,0.,1.));
#16804=DIRECTION('refdir',(1.,0.,0.));
#16805=DIRECTION('center_axis',(0.,-1.83697019872103E-16,1.));
#16806=DIRECTION('ref_axis',(0.,-1.,-1.83697019872103E-16));
#16807=DIRECTION('center_axis',(0.,-1.83697019872103E-16,1.));
#16808=DIRECTION('ref_axis',(0.,-1.,-1.83697019872103E-16));
#16809=DIRECTION('center_axis',(1.,1.22464679914735E-16,2.24963967399279E-32));
#16810=DIRECTION('ref_axis',(-1.22464679914735E-16,1.,1.83697019872103E-16));
#16811=DIRECTION('center_axis',(0.,-1.83697019872103E-16,1.));
#16812=DIRECTION('ref_axis',(0.,-1.,-1.83697019872103E-16));
#16813=DIRECTION('center_axis',(0.,1.83697019872103E-16,-1.));
#16814=DIRECTION('ref_axis',(0.,1.,2.09599627067876E-16));
#16815=DIRECTION('center_axis',(0.,1.83697019872103E-16,-1.));
#16816=DIRECTION('ref_axis',(0.,1.,1.83697019872103E-16));
#16817=DIRECTION('center_axis',(0.,1.83697019872103E-16,-1.));
#16818=DIRECTION('ref_axis',(0.,1.,1.83697019872103E-16));
#16819=DIRECTION('center_axis',(-1.,1.22464679914735E-16,2.24963967399279E-32));
#16820=DIRECTION('ref_axis',(-1.22464679914735E-16,-1.,-1.30999766917423E-16));
#16821=DIRECTION('center_axis',(0.,-1.83697019872103E-16,1.));
#16822=DIRECTION('ref_axis',(0.,1.,1.83697019872103E-16));
#16823=DIRECTION('center_axis',(0.,-1.83697019872103E-16,1.));
#16824=DIRECTION('ref_axis',(0.,1.,1.83697019872103E-16));
#16825=DIRECTION('center_axis',(0.,1.83697019872103E-16,-1.));
#16826=DIRECTION('ref_axis',(0.,1.,2.09599627067876E-16));
#16827=DIRECTION('center_axis',(0.,1.83697019872103E-16,-1.));
#16828=DIRECTION('ref_axis',(0.,1.,1.83697019872103E-16));
#16829=DIRECTION('center_axis',(0.,1.83697019872103E-16,-1.));
#16830=DIRECTION('ref_axis',(0.,1.,1.83697019872103E-16));
#16831=DIRECTION('center_axis',(-1.,1.22464679914735E-16,2.24963967399279E-32));
#16832=DIRECTION('ref_axis',(-1.22464679914735E-16,-1.,-1.30999766917423E-16));
#16833=DIRECTION('center_axis',(0.,-1.83697019872103E-16,1.));
#16834=DIRECTION('ref_axis',(0.,-1.,-1.83697019872103E-16));
#16835=DIRECTION('center_axis',(0.,-1.83697019872103E-16,1.));
#16836=DIRECTION('ref_axis',(0.,-1.,-1.83697019872103E-16));
#16837=DIRECTION('',(-8.65956056235483E-17,0.707106781186539,0.707106781186556));
#16838=DIRECTION('center_axis',(0.,-1.83697019872103E-16,1.));
#16839=DIRECTION('ref_axis',(0.,-1.,-1.83697019872103E-16));
#16840=DIRECTION('center_axis',(0.,-1.83697019872103E-16,1.));
#16841=DIRECTION('ref_axis',(0.,-1.,-1.83697019872103E-16));
#16842=DIRECTION('',(0.,-1.83697019872103E-16,1.));
#16843=DIRECTION('center_axis',(0.,1.83697019872103E-16,-1.));
#16844=DIRECTION('ref_axis',(0.,1.,1.83697019872103E-16));
#16845=DIRECTION('',(-8.65956056235483E-17,-0.707106781186539,-0.707106781186556));
#16846=DIRECTION('center_axis',(0.,-1.83697019872103E-16,1.));
#16847=DIRECTION('ref_axis',(0.,-1.,-1.83697019872103E-16));
#16848=DIRECTION('center_axis',(0.,-1.83697019872103E-16,1.));
#16849=DIRECTION('ref_axis',(0.,-1.,-1.83697019872103E-16));
#16850=DIRECTION('',(0.,1.83697019872103E-16,-1.));
#16851=DIRECTION('center_axis',(0.,-1.83697019872103E-16,1.));
#16852=DIRECTION('ref_axis',(0.,-1.,-1.83697019872103E-16));
#16853=DIRECTION('center_axis',(0.,-1.83697019872103E-16,1.));
#16854=DIRECTION('ref_axis',(0.,-1.,-1.83697019872103E-16));
#16855=DIRECTION('center_axis',(0.,-1.83697019872103E-16,1.));
#16856=DIRECTION('ref_axis',(0.,-1.,-1.83697019872103E-16));
#16857=DIRECTION('',(0.,1.83697019872103E-16,-1.));
#16858=DIRECTION('center_axis',(0.,1.83697019872103E-16,-1.));
#16859=DIRECTION('ref_axis',(0.,1.,1.83697019872103E-16));
#16860=DIRECTION('center_axis',(0.,-1.83697019872103E-16,1.));
#16861=DIRECTION('ref_axis',(0.,-1.,-1.83697019872103E-16));
#16862=DIRECTION('center_axis',(-1.,0.,0.));
#16863=DIRECTION('ref_axis',(0.,1.,0.));
#16864=DIRECTION('center_axis',(0.,1.22464679914735E-16,1.));
#16865=DIRECTION('ref_axis',(0.,-1.,1.22464679914735E-16));
#16866=DIRECTION('center_axis',(-0.623489801858732,0.781831482468031,1.43620113371566E-16));
#16867=DIRECTION('ref_axis',(0.781831482468031,0.623489801858732,-6.91638013500061E-17));
#16868=DIRECTION('center_axis',(2.39366855619276E-16,7.19167766472515E-18,
1.));
#16869=DIRECTION('ref_axis',(-0.781831482468031,-0.623489801858732,1.91628481264741E-16));
#16870=DIRECTION('center_axis',(0.222520933956319,0.974927912181823,1.79091352057932E-16));
#16871=DIRECTION('ref_axis',(0.974927912181823,-0.222520933956319,-2.24573452299036E-16));
#16872=DIRECTION('center_axis',(2.98485586763221E-16,-2.51824407250324E-16,
1.));
#16873=DIRECTION('ref_axis',(-0.974927912181823,0.222520933956319,3.47038132213772E-16));
#16874=DIRECTION('center_axis',(0.900968867902422,0.433883739117552,7.97031498468594E-17));
#16875=DIRECTION('ref_axis',(0.433883739117552,-0.900968867902422,-3.4920231590332E-16));
#16876=DIRECTION('center_axis',(1.32838583078098E-16,-4.59539179924132E-16,
1.));
#16877=DIRECTION('ref_axis',(-0.433883739117552,0.900968867902422,4.71666995818055E-16));
#16878=DIRECTION('center_axis',(0.900968867902416,-0.433883739117565,-7.97031498468616E-17));
#16879=DIRECTION('ref_axis',(-0.433883739117565,-0.900968867902416,-3.49202315903319E-16));
#16880=DIRECTION('center_axis',(-1.32838583078103E-16,-4.5953917992413E-16,
1.));
#16881=DIRECTION('ref_axis',(0.433883739117565,0.900968867902416,4.71666995818054E-16));
#16882=DIRECTION('center_axis',(0.222520933956305,-0.974927912181826,-1.79091352057933E-16));
#16883=DIRECTION('ref_axis',(-0.974927912181826,-0.222520933956305,-2.24573452299033E-16));
#16884=DIRECTION('center_axis',(-2.98485586763221E-16,-2.5182440725032E-16,
1.));
#16885=DIRECTION('ref_axis',(0.974927912181826,0.222520933956305,3.47038132213768E-16));
#16886=DIRECTION('center_axis',(-0.623489801858743,-0.781831482468022,-1.43620113371564E-16));
#16887=DIRECTION('ref_axis',(-0.781831482468022,0.623489801858743,-6.91638013500039E-17));
#16888=DIRECTION('center_axis',(-2.39366855619273E-16,7.19167766472869E-18,
1.));
#16889=DIRECTION('ref_axis',(0.781831482468022,-0.623489801858743,1.91628481264739E-16));
#16890=DIRECTION('center_axis',(0.,1.83697019872103E-16,-1.));
#16891=DIRECTION('ref_axis',(0.,1.,1.62614292875575E-16));
#16892=DIRECTION('center_axis',(0.,1.83697019872103E-16,-1.));
#16893=DIRECTION('ref_axis',(0.,1.,1.83697019872103E-16));
#16894=DIRECTION('center_axis',(-1.,1.22464679914735E-16,2.24963967399279E-32));
#16895=DIRECTION('ref_axis',(-1.22464679914735E-16,-1.,-2.03267866094469E-16));
#16896=DIRECTION('center_axis',(0.,-1.83697019872103E-16,1.));
#16897=DIRECTION('ref_axis',(0.,1.,1.83697019872103E-16));
#16898=DIRECTION('center_axis',(0.,-1.83697019872103E-16,1.));
#16899=DIRECTION('ref_axis',(0.,1.,1.83697019872103E-16));
#16900=DIRECTION('center_axis',(0.,-1.83697019872103E-16,1.));
#16901=DIRECTION('ref_axis',(0.,-1.,-1.64970202400831E-16));
#16902=DIRECTION('center_axis',(0.,-1.83697019872103E-16,1.));
#16903=DIRECTION('ref_axis',(0.,-1.,-1.83697019872103E-16));
#16904=DIRECTION('center_axis',(-1.,-1.22464679914735E-16,-2.24963967399279E-32));
#16905=DIRECTION('ref_axis',(-1.22464679914735E-16,1.,2.06212753001039E-16));
#16906=DIRECTION('center_axis',(0.,1.83697019872103E-16,-1.));
#16907=DIRECTION('ref_axis',(0.,-1.,-1.83697019872103E-16));
#16908=DIRECTION('center_axis',(0.,-1.83697019872103E-16,1.));
#16909=DIRECTION('ref_axis',(0.,-1.,-1.62614292875575E-16));
#16910=DIRECTION('center_axis',(0.,-1.83697019872103E-16,1.));
#16911=DIRECTION('ref_axis',(0.,-1.,-1.83697019872103E-16));
#16912=DIRECTION('center_axis',(-1.,-1.22464679914735E-16,-2.24963967399279E-32));
#16913=DIRECTION('ref_axis',(-1.22464679914735E-16,1.,2.03267866094469E-16));
#16914=DIRECTION('center_axis',(0.,1.83697019872103E-16,-1.));
#16915=DIRECTION('ref_axis',(0.,-1.,-1.83697019872103E-16));
#16916=DIRECTION('center_axis',(0.,1.83697019872103E-16,-1.));
#16917=DIRECTION('ref_axis',(0.,1.,1.64970202400831E-16));
#16918=DIRECTION('center_axis',(0.,1.83697019872103E-16,-1.));
#16919=DIRECTION('ref_axis',(0.,1.,1.83697019872103E-16));
#16920=DIRECTION('center_axis',(0.,1.83697019872103E-16,-1.));
#16921=DIRECTION('ref_axis',(0.,1.,1.83697019872103E-16));
#16922=DIRECTION('center_axis',(-1.,1.22464679914735E-16,2.24963967399279E-32));
#16923=DIRECTION('ref_axis',(-1.22464679914735E-16,-1.,-2.06212753001039E-16));
#16924=DIRECTION('center_axis',(0.,-1.83697019872103E-16,1.));
#16925=DIRECTION('ref_axis',(0.,1.,1.83697019872103E-16));
#16926=DIRECTION('center_axis',(0.,-1.83697019872103E-16,1.));
#16927=DIRECTION('ref_axis',(0.,-1.,-1.83697019872103E-16));
#16928=DIRECTION('center_axis',(0.,-1.83697019872103E-16,1.));
#16929=DIRECTION('ref_axis',(0.,-1.,-1.83697019872103E-16));
#16930=DIRECTION('',(0.,-1.83697019872103E-16,1.));
#16931=DIRECTION('center_axis',(0.,-1.83697019872103E-16,1.));
#16932=DIRECTION('ref_axis',(0.,-1.,-1.83697019872103E-16));
#16933=DIRECTION('center_axis',(0.,-1.83697019872103E-16,1.));
#16934=DIRECTION('ref_axis',(0.,-1.,-1.83697019872103E-16));
#16935=DIRECTION('center_axis',(0.,-1.83697019872103E-16,1.));
#16936=DIRECTION('ref_axis',(0.,-1.,-1.83697019872103E-16));
#16937=DIRECTION('',(0.,-1.83697019872103E-16,1.));
#16938=DIRECTION('center_axis',(0.,-1.83697019872103E-16,1.));
#16939=DIRECTION('ref_axis',(0.,-1.,-1.83697019872103E-16));
#16940=DIRECTION('',(0.,-1.83697019872103E-16,1.));
#16941=DIRECTION('center_axis',(0.,-1.83697019872103E-16,1.));
#16942=DIRECTION('ref_axis',(0.,-1.,-1.83697019872103E-16));
#16943=DIRECTION('center_axis',(0.,-1.83697019872103E-16,1.));
#16944=DIRECTION('ref_axis',(0.,-1.,-1.83697019872103E-16));
#16945=DIRECTION('center_axis',(1.,1.22464679914735E-16,2.24963967399279E-32));
#16946=DIRECTION('ref_axis',(-1.22464679914735E-16,1.,1.83697019872103E-16));
#16947=DIRECTION('center_axis',(0.,-1.83697019872103E-16,1.));
#16948=DIRECTION('ref_axis',(0.,-1.,-1.83697019872103E-16));
#16949=DIRECTION('center_axis',(0.,-1.83697019872103E-16,1.));
#16950=DIRECTION('ref_axis',(0.,-1.,-1.83697019872103E-16));
#16951=DIRECTION('',(0.,-1.83697019872103E-16,1.));
#16952=DIRECTION('center_axis',(0.,-1.83697019872103E-16,1.));
#16953=DIRECTION('ref_axis',(0.,-1.,-1.83697019872103E-16));
#16954=DIRECTION('',(0.,-1.83697019872103E-16,1.));
#16955=DIRECTION('center_axis',(0.,-1.83697019872103E-16,1.));
#16956=DIRECTION('ref_axis',(0.,-1.,-1.83697019872103E-16));
#16957=DIRECTION('center_axis',(0.,-1.83697019872103E-16,1.));
#16958=DIRECTION('ref_axis',(0.,-1.,-1.83697019872103E-16));
#16959=DIRECTION('center_axis',(0.,-1.83697019872103E-16,1.));
#16960=DIRECTION('ref_axis',(0.,-1.,-1.83697019872103E-16));
#16961=DIRECTION('',(0.,-1.83697019872103E-16,1.));
#16962=DIRECTION('center_axis',(0.,-1.83697019872103E-16,1.));
#16963=DIRECTION('ref_axis',(0.,-1.,-1.83697019872103E-16));
#16964=DIRECTION('center_axis',(0.,-1.83697019872103E-16,1.));
#16965=DIRECTION('ref_axis',(0.,-1.,-1.83697019872103E-16));
#16966=DIRECTION('center_axis',(0.,-1.83697019872103E-16,1.));
#16967=DIRECTION('ref_axis',(0.,-1.,-1.83697019872103E-16));
#16968=DIRECTION('',(8.65956056235488E-17,-0.707106781186543,-0.707106781186552));
#16969=DIRECTION('center_axis',(0.,-1.83697019872103E-16,1.));
#16970=DIRECTION('ref_axis',(0.,-1.,-1.83697019872103E-16));
#16971=DIRECTION('center_axis',(0.,1.83697019872103E-16,-1.));
#16972=DIRECTION('ref_axis',(0.,1.,1.83697019872103E-16));
#16973=DIRECTION('center_axis',(0.,-1.83697019872103E-16,1.));
#16974=DIRECTION('ref_axis',(0.,-1.,-1.83697019872103E-16));
#16975=DIRECTION('',(8.65956056235488E-17,0.707106781186543,0.707106781186552));
#16976=DIRECTION('center_axis',(0.,-1.83697019872103E-16,1.));
#16977=DIRECTION('ref_axis',(0.,-1.,-1.83697019872103E-16));
#16978=DIRECTION('center_axis',(0.,-1.83697019872103E-16,1.));
#16979=DIRECTION('ref_axis',(0.,-1.,-1.83697019872103E-16));
#16980=DIRECTION('center_axis',(0.,-1.83697019872103E-16,1.));
#16981=DIRECTION('ref_axis',(0.,-1.,-1.83697019872103E-16));
#16982=DIRECTION('',(0.,1.83697019872103E-16,-1.));
#16983=DIRECTION('center_axis',(0.,1.83697019872103E-16,-1.));
#16984=DIRECTION('ref_axis',(0.,1.,1.83697019872103E-16));
#16985=DIRECTION('center_axis',(0.,-1.83697019872103E-16,1.));
#16986=DIRECTION('ref_axis',(0.,-1.,-1.83697019872103E-16));
#16987=DIRECTION('center_axis',(0.,1.83697019872103E-16,-1.));
#16988=DIRECTION('ref_axis',(0.,1.,1.83697019872103E-16));
#16989=DIRECTION('center_axis',(0.,-1.83697019872103E-16,1.));
#16990=DIRECTION('ref_axis',(0.,-1.,-1.83697019872103E-16));
#16991=DIRECTION('center_axis',(0.,1.83697019872103E-16,-1.));
#16992=DIRECTION('ref_axis',(0.,1.,1.83697019872103E-16));
#16993=DIRECTION('center_axis',(0.,-1.83697019872103E-16,1.));
#16994=DIRECTION('ref_axis',(0.,-1.,-1.83697019872103E-16));
#16995=DIRECTION('center_axis',(-0.781831482468031,0.623489801858732,-6.91638013500059E-17));
#16996=DIRECTION('ref_axis',(0.,0.,1.));
#16997=DIRECTION('center_axis',(-0.781831482468031,0.623489801858732,-6.91638013500059E-17));
#16998=DIRECTION('ref_axis',(-5.40744373425995E-17,4.31229247995119E-17,
1.));
#16999=DIRECTION('center_axis',(-0.623489801858732,-0.781831482468031,2.05955304247937E-16));
#17000=DIRECTION('ref_axis',(0.,-2.63426721571497E-16,-1.));
#17001=DIRECTION('center_axis',(-0.781831482468031,0.623489801858732,-6.91638013500059E-17));
#17002=DIRECTION('ref_axis',(-5.40744373425995E-17,4.31229247995119E-17,
1.));
#17003=DIRECTION('center_axis',(0.623489801858732,0.781831482468031,1.22464679914735E-16));
#17004=DIRECTION('ref_axis',(0.,0.,1.));
#17005=DIRECTION('center_axis',(-1.79091352057932E-16,-2.24573452299036E-16,
1.));
#17006=DIRECTION('ref_axis',(-5.50003967499518E-33,-1.,-2.24573452299036E-16));
#17007=DIRECTION('center_axis',(0.781831482468031,-0.623489801858732,0.));
#17008=DIRECTION('ref_axis',(0.,0.,-1.));
#17009=DIRECTION('center_axis',(-1.43620113371566E-16,-6.91638013500059E-17,
1.));
#17010=DIRECTION('ref_axis',(0.623489801858732,0.781831482468031,1.43620113371566E-16));
#17011=DIRECTION('center_axis',(-1.43620113371566E-16,-6.91638013500059E-17,
1.));
#17012=DIRECTION('ref_axis',(0.623489801858732,0.781831482468031,1.43620113371566E-16));
#17013=DIRECTION('center_axis',(-1.43620113371566E-16,-6.91638013500059E-17,
1.));
#17014=DIRECTION('ref_axis',(0.623489801858732,0.781831482468031,1.43620113371566E-16));
#17015=DIRECTION('center_axis',(-1.79091352057932E-16,-2.24573452299036E-16,
1.));
#17016=DIRECTION('ref_axis',(-5.50003967499518E-33,-1.,-2.24573452299036E-16));
#17017=DIRECTION('center_axis',(-1.79091352057932E-16,-2.24573452299036E-16,
1.));
#17018=DIRECTION('ref_axis',(-5.5000396749952E-33,-1.,-2.24573452299036E-16));
#17019=DIRECTION('center_axis',(-0.781831482468031,0.623489801858732,-6.91638013500059E-17));
#17020=DIRECTION('ref_axis',(-5.40744373425995E-17,4.31229247995119E-17,
1.));
#17021=DIRECTION('center_axis',(-0.781831482468031,0.623489801858732,-6.91638013500059E-17));
#17022=DIRECTION('ref_axis',(-5.40744373425995E-17,4.31229247995119E-17,
1.));
#17023=DIRECTION('center_axis',(-0.974927912181823,-0.222520933956318,-2.24573452299036E-16));
#17024=DIRECTION('ref_axis',(0.,-2.10741377257197E-16,1.));
#17025=DIRECTION('center_axis',(-0.974927912181823,-0.222520933956318,-2.24573452299036E-16));
#17026=DIRECTION('ref_axis',(-1.71433215598957E-16,-2.58125940401653E-16,
1.));
#17027=DIRECTION('center_axis',(0.222520933956318,-0.974927912181823,-1.28411031837301E-16));
#17028=DIRECTION('ref_axis',(0.,1.31713360785748E-16,-1.));
#17029=DIRECTION('center_axis',(-0.974927912181823,-0.222520933956318,-2.24573452299036E-16));
#17030=DIRECTION('ref_axis',(-1.71433215598957E-16,-2.58125940401653E-16,
1.));
#17031=DIRECTION('center_axis',(-0.222520933956318,0.974927912181823,3.59586625308286E-16));
#17032=DIRECTION('ref_axis',(0.,-2.4905725751517E-16,1.));
#17033=DIRECTION('center_axis',(-7.97031498468594E-17,-3.4920231590332E-16,
1.));
#17034=DIRECTION('ref_axis',(2.39882519785021E-33,-1.,-3.4920231590332E-16));
#17035=DIRECTION('center_axis',(0.974927912181823,0.222520933956318,6.92755669385935E-17));
#17036=DIRECTION('ref_axis',(0.,3.11321571893962E-16,-1.));
#17037=DIRECTION('center_axis',(-1.79091352057932E-16,-2.24573452299036E-16,
1.));
#17038=DIRECTION('ref_axis',(-0.222520933956318,0.974927912181823,1.79091352057933E-16));
#17039=DIRECTION('center_axis',(-1.79091352057932E-16,-2.24573452299036E-16,
1.));
#17040=DIRECTION('ref_axis',(-0.222520933956318,0.974927912181823,1.79091352057933E-16));
#17041=DIRECTION('center_axis',(-1.79091352057932E-16,-2.24573452299036E-16,
1.));
#17042=DIRECTION('ref_axis',(-0.222520933956318,0.974927912181823,1.79091352057933E-16));
#17043=DIRECTION('center_axis',(-7.97031498468594E-17,-3.4920231590332E-16,
1.));
#17044=DIRECTION('ref_axis',(2.39882519785021E-33,-1.,-3.4920231590332E-16));
#17045=DIRECTION('center_axis',(-7.97031498468594E-17,-3.4920231590332E-16,
1.));
#17046=DIRECTION('ref_axis',(2.39882519785021E-33,-1.,-3.4920231590332E-16));
#17047=DIRECTION('center_axis',(-0.974927912181823,-0.222520933956318,-2.24573452299036E-16));
#17048=DIRECTION('ref_axis',(-1.64444757441796E-16,-2.88744376156862E-16,
1.));
#17049=DIRECTION('center_axis',(-0.974927912181823,-0.222520933956318,-2.24573452299036E-16));
#17050=DIRECTION('ref_axis',(-1.64444757441796E-16,-2.88744376156862E-16,
1.));
#17051=DIRECTION('center_axis',(-0.433883739117553,-0.900968867902422,-3.4920231590332E-16));
#17052=DIRECTION('ref_axis',(0.,-4.21482754514395E-16,1.));
#17053=DIRECTION('center_axis',(-0.433883739117553,-0.900968867902422,-3.4920231590332E-16));
#17054=DIRECTION('ref_axis',(1.97058769816641E-17,-3.97075180104293E-16,
1.));
#17055=DIRECTION('center_axis',(0.900968867902422,-0.433883739117553,-2.28593141877839E-16));
#17056=DIRECTION('ref_axis',(0.,5.26853443142994E-16,-1.));
#17057=DIRECTION('center_axis',(-0.433883739117553,-0.900968867902422,-3.4920231590332E-16));
#17058=DIRECTION('ref_axis',(1.97058769816641E-17,-3.97075180104293E-16,
1.));
#17059=DIRECTION('center_axis',(-0.900968867902422,0.433883739117552,3.33523066916777E-16));
#17060=DIRECTION('ref_axis',(0.,-4.9811451503034E-16,1.));
#17061=DIRECTION('center_axis',(7.97031498468617E-17,-3.49202315903319E-16,
1.));
#17062=DIRECTION('ref_axis',(-2.39882519785018E-33,-1.,-3.49202315903319E-16));
#17063=DIRECTION('center_axis',(0.433883739117552,0.900968867902422,5.60982088365811E-16));
#17064=DIRECTION('ref_axis',(0.,6.22643143787925E-16,-1.));
#17065=DIRECTION('center_axis',(-7.97031498468594E-17,-3.4920231590332E-16,
1.));
#17066=DIRECTION('ref_axis',(-0.900968867902422,0.433883739117553,7.97031498468594E-17));
#17067=DIRECTION('center_axis',(-7.97031498468594E-17,-3.4920231590332E-16,
1.));
#17068=DIRECTION('ref_axis',(-0.900968867902422,0.433883739117553,7.97031498468594E-17));
#17069=DIRECTION('center_axis',(-7.97031498468594E-17,-3.4920231590332E-16,
1.));
#17070=DIRECTION('ref_axis',(-0.900968867902422,0.433883739117553,7.97031498468594E-17));
#17071=DIRECTION('center_axis',(7.97031498468617E-17,-3.49202315903319E-16,
1.));
#17072=DIRECTION('ref_axis',(-2.39882519785018E-33,-1.,-3.49202315903319E-16));
#17073=DIRECTION('center_axis',(7.97031498468617E-17,-3.49202315903319E-16,
1.));
#17074=DIRECTION('ref_axis',(-2.39882519785018E-33,-1.,-3.49202315903319E-16));
#17075=DIRECTION('center_axis',(-0.433883739117553,-0.900968867902422,-3.4920231590332E-16));
#17076=DIRECTION('ref_axis',(4.4891409918625E-17,-4.09203893527874E-16,
1.));
#17077=DIRECTION('center_axis',(-0.433883739117553,-0.900968867902422,-3.4920231590332E-16));
#17078=DIRECTION('ref_axis',(4.48914099186251E-17,-4.09203893527874E-16,
1.));
#17079=DIRECTION('center_axis',(0.433883739117565,-0.900968867902416,-3.49202315903319E-16));
#17080=DIRECTION('ref_axis',(0.,-4.21482754514395E-16,1.));
#17081=DIRECTION('center_axis',(0.433883739117565,-0.900968867902416,-3.49202315903319E-16));
#17082=DIRECTION('ref_axis',(-1.97058769816642E-17,-3.97075180104295E-16,
1.));
#17083=DIRECTION('center_axis',(0.900968867902416,0.433883739117565,2.28593141877845E-16));
#17084=DIRECTION('ref_axis',(0.,5.26853443142994E-16,-1.));
#17085=DIRECTION('center_axis',(0.433883739117565,-0.900968867902416,-3.49202315903319E-16));
#17086=DIRECTION('ref_axis',(-1.97058769816642E-17,-3.97075180104295E-16,
1.));
#17087=DIRECTION('center_axis',(-0.900968867902416,-0.433883739117565,-8.85937070873124E-17));
#17088=DIRECTION('ref_axis',(0.,-4.9811451503034E-16,1.));
#17089=DIRECTION('center_axis',(1.79091352057933E-16,-2.24573452299033E-16,
1.));
#17090=DIRECTION('ref_axis',(5.50003967499563E-33,-1.,-2.24573452299033E-16));
#17091=DIRECTION('center_axis',(-0.433883739117565,0.900968867902416,5.60982088365808E-16));
#17092=DIRECTION('ref_axis',(0.,6.22643143787925E-16,-1.));
#17093=DIRECTION('center_axis',(7.97031498468617E-17,-3.49202315903319E-16,
1.));
#17094=DIRECTION('ref_axis',(-0.900968867902416,-0.433883739117565,-7.97031498468616E-17));
#17095=DIRECTION('center_axis',(7.97031498468617E-17,-3.49202315903319E-16,
1.));
#17096=DIRECTION('ref_axis',(-0.900968867902416,-0.433883739117565,-7.97031498468616E-17));
#17097=DIRECTION('center_axis',(7.97031498468617E-17,-3.49202315903319E-16,
1.));
#17098=DIRECTION('ref_axis',(-0.900968867902416,-0.433883739117565,-7.97031498468616E-17));
#17099=DIRECTION('center_axis',(1.79091352057933E-16,-2.24573452299033E-16,
1.));
#17100=DIRECTION('ref_axis',(5.50003967499563E-33,-1.,-2.24573452299033E-16));
#17101=DIRECTION('center_axis',(1.79091352057933E-16,-2.24573452299033E-16,
1.));
#17102=DIRECTION('ref_axis',(5.50003967499563E-33,-1.,-2.24573452299033E-16));
#17103=DIRECTION('center_axis',(0.433883739117565,-0.900968867902416,-3.49202315903319E-16));
#17104=DIRECTION('ref_axis',(-4.48914099186257E-17,-4.09203893527877E-16,
1.));
#17105=DIRECTION('center_axis',(0.433883739117565,-0.900968867902416,-3.49202315903319E-16));
#17106=DIRECTION('ref_axis',(-4.48914099186258E-17,-4.09203893527877E-16,
1.));
#17107=DIRECTION('center_axis',(0.974927912181826,-0.222520933956305,-2.24573452299033E-16));
#17108=DIRECTION('ref_axis',(0.,-2.10741377257197E-16,1.));
#17109=DIRECTION('center_axis',(0.974927912181826,-0.222520933956305,-2.24573452299033E-16));
#17110=DIRECTION('ref_axis',(1.71433215598957E-16,-2.58125940401651E-16,
1.));
#17111=DIRECTION('center_axis',(0.222520933956305,0.974927912181826,3.85233095511904E-16));
#17112=DIRECTION('ref_axis',(0.,3.95140082357245E-16,-1.));
#17113=DIRECTION('center_axis',(0.974927912181826,-0.222520933956305,-2.24573452299033E-16));
#17114=DIRECTION('ref_axis',(1.71433215598957E-16,-2.58125940401651E-16,
1.));
#17115=DIRECTION('center_axis',(-0.222520933956305,-0.974927912181826,-1.14657265478815E-16));
#17116=DIRECTION('ref_axis',(0.,-1.24528628757585E-16,1.));
#17117=DIRECTION('center_axis',(1.43620113371564E-16,-6.91638013500039E-17,
1.));
#17118=DIRECTION('ref_axis',(1.,1.10509814492259E-33,-1.43620113371564E-16));
#17119=DIRECTION('center_axis',(-0.974927912181826,0.222520933956305,3.46377834692947E-17));
#17120=DIRECTION('ref_axis',(0.,1.55660785946981E-16,-1.));
#17121=DIRECTION('center_axis',(1.79091352057933E-16,-2.24573452299033E-16,
1.));
#17122=DIRECTION('ref_axis',(-0.222520933956305,-0.974927912181826,-1.79091352057932E-16));
#17123=DIRECTION('center_axis',(1.79091352057933E-16,-2.24573452299033E-16,
1.));
#17124=DIRECTION('ref_axis',(-0.222520933956305,-0.974927912181826,-1.79091352057932E-16));
#17125=DIRECTION('center_axis',(1.79091352057933E-16,-2.24573452299033E-16,
1.));
#17126=DIRECTION('ref_axis',(-0.222520933956305,-0.974927912181826,-1.79091352057932E-16));
#17127=DIRECTION('center_axis',(1.43620113371564E-16,-6.91638013500039E-17,
1.));
#17128=DIRECTION('ref_axis',(1.,1.10509814492259E-33,-1.43620113371564E-16));
#17129=DIRECTION('center_axis',(1.43620113371564E-16,-6.91638013500039E-17,
1.));
#17130=DIRECTION('ref_axis',(1.,1.10509814492259E-33,-1.43620113371564E-16));
#17131=DIRECTION('center_axis',(0.974927912181826,-0.222520933956305,-2.24573452299033E-16));
#17132=DIRECTION('ref_axis',(1.64444757441797E-16,-2.8874437615686E-16,
1.));
#17133=DIRECTION('center_axis',(0.974927912181826,-0.222520933956305,-2.24573452299033E-16));
#17134=DIRECTION('ref_axis',(1.64444757441797E-16,-2.8874437615686E-16,
1.));
#17135=DIRECTION('center_axis',(0.781831482468022,0.623489801858743,-6.91638013500039E-17));
#17136=DIRECTION('ref_axis',(0.,0.,1.));
#17137=DIRECTION('center_axis',(0.781831482468022,0.623489801858743,-6.91638013500039E-17));
#17138=DIRECTION('ref_axis',(5.40744373425973E-17,4.31229247995114E-17,
1.));
#17139=DIRECTION('center_axis',(-0.623489801858743,0.781831482468022,0.));
#17140=DIRECTION('ref_axis',(0.,0.,-1.));
#17141=DIRECTION('center_axis',(0.781831482468022,0.623489801858743,-6.91638013500039E-17));
#17142=DIRECTION('ref_axis',(5.40744373425973E-17,4.31229247995114E-17,
1.));
#17143=DIRECTION('center_axis',(0.623489801858743,-0.781831482468022,1.22464679914735E-16));
#17144=DIRECTION('ref_axis',(0.,0.,1.));
#17145=DIRECTION('center_axis',(0.,0.,-1.));
#17146=DIRECTION('ref_axis',(1.,0.,0.));
#17147=DIRECTION('center_axis',(0.,0.,-1.));
#17148=DIRECTION('ref_axis',(1.,0.,0.));
#17149=DIRECTION('center_axis',(0.,0.,-1.));
#17150=DIRECTION('ref_axis',(1.,0.,0.));
#17151=DIRECTION('center_axis',(-0.781831482468022,-0.623489801858743,0.));
#17152=DIRECTION('ref_axis',(0.,0.,-1.));
#17153=DIRECTION('center_axis',(1.43620113371564E-16,-6.91638013500039E-17,
1.));
#17154=DIRECTION('ref_axis',(0.623489801858743,-0.781831482468022,-1.43620113371564E-16));
#17155=DIRECTION('center_axis',(1.43620113371564E-16,-6.91638013500039E-17,
1.));
#17156=DIRECTION('ref_axis',(0.623489801858743,-0.781831482468022,-1.43620113371564E-16));
#17157=DIRECTION('center_axis',(1.43620113371564E-16,-6.91638013500039E-17,
1.));
#17158=DIRECTION('ref_axis',(0.623489801858743,-0.781831482468022,-1.43620113371564E-16));
#17159=DIRECTION('center_axis',(0.781831482468022,0.623489801858743,-6.91638013500039E-17));
#17160=DIRECTION('ref_axis',(5.40744373425973E-17,4.31229247995114E-17,
1.));
#17161=DIRECTION('center_axis',(0.781831482468022,0.623489801858743,-6.91638013500039E-17));
#17162=DIRECTION('ref_axis',(5.40744373425973E-17,4.31229247995114E-17,
1.));
#17163=DIRECTION('center_axis',(1.,0.,1.22464679914735E-16));
#17164=DIRECTION('ref_axis',(-6.12323399573677E-17,0.,1.));
#17165=DIRECTION('center_axis',(-1.43620113371566E-16,-6.91638013500059E-17,
1.));
#17166=DIRECTION('ref_axis',(1.,-1.10509814492274E-33,1.43620113371566E-16));
#17167=DIRECTION('center_axis',(0.,-1.,0.));
#17168=DIRECTION('ref_axis',(6.12323399573677E-17,0.,-1.));
#17169=DIRECTION('center_axis',(0.,0.,1.));
#17170=DIRECTION('ref_axis',(1.,0.,0.));
#17171=DIRECTION('center_axis',(0.,0.,1.));
#17172=DIRECTION('ref_axis',(1.,0.,0.));
#17173=DIRECTION('center_axis',(0.,0.,1.));
#17174=DIRECTION('ref_axis',(1.,0.,0.));
#17175=DIRECTION('center_axis',(-1.43620113371566E-16,-6.91638013500059E-17,
1.));
#17176=DIRECTION('ref_axis',(1.,-1.10509814492274E-33,1.43620113371566E-16));
#17177=DIRECTION('center_axis',(-1.43620113371566E-16,-6.91638013500059E-17,
1.));
#17178=DIRECTION('ref_axis',(1.,-1.10509814492274E-33,1.43620113371566E-16));
#17179=DIRECTION('center_axis',(0.,1.,0.));
#17180=DIRECTION('ref_axis',(0.,0.,1.));
#17181=DIRECTION('center_axis',(0.,1.,0.));
#17182=DIRECTION('ref_axis',(0.,0.,1.));
#17183=DIRECTION('center_axis',(0.,1.,0.));
#17184=DIRECTION('ref_axis',(0.,0.,1.));
#17185=DIRECTION('center_axis',(0.,1.,0.));
#17186=DIRECTION('ref_axis',(0.,0.,1.));
#17187=DIRECTION('center_axis',(-1.,0.,1.22464679914735E-16));
#17188=DIRECTION('ref_axis',(-1.22464679914735E-16,0.,-1.));
#17189=DIRECTION('center_axis',(0.,1.,0.));
#17190=DIRECTION('ref_axis',(0.,0.,1.));
#17191=DIRECTION('center_axis',(0.,0.,-1.));
#17192=DIRECTION('ref_axis',(-1.,0.,0.));
#17193=DIRECTION('center_axis',(0.,0.,-1.));
#17194=DIRECTION('ref_axis',(1.,0.,0.));
#17195=DIRECTION('center_axis',(0.,0.,-1.));
#17196=DIRECTION('ref_axis',(1.,0.,0.));
#17197=DIRECTION('center_axis',(0.,0.,-1.));
#17198=DIRECTION('ref_axis',(-1.,0.,0.));
#17199=DIRECTION('center_axis',(0.,0.,1.));
#17200=DIRECTION('ref_axis',(1.,0.,0.));
#17201=DIRECTION('center_axis',(0.,0.,1.));
#17202=DIRECTION('ref_axis',(1.,0.,0.));
#17203=DIRECTION('center_axis',(0.,0.,1.));
#17204=DIRECTION('ref_axis',(1.,0.,0.));
#17205=DIRECTION('center_axis',(0.,0.,1.));
#17206=DIRECTION('ref_axis',(1.,0.,0.));
#17207=DIRECTION('center_axis',(0.,1.,0.));
#17208=DIRECTION('ref_axis',(0.,0.,1.));
#17209=DIRECTION('center_axis',(0.,-1.,0.));
#17210=DIRECTION('ref_axis',(0.,0.,-1.));
#17211=DIRECTION('center_axis',(0.,0.,1.));
#17212=DIRECTION('ref_axis',(1.,0.,0.));
#17213=DIRECTION('center_axis',(0.,0.,-1.));
#17214=DIRECTION('ref_axis',(1.,0.,0.));
#17215=DIRECTION('center_axis',(0.,0.,1.));
#17216=DIRECTION('ref_axis',(1.,0.,0.));
#17217=DIRECTION('center_axis',(0.,0.,1.));
#17218=DIRECTION('ref_axis',(1.,0.,0.));
#17219=DIRECTION('center_axis',(0.,0.,-1.));
#17220=DIRECTION('ref_axis',(1.,0.,0.));
#17221=DIRECTION('center_axis',(0.,0.,1.));
#17222=DIRECTION('ref_axis',(1.,0.,0.));
#17223=DIRECTION('center_axis',(0.,0.,-1.));
#17224=DIRECTION('ref_axis',(-1.,0.,0.));
#17225=DIRECTION('center_axis',(0.,0.,-1.));
#17226=DIRECTION('ref_axis',(-1.,0.,0.));
#17227=DIRECTION('center_axis',(-0.781831482468022,-0.623489801858743,6.91638013500039E-17));
#17228=DIRECTION('ref_axis',(-1.43620113371564E-16,6.91638013500039E-17,
-1.));
#17229=DIRECTION('center_axis',(0.781831482468022,0.623489801858743,-6.91638013500039E-17));
#17230=DIRECTION('ref_axis',(1.43620113371564E-16,-6.91638013500039E-17,
1.));
#17231=DIRECTION('center_axis',(1.43620113371564E-16,-6.91638013500039E-17,
1.));
#17232=DIRECTION('ref_axis',(0.623489801858743,-0.781831482468022,-1.43620113371564E-16));
#17233=DIRECTION('center_axis',(-1.43620113371564E-16,6.91638013500039E-17,
-1.));
#17234=DIRECTION('ref_axis',(0.623489801858743,-0.781831482468022,-1.43620113371564E-16));
#17235=DIRECTION('center_axis',(1.43620113371564E-16,-6.91638013500039E-17,
1.));
#17236=DIRECTION('ref_axis',(0.623489801858743,-0.781831482468022,-1.43620113371564E-16));
#17237=DIRECTION('center_axis',(1.43620113371564E-16,-6.91638013500039E-17,
1.));
#17238=DIRECTION('ref_axis',(0.623489801858743,-0.781831482468022,-1.43620113371564E-16));
#17239=DIRECTION('center_axis',(-1.43620113371564E-16,6.91638013500039E-17,
-1.));
#17240=DIRECTION('ref_axis',(0.623489801858743,-0.781831482468022,-1.43620113371564E-16));
#17241=DIRECTION('center_axis',(1.43620113371564E-16,-6.91638013500039E-17,
1.));
#17242=DIRECTION('ref_axis',(0.623489801858743,-0.781831482468022,-1.43620113371564E-16));
#17243=DIRECTION('center_axis',(-1.43620113371564E-16,6.91638013500039E-17,
-1.));
#17244=DIRECTION('ref_axis',(-0.623489801858743,0.781831482468022,1.43620113371564E-16));
#17245=DIRECTION('center_axis',(-1.43620113371564E-16,6.91638013500039E-17,
-1.));
#17246=DIRECTION('ref_axis',(-0.623489801858743,0.781831482468022,1.43620113371564E-16));
#17247=DIRECTION('center_axis',(-1.79091352057933E-16,2.24573452299033E-16,
-1.));
#17248=DIRECTION('ref_axis',(0.222520933956305,0.974927912181826,1.79091352057932E-16));
#17249=DIRECTION('center_axis',(-1.79091352057933E-16,2.24573452299033E-16,
-1.));
#17250=DIRECTION('ref_axis',(-0.222520933956305,-0.974927912181826,-1.79091352057932E-16));
#17251=DIRECTION('center_axis',(-1.79091352057933E-16,2.24573452299033E-16,
-1.));
#17252=DIRECTION('ref_axis',(-0.222520933956305,-0.974927912181826,-1.79091352057932E-16));
#17253=DIRECTION('center_axis',(-1.79091352057933E-16,2.24573452299033E-16,
-1.));
#17254=DIRECTION('ref_axis',(0.222520933956305,0.974927912181826,1.79091352057932E-16));
#17255=DIRECTION('center_axis',(1.79091352057933E-16,-2.24573452299033E-16,
1.));
#17256=DIRECTION('ref_axis',(-0.222520933956305,-0.974927912181826,-1.79091352057932E-16));
#17257=DIRECTION('center_axis',(1.79091352057933E-16,-2.24573452299033E-16,
1.));
#17258=DIRECTION('ref_axis',(-0.222520933956305,-0.974927912181826,-1.79091352057932E-16));
#17259=DIRECTION('center_axis',(1.79091352057933E-16,-2.24573452299033E-16,
1.));
#17260=DIRECTION('ref_axis',(-0.222520933956305,-0.974927912181826,-1.79091352057932E-16));
#17261=DIRECTION('center_axis',(1.79091352057933E-16,-2.24573452299033E-16,
1.));
#17262=DIRECTION('ref_axis',(-0.222520933956305,-0.974927912181826,-1.79091352057932E-16));
#17263=DIRECTION('center_axis',(-0.974927912181826,0.222520933956305,2.24573452299033E-16));
#17264=DIRECTION('ref_axis',(-1.79091352057933E-16,2.24573452299033E-16,
-1.));
#17265=DIRECTION('center_axis',(0.974927912181826,-0.222520933956305,-2.24573452299033E-16));
#17266=DIRECTION('ref_axis',(1.79091352057933E-16,-2.24573452299033E-16,
1.));
#17267=DIRECTION('center_axis',(1.79091352057933E-16,-2.24573452299033E-16,
1.));
#17268=DIRECTION('ref_axis',(-0.222520933956305,-0.974927912181826,-1.79091352057932E-16));
#17269=DIRECTION('center_axis',(-1.79091352057933E-16,2.24573452299033E-16,
-1.));
#17270=DIRECTION('ref_axis',(-0.222520933956305,-0.974927912181826,-1.79091352057932E-16));
#17271=DIRECTION('center_axis',(1.79091352057933E-16,-2.24573452299033E-16,
1.));
#17272=DIRECTION('ref_axis',(-0.222520933956305,-0.974927912181826,-1.79091352057932E-16));
#17273=DIRECTION('center_axis',(1.79091352057933E-16,-2.24573452299033E-16,
1.));
#17274=DIRECTION('ref_axis',(-0.222520933956305,-0.974927912181826,-1.79091352057932E-16));
#17275=DIRECTION('center_axis',(-1.79091352057933E-16,2.24573452299033E-16,
-1.));
#17276=DIRECTION('ref_axis',(-0.222520933956305,-0.974927912181826,-1.79091352057932E-16));
#17277=DIRECTION('center_axis',(1.79091352057933E-16,-2.24573452299033E-16,
1.));
#17278=DIRECTION('ref_axis',(-0.222520933956305,-0.974927912181826,-1.79091352057932E-16));
#17279=DIRECTION('center_axis',(-1.79091352057933E-16,2.24573452299033E-16,
-1.));
#17280=DIRECTION('ref_axis',(0.222520933956305,0.974927912181826,1.79091352057932E-16));
#17281=DIRECTION('center_axis',(-1.79091352057933E-16,2.24573452299033E-16,
-1.));
#17282=DIRECTION('ref_axis',(0.222520933956305,0.974927912181826,1.79091352057932E-16));
#17283=DIRECTION('center_axis',(-7.97031498468617E-17,3.49202315903319E-16,
-1.));
#17284=DIRECTION('ref_axis',(0.900968867902416,0.433883739117565,7.97031498468616E-17));
#17285=DIRECTION('center_axis',(-7.97031498468617E-17,3.49202315903319E-16,
-1.));
#17286=DIRECTION('ref_axis',(-0.900968867902416,-0.433883739117565,-7.97031498468616E-17));
#17287=DIRECTION('center_axis',(-7.97031498468617E-17,3.49202315903319E-16,
-1.));
#17288=DIRECTION('ref_axis',(-0.900968867902416,-0.433883739117565,-7.97031498468616E-17));
#17289=DIRECTION('center_axis',(-7.97031498468617E-17,3.49202315903319E-16,
-1.));
#17290=DIRECTION('ref_axis',(0.900968867902416,0.433883739117565,7.97031498468616E-17));
#17291=DIRECTION('center_axis',(7.97031498468617E-17,-3.49202315903319E-16,
1.));
#17292=DIRECTION('ref_axis',(-0.900968867902416,-0.433883739117565,-7.97031498468616E-17));
#17293=DIRECTION('center_axis',(7.97031498468617E-17,-3.49202315903319E-16,
1.));
#17294=DIRECTION('ref_axis',(-0.900968867902416,-0.433883739117565,-7.97031498468616E-17));
#17295=DIRECTION('center_axis',(7.97031498468617E-17,-3.49202315903319E-16,
1.));
#17296=DIRECTION('ref_axis',(-0.900968867902416,-0.433883739117565,-7.97031498468616E-17));
#17297=DIRECTION('center_axis',(7.97031498468617E-17,-3.49202315903319E-16,
1.));
#17298=DIRECTION('ref_axis',(-0.900968867902416,-0.433883739117565,-7.97031498468616E-17));
#17299=DIRECTION('center_axis',(-0.433883739117565,0.900968867902416,3.49202315903319E-16));
#17300=DIRECTION('ref_axis',(-7.97031498468617E-17,3.49202315903319E-16,
-1.));
#17301=DIRECTION('center_axis',(0.433883739117565,-0.900968867902416,-3.49202315903319E-16));
#17302=DIRECTION('ref_axis',(7.97031498468617E-17,-3.49202315903319E-16,
1.));
#17303=DIRECTION('center_axis',(7.97031498468617E-17,-3.49202315903319E-16,
1.));
#17304=DIRECTION('ref_axis',(-0.900968867902416,-0.433883739117565,-7.97031498468616E-17));
#17305=DIRECTION('center_axis',(-7.97031498468617E-17,3.49202315903319E-16,
-1.));
#17306=DIRECTION('ref_axis',(-0.900968867902416,-0.433883739117565,-7.97031498468616E-17));
#17307=DIRECTION('center_axis',(7.97031498468617E-17,-3.49202315903319E-16,
1.));
#17308=DIRECTION('ref_axis',(-0.900968867902416,-0.433883739117565,-7.97031498468616E-17));
#17309=DIRECTION('center_axis',(7.97031498468617E-17,-3.49202315903319E-16,
1.));
#17310=DIRECTION('ref_axis',(-0.900968867902416,-0.433883739117565,-7.97031498468616E-17));
#17311=DIRECTION('center_axis',(-7.97031498468617E-17,3.49202315903319E-16,
-1.));
#17312=DIRECTION('ref_axis',(-0.900968867902416,-0.433883739117565,-7.97031498468616E-17));
#17313=DIRECTION('center_axis',(7.97031498468617E-17,-3.49202315903319E-16,
1.));
#17314=DIRECTION('ref_axis',(-0.900968867902416,-0.433883739117565,-7.97031498468616E-17));
#17315=DIRECTION('center_axis',(-7.97031498468617E-17,3.49202315903319E-16,
-1.));
#17316=DIRECTION('ref_axis',(0.900968867902416,0.433883739117565,7.97031498468616E-17));
#17317=DIRECTION('center_axis',(-7.97031498468617E-17,3.49202315903319E-16,
-1.));
#17318=DIRECTION('ref_axis',(0.900968867902416,0.433883739117565,7.97031498468616E-17));
#17319=DIRECTION('center_axis',(7.97031498468594E-17,3.4920231590332E-16,
-1.));
#17320=DIRECTION('ref_axis',(0.900968867902422,-0.433883739117553,-7.97031498468594E-17));
#17321=DIRECTION('center_axis',(7.97031498468594E-17,3.4920231590332E-16,
-1.));
#17322=DIRECTION('ref_axis',(-0.900968867902422,0.433883739117553,7.97031498468594E-17));
#17323=DIRECTION('center_axis',(7.97031498468594E-17,3.4920231590332E-16,
-1.));
#17324=DIRECTION('ref_axis',(-0.900968867902422,0.433883739117553,7.97031498468594E-17));
#17325=DIRECTION('center_axis',(7.97031498468594E-17,3.4920231590332E-16,
-1.));
#17326=DIRECTION('ref_axis',(0.900968867902422,-0.433883739117553,-7.97031498468594E-17));
#17327=DIRECTION('center_axis',(-7.97031498468594E-17,-3.4920231590332E-16,
1.));
#17328=DIRECTION('ref_axis',(-0.900968867902422,0.433883739117553,7.97031498468594E-17));
#17329=DIRECTION('center_axis',(-7.97031498468594E-17,-3.4920231590332E-16,
1.));
#17330=DIRECTION('ref_axis',(-0.900968867902422,0.433883739117553,7.97031498468594E-17));
#17331=DIRECTION('center_axis',(-7.97031498468594E-17,-3.4920231590332E-16,
1.));
#17332=DIRECTION('ref_axis',(-0.900968867902422,0.433883739117553,7.97031498468594E-17));
#17333=DIRECTION('center_axis',(-7.97031498468594E-17,-3.4920231590332E-16,
1.));
#17334=DIRECTION('ref_axis',(-0.900968867902422,0.433883739117553,7.97031498468594E-17));
#17335=DIRECTION('center_axis',(0.433883739117553,0.900968867902422,3.4920231590332E-16));
#17336=DIRECTION('ref_axis',(7.97031498468594E-17,3.4920231590332E-16,-1.));
#17337=DIRECTION('center_axis',(-0.433883739117553,-0.900968867902422,-3.4920231590332E-16));
#17338=DIRECTION('ref_axis',(-7.97031498468594E-17,-3.4920231590332E-16,
1.));
#17339=DIRECTION('center_axis',(-7.97031498468594E-17,-3.4920231590332E-16,
1.));
#17340=DIRECTION('ref_axis',(-0.900968867902422,0.433883739117553,7.97031498468594E-17));
#17341=DIRECTION('center_axis',(7.97031498468594E-17,3.4920231590332E-16,
-1.));
#17342=DIRECTION('ref_axis',(-0.900968867902422,0.433883739117553,7.97031498468594E-17));
#17343=DIRECTION('center_axis',(-7.97031498468594E-17,-3.4920231590332E-16,
1.));
#17344=DIRECTION('ref_axis',(-0.900968867902422,0.433883739117553,7.97031498468594E-17));
#17345=DIRECTION('center_axis',(-7.97031498468594E-17,-3.4920231590332E-16,
1.));
#17346=DIRECTION('ref_axis',(-0.900968867902422,0.433883739117553,7.97031498468594E-17));
#17347=DIRECTION('center_axis',(7.97031498468594E-17,3.4920231590332E-16,
-1.));
#17348=DIRECTION('ref_axis',(-0.900968867902422,0.433883739117553,7.97031498468594E-17));
#17349=DIRECTION('center_axis',(-7.97031498468594E-17,-3.4920231590332E-16,
1.));
#17350=DIRECTION('ref_axis',(-0.900968867902422,0.433883739117553,7.97031498468594E-17));
#17351=DIRECTION('center_axis',(7.97031498468594E-17,3.4920231590332E-16,
-1.));
#17352=DIRECTION('ref_axis',(0.900968867902422,-0.433883739117553,-7.97031498468594E-17));
#17353=DIRECTION('center_axis',(7.97031498468594E-17,3.4920231590332E-16,
-1.));
#17354=DIRECTION('ref_axis',(0.900968867902422,-0.433883739117553,-7.97031498468594E-17));
#17355=DIRECTION('center_axis',(1.79091352057932E-16,2.24573452299036E-16,
-1.));
#17356=DIRECTION('ref_axis',(0.222520933956318,-0.974927912181823,-1.79091352057933E-16));
#17357=DIRECTION('center_axis',(1.79091352057932E-16,2.24573452299036E-16,
-1.));
#17358=DIRECTION('ref_axis',(-0.222520933956318,0.974927912181823,1.79091352057933E-16));
#17359=DIRECTION('center_axis',(1.79091352057932E-16,2.24573452299036E-16,
-1.));
#17360=DIRECTION('ref_axis',(-0.222520933956318,0.974927912181823,1.79091352057933E-16));
#17361=DIRECTION('center_axis',(1.79091352057932E-16,2.24573452299036E-16,
-1.));
#17362=DIRECTION('ref_axis',(0.222520933956318,-0.974927912181823,-1.79091352057933E-16));
#17363=DIRECTION('center_axis',(-1.79091352057932E-16,-2.24573452299036E-16,
1.));
#17364=DIRECTION('ref_axis',(-0.222520933956318,0.974927912181823,1.79091352057933E-16));
#17365=DIRECTION('center_axis',(-1.79091352057932E-16,-2.24573452299036E-16,
1.));
#17366=DIRECTION('ref_axis',(-0.222520933956318,0.974927912181823,1.79091352057933E-16));
#17367=DIRECTION('center_axis',(-1.79091352057932E-16,-2.24573452299036E-16,
1.));
#17368=DIRECTION('ref_axis',(-0.222520933956318,0.974927912181823,1.79091352057933E-16));
#17369=DIRECTION('center_axis',(-1.79091352057932E-16,-2.24573452299036E-16,
1.));
#17370=DIRECTION('ref_axis',(-0.222520933956318,0.974927912181823,1.79091352057933E-16));
#17371=DIRECTION('center_axis',(0.974927912181823,0.222520933956318,2.24573452299036E-16));
#17372=DIRECTION('ref_axis',(1.79091352057932E-16,2.24573452299036E-16,
-1.));
#17373=DIRECTION('center_axis',(-0.974927912181823,-0.222520933956318,-2.24573452299036E-16));
#17374=DIRECTION('ref_axis',(-1.79091352057932E-16,-2.24573452299036E-16,
1.));
#17375=DIRECTION('center_axis',(-1.79091352057932E-16,-2.24573452299036E-16,
1.));
#17376=DIRECTION('ref_axis',(-0.222520933956318,0.974927912181823,1.79091352057933E-16));
#17377=DIRECTION('center_axis',(1.79091352057932E-16,2.24573452299036E-16,
-1.));
#17378=DIRECTION('ref_axis',(-0.222520933956318,0.974927912181823,1.79091352057933E-16));
#17379=DIRECTION('center_axis',(-1.79091352057932E-16,-2.24573452299036E-16,
1.));
#17380=DIRECTION('ref_axis',(-0.222520933956318,0.974927912181823,1.79091352057933E-16));
#17381=DIRECTION('center_axis',(-1.79091352057932E-16,-2.24573452299036E-16,
1.));
#17382=DIRECTION('ref_axis',(-0.222520933956318,0.974927912181823,1.79091352057933E-16));
#17383=DIRECTION('center_axis',(1.79091352057932E-16,2.24573452299036E-16,
-1.));
#17384=DIRECTION('ref_axis',(-0.222520933956318,0.974927912181823,1.79091352057933E-16));
#17385=DIRECTION('center_axis',(-1.79091352057932E-16,-2.24573452299036E-16,
1.));
#17386=DIRECTION('ref_axis',(-0.222520933956318,0.974927912181823,1.79091352057933E-16));
#17387=DIRECTION('center_axis',(1.79091352057932E-16,2.24573452299036E-16,
-1.));
#17388=DIRECTION('ref_axis',(0.222520933956318,-0.974927912181823,-1.79091352057933E-16));
#17389=DIRECTION('center_axis',(1.79091352057932E-16,2.24573452299036E-16,
-1.));
#17390=DIRECTION('ref_axis',(0.222520933956318,-0.974927912181823,-1.79091352057933E-16));
#17391=DIRECTION('center_axis',(1.43620113371566E-16,6.91638013500059E-17,
-1.));
#17392=DIRECTION('ref_axis',(-0.623489801858732,-0.781831482468031,-1.43620113371566E-16));
#17393=DIRECTION('center_axis',(1.43620113371566E-16,6.91638013500059E-17,
-1.));
#17394=DIRECTION('ref_axis',(0.623489801858732,0.781831482468031,1.43620113371566E-16));
#17395=DIRECTION('center_axis',(1.43620113371566E-16,6.91638013500059E-17,
-1.));
#17396=DIRECTION('ref_axis',(0.623489801858732,0.781831482468031,1.43620113371566E-16));
#17397=DIRECTION('center_axis',(1.43620113371566E-16,6.91638013500059E-17,
-1.));
#17398=DIRECTION('ref_axis',(-0.623489801858732,-0.781831482468031,-1.43620113371566E-16));
#17399=DIRECTION('center_axis',(-1.43620113371566E-16,-6.91638013500059E-17,
1.));
#17400=DIRECTION('ref_axis',(0.623489801858732,0.781831482468031,1.43620113371566E-16));
#17401=DIRECTION('center_axis',(-1.43620113371566E-16,-6.91638013500059E-17,
1.));
#17402=DIRECTION('ref_axis',(0.623489801858732,0.781831482468031,1.43620113371566E-16));
#17403=DIRECTION('center_axis',(-1.43620113371566E-16,-6.91638013500059E-17,
1.));
#17404=DIRECTION('ref_axis',(0.623489801858732,0.781831482468031,1.43620113371566E-16));
#17405=DIRECTION('center_axis',(-1.43620113371566E-16,-6.91638013500059E-17,
1.));
#17406=DIRECTION('ref_axis',(0.623489801858732,0.781831482468031,1.43620113371566E-16));
#17407=DIRECTION('center_axis',(0.781831482468031,-0.623489801858732,6.91638013500059E-17));
#17408=DIRECTION('ref_axis',(1.43620113371566E-16,6.91638013500061E-17,
-1.));
#17409=DIRECTION('center_axis',(-0.781831482468031,0.623489801858732,-6.91638013500059E-17));
#17410=DIRECTION('ref_axis',(-1.43620113371566E-16,-6.91638013500061E-17,
1.));
#17411=DIRECTION('center_axis',(-1.43620113371566E-16,-6.91638013500059E-17,
1.));
#17412=DIRECTION('ref_axis',(0.623489801858732,0.781831482468031,1.43620113371566E-16));
#17413=DIRECTION('center_axis',(1.43620113371566E-16,6.91638013500059E-17,
-1.));
#17414=DIRECTION('ref_axis',(0.623489801858732,0.781831482468031,1.43620113371566E-16));
#17415=DIRECTION('center_axis',(-1.43620113371566E-16,-6.91638013500059E-17,
1.));
#17416=DIRECTION('ref_axis',(0.623489801858732,0.781831482468031,1.43620113371566E-16));
#17417=DIRECTION('center_axis',(-1.43620113371566E-16,-6.91638013500059E-17,
1.));
#17418=DIRECTION('ref_axis',(0.623489801858732,0.781831482468031,1.43620113371566E-16));
#17419=DIRECTION('center_axis',(1.43620113371566E-16,6.91638013500059E-17,
-1.));
#17420=DIRECTION('ref_axis',(0.623489801858732,0.781831482468031,1.43620113371566E-16));
#17421=DIRECTION('center_axis',(-1.43620113371566E-16,-6.91638013500059E-17,
1.));
#17422=DIRECTION('ref_axis',(0.623489801858732,0.781831482468031,1.43620113371566E-16));
#17423=DIRECTION('center_axis',(1.43620113371566E-16,6.91638013500059E-17,
-1.));
#17424=DIRECTION('ref_axis',(-0.623489801858732,-0.781831482468031,-1.43620113371566E-16));
#17425=DIRECTION('center_axis',(1.43620113371566E-16,6.91638013500059E-17,
-1.));
#17426=DIRECTION('ref_axis',(-0.623489801858732,-0.781831482468031,-1.43620113371566E-16));
#17427=DIRECTION('center_axis',(0.,0.,1.));
#17428=DIRECTION('ref_axis',(1.,0.,0.));
#17429=DIRECTION('center_axis',(0.,0.,-1.));
#17430=DIRECTION('ref_axis',(1.,0.,0.));
#17431=DIRECTION('center_axis',(0.,0.,1.));
#17432=DIRECTION('ref_axis',(1.,0.,0.));
#17433=DIRECTION('center_axis',(0.,0.,1.));
#17434=DIRECTION('ref_axis',(1.,0.,0.));
#17435=DIRECTION('center_axis',(0.,0.,-1.));
#17436=DIRECTION('ref_axis',(1.,0.,0.));
#17437=DIRECTION('center_axis',(0.,0.,1.));
#17438=DIRECTION('ref_axis',(1.,0.,0.));
#17439=DIRECTION('center_axis',(0.,0.,-1.));
#17440=DIRECTION('ref_axis',(-1.,0.,0.));
#17441=DIRECTION('center_axis',(0.,0.,-1.));
#17442=DIRECTION('ref_axis',(-1.,0.,0.));
#17443=DIRECTION('axis',(0.,0.,1.));
#17444=DIRECTION('refdir',(1.,0.,0.));
#17445=DIRECTION('center_axis',(0.,-1.83697019872103E-16,-1.));
#17446=DIRECTION('ref_axis',(0.,-1.,1.83697019872103E-16));
#17447=DIRECTION('center_axis',(0.,1.83697019872103E-16,1.));
#17448=DIRECTION('ref_axis',(0.,-1.,1.83697019872103E-16));
#17449=DIRECTION('center_axis',(-1.,1.22464679914735E-16,-2.24963967399279E-32));
#17450=DIRECTION('ref_axis',(1.22464679914735E-16,1.,-1.83697019872103E-16));
#17451=DIRECTION('center_axis',(0.,1.83697019872103E-16,1.));
#17452=DIRECTION('ref_axis',(0.,-1.,1.83697019872103E-16));
#17453=DIRECTION('center_axis',(0.,1.83697019872103E-16,1.));
#17454=DIRECTION('ref_axis',(0.,1.,-2.09599627067876E-16));
#17455=DIRECTION('center_axis',(0.,-1.83697019872103E-16,-1.));
#17456=DIRECTION('ref_axis',(0.,1.,-1.83697019872103E-16));
#17457=DIRECTION('center_axis',(1.,1.22464679914735E-16,-2.24963967399279E-32));
#17458=DIRECTION('ref_axis',(1.22464679914735E-16,-1.,1.30999766917423E-16));
#17459=DIRECTION('center_axis',(0.,1.83697019872103E-16,1.));
#17460=DIRECTION('ref_axis',(0.,1.,-1.83697019872103E-16));
#17461=DIRECTION('center_axis',(0.,1.83697019872103E-16,1.));
#17462=DIRECTION('ref_axis',(0.,1.,-1.83697019872103E-16));
#17463=DIRECTION('center_axis',(0.,-1.83697019872103E-16,-1.));
#17464=DIRECTION('ref_axis',(0.,1.,-1.83697019872103E-16));
#17465=DIRECTION('center_axis',(0.,1.83697019872103E-16,1.));
#17466=DIRECTION('ref_axis',(0.,1.,-2.09599627067876E-16));
#17467=DIRECTION('center_axis',(0.,-1.83697019872103E-16,-1.));
#17468=DIRECTION('ref_axis',(0.,1.,-1.83697019872103E-16));
#17469=DIRECTION('center_axis',(1.,1.22464679914735E-16,-2.24963967399279E-32));
#17470=DIRECTION('ref_axis',(1.22464679914735E-16,-1.,1.30999766917423E-16));
#17471=DIRECTION('center_axis',(0.,1.83697019872103E-16,1.));
#17472=DIRECTION('ref_axis',(0.,-1.,1.83697019872103E-16));
#17473=DIRECTION('center_axis',(0.,-1.83697019872103E-16,-1.));
#17474=DIRECTION('ref_axis',(0.,1.,-1.83697019872103E-16));
#17475=DIRECTION('center_axis',(0.,-1.83697019872103E-16,-1.));
#17476=DIRECTION('ref_axis',(0.,-1.,1.83697019872103E-16));
#17477=DIRECTION('',(8.65956056235483E-17,0.707106781186539,-0.707106781186556));
#17478=DIRECTION('center_axis',(0.,1.83697019872103E-16,1.));
#17479=DIRECTION('ref_axis',(0.,-1.,1.83697019872103E-16));
#17480=DIRECTION('center_axis',(0.,1.83697019872103E-16,1.));
#17481=DIRECTION('ref_axis',(0.,-1.,1.83697019872103E-16));
#17482=DIRECTION('',(0.,1.83697019872103E-16,1.));
#17483=DIRECTION('center_axis',(0.,1.83697019872103E-16,1.));
#17484=DIRECTION('ref_axis',(0.,1.,-1.83697019872103E-16));
#17485=DIRECTION('',(8.65956056235483E-17,-0.707106781186539,0.707106781186556));
#17486=DIRECTION('center_axis',(0.,1.83697019872103E-16,1.));
#17487=DIRECTION('ref_axis',(0.,-1.,1.83697019872103E-16));
#17488=DIRECTION('center_axis',(0.,1.83697019872103E-16,1.));
#17489=DIRECTION('ref_axis',(0.,-1.,1.83697019872103E-16));
#17490=DIRECTION('center_axis',(0.,1.83697019872103E-16,1.));
#17491=DIRECTION('ref_axis',(0.,-1.,1.83697019872103E-16));
#17492=DIRECTION('',(0.,-1.83697019872103E-16,-1.));
#17493=DIRECTION('center_axis',(0.,1.83697019872103E-16,1.));
#17494=DIRECTION('ref_axis',(0.,-1.,1.83697019872103E-16));
#17495=DIRECTION('',(0.,-1.83697019872103E-16,-1.));
#17496=DIRECTION('center_axis',(0.,1.83697019872103E-16,1.));
#17497=DIRECTION('ref_axis',(0.,-1.,1.83697019872103E-16));
#17498=DIRECTION('center_axis',(0.,-1.83697019872103E-16,-1.));
#17499=DIRECTION('ref_axis',(0.,1.,-1.83697019872103E-16));
#17500=DIRECTION('center_axis',(0.,1.83697019872103E-16,1.));
#17501=DIRECTION('ref_axis',(0.,-1.,1.83697019872103E-16));
#17502=DIRECTION('center_axis',(-1.,0.,0.));
#17503=DIRECTION('ref_axis',(0.,1.,0.));
#17504=DIRECTION('center_axis',(0.,1.22464679914735E-16,1.));
#17505=DIRECTION('ref_axis',(0.,-1.,1.22464679914735E-16));
#17506=DIRECTION('center_axis',(-0.623489801858732,0.781831482468031,-1.43620113371566E-16));
#17507=DIRECTION('ref_axis',(0.781831482468031,0.623489801858732,6.91638013500061E-17));
#17508=DIRECTION('center_axis',(-4.78733711238555E-17,1.45519280364738E-16,
1.));
#17509=DIRECTION('ref_axis',(-0.781831482468031,-0.623489801858732,5.33008785647293E-17));
#17510=DIRECTION('center_axis',(0.222520933956319,0.974927912181823,-1.79091352057932E-16));
#17511=DIRECTION('ref_axis',(0.974927912181823,-0.222520933956319,2.24573452299036E-16));
#17512=DIRECTION('center_axis',(-5.96971173526444E-17,1.97322497347747E-16,
1.));
#17513=DIRECTION('ref_axis',(-0.974927912181823,0.222520933956319,-1.02108772384301E-16));
#17514=DIRECTION('center_axis',(0.900968867902422,0.433883739117552,-7.97031498468594E-17));
#17515=DIRECTION('ref_axis',(0.433883739117552,-0.900968867902422,3.4920231590332E-16));
#17516=DIRECTION('center_axis',(-2.65677166156194E-17,2.38865451882509E-16,
1.));
#17517=DIRECTION('ref_axis',(-0.433883739117552,0.900968867902422,-2.26737635988585E-16));
#17518=DIRECTION('center_axis',(0.900968867902416,-0.433883739117565,7.97031498468616E-17));
#17519=DIRECTION('ref_axis',(-0.433883739117565,-0.900968867902416,3.49202315903319E-16));
#17520=DIRECTION('center_axis',(2.65677166156204E-17,2.38865451882508E-16,
1.));
#17521=DIRECTION('ref_axis',(0.433883739117565,0.900968867902416,-2.26737635988584E-16));
#17522=DIRECTION('center_axis',(0.222520933956305,-0.974927912181826,1.79091352057933E-16));
#17523=DIRECTION('ref_axis',(-0.974927912181826,-0.222520933956305,2.24573452299033E-16));
#17524=DIRECTION('center_axis',(5.9697117352644E-17,1.97322497347747E-16,
1.));
#17525=DIRECTION('ref_axis',(0.974927912181826,0.222520933956305,-1.02108772384298E-16));
#17526=DIRECTION('center_axis',(-0.623489801858743,-0.781831482468022,1.43620113371564E-16));
#17527=DIRECTION('ref_axis',(-0.781831482468022,0.623489801858743,6.91638013500039E-17));
#17528=DIRECTION('center_axis',(4.78733711238546E-17,1.45519280364737E-16,
1.));
#17529=DIRECTION('ref_axis',(0.781831482468022,-0.623489801858743,5.33008785647315E-17));
#17530=DIRECTION('center_axis',(0.,1.83697019872103E-16,1.));
#17531=DIRECTION('ref_axis',(0.,1.,-1.62614292875575E-16));
#17532=DIRECTION('center_axis',(0.,-1.83697019872103E-16,-1.));
#17533=DIRECTION('ref_axis',(0.,1.,-1.83697019872103E-16));
#17534=DIRECTION('center_axis',(1.,1.22464679914735E-16,-2.24963967399279E-32));
#17535=DIRECTION('ref_axis',(1.22464679914735E-16,-1.,2.03267866094469E-16));
#17536=DIRECTION('center_axis',(0.,1.83697019872103E-16,1.));
#17537=DIRECTION('ref_axis',(0.,1.,-1.83697019872103E-16));
#17538=DIRECTION('center_axis',(0.,1.83697019872103E-16,1.));
#17539=DIRECTION('ref_axis',(0.,1.,-1.83697019872103E-16));
#17540=DIRECTION('center_axis',(0.,-1.83697019872103E-16,-1.));
#17541=DIRECTION('ref_axis',(0.,-1.,1.64970202400831E-16));
#17542=DIRECTION('center_axis',(0.,1.83697019872103E-16,1.));
#17543=DIRECTION('ref_axis',(0.,-1.,1.83697019872103E-16));
#17544=DIRECTION('center_axis',(1.,-1.22464679914735E-16,2.24963967399279E-32));
#17545=DIRECTION('ref_axis',(1.22464679914735E-16,1.,-2.06212753001039E-16));
#17546=DIRECTION('center_axis',(0.,-1.83697019872103E-16,-1.));
#17547=DIRECTION('ref_axis',(0.,-1.,1.83697019872103E-16));
#17548=DIRECTION('center_axis',(0.,-1.83697019872103E-16,-1.));
#17549=DIRECTION('ref_axis',(0.,-1.,1.62614292875575E-16));
#17550=DIRECTION('center_axis',(0.,1.83697019872103E-16,1.));
#17551=DIRECTION('ref_axis',(0.,-1.,1.83697019872103E-16));
#17552=DIRECTION('center_axis',(1.,-1.22464679914735E-16,2.24963967399279E-32));
#17553=DIRECTION('ref_axis',(1.22464679914735E-16,1.,-2.03267866094469E-16));
#17554=DIRECTION('center_axis',(0.,-1.83697019872103E-16,-1.));
#17555=DIRECTION('ref_axis',(0.,-1.,1.83697019872103E-16));
#17556=DIRECTION('center_axis',(0.,1.83697019872103E-16,1.));
#17557=DIRECTION('ref_axis',(0.,1.,-1.64970202400831E-16));
#17558=DIRECTION('center_axis',(0.,-1.83697019872103E-16,-1.));
#17559=DIRECTION('ref_axis',(0.,1.,-1.83697019872103E-16));
#17560=DIRECTION('center_axis',(1.,1.22464679914735E-16,-2.24963967399279E-32));
#17561=DIRECTION('ref_axis',(1.22464679914735E-16,-1.,2.06212753001039E-16));
#17562=DIRECTION('center_axis',(0.,1.83697019872103E-16,1.));
#17563=DIRECTION('ref_axis',(0.,1.,-1.83697019872103E-16));
#17564=DIRECTION('center_axis',(0.,-1.83697019872103E-16,-1.));
#17565=DIRECTION('ref_axis',(0.,1.,-1.83697019872103E-16));
#17566=DIRECTION('center_axis',(0.,1.83697019872103E-16,1.));
#17567=DIRECTION('ref_axis',(0.,-1.,1.83697019872103E-16));
#17568=DIRECTION('center_axis',(0.,1.83697019872103E-16,1.));
#17569=DIRECTION('ref_axis',(0.,-1.,1.83697019872103E-16));
#17570=DIRECTION('',(0.,1.83697019872103E-16,1.));
#17571=DIRECTION('center_axis',(0.,1.83697019872103E-16,1.));
#17572=DIRECTION('ref_axis',(0.,-1.,1.83697019872103E-16));
#17573=DIRECTION('center_axis',(0.,1.83697019872103E-16,1.));
#17574=DIRECTION('ref_axis',(0.,-1.,1.83697019872103E-16));
#17575=DIRECTION('',(0.,1.83697019872103E-16,1.));
#17576=DIRECTION('center_axis',(0.,1.83697019872103E-16,1.));
#17577=DIRECTION('ref_axis',(0.,-1.,1.83697019872103E-16));
#17578=DIRECTION('center_axis',(0.,1.83697019872103E-16,1.));
#17579=DIRECTION('ref_axis',(0.,-1.,1.83697019872103E-16));
#17580=DIRECTION('center_axis',(0.,1.83697019872103E-16,1.));
#17581=DIRECTION('ref_axis',(0.,-1.,1.83697019872103E-16));
#17582=DIRECTION('',(0.,1.83697019872103E-16,1.));
#17583=DIRECTION('center_axis',(0.,-1.83697019872103E-16,-1.));
#17584=DIRECTION('ref_axis',(0.,-1.,1.83697019872103E-16));
#17585=DIRECTION('center_axis',(-1.,1.22464679914735E-16,-2.24963967399279E-32));
#17586=DIRECTION('ref_axis',(1.22464679914735E-16,1.,-1.83697019872103E-16));
#17587=DIRECTION('center_axis',(0.,1.83697019872103E-16,1.));
#17588=DIRECTION('ref_axis',(0.,-1.,1.83697019872103E-16));
#17589=DIRECTION('center_axis',(0.,1.83697019872103E-16,1.));
#17590=DIRECTION('ref_axis',(0.,-1.,1.83697019872103E-16));
#17591=DIRECTION('',(0.,1.83697019872103E-16,1.));
#17592=DIRECTION('center_axis',(0.,1.83697019872103E-16,1.));
#17593=DIRECTION('ref_axis',(0.,-1.,1.83697019872103E-16));
#17594=DIRECTION('center_axis',(0.,1.83697019872103E-16,1.));
#17595=DIRECTION('ref_axis',(0.,-1.,1.83697019872103E-16));
#17596=DIRECTION('',(0.,1.83697019872103E-16,1.));
#17597=DIRECTION('center_axis',(0.,1.83697019872103E-16,1.));
#17598=DIRECTION('ref_axis',(0.,-1.,1.83697019872103E-16));
#17599=DIRECTION('center_axis',(0.,1.83697019872103E-16,1.));
#17600=DIRECTION('ref_axis',(0.,-1.,1.83697019872103E-16));
#17601=DIRECTION('',(0.,1.83697019872103E-16,1.));
#17602=DIRECTION('center_axis',(0.,1.83697019872103E-16,1.));
#17603=DIRECTION('ref_axis',(0.,-1.,1.83697019872103E-16));
#17604=DIRECTION('center_axis',(0.,-1.83697019872103E-16,-1.));
#17605=DIRECTION('ref_axis',(0.,-1.,1.83697019872103E-16));
#17606=DIRECTION('center_axis',(0.,1.83697019872103E-16,1.));
#17607=DIRECTION('ref_axis',(0.,-1.,1.83697019872103E-16));
#17608=DIRECTION('',(-8.65956056235488E-17,-0.707106781186543,0.707106781186552));
#17609=DIRECTION('center_axis',(0.,1.83697019872103E-16,1.));
#17610=DIRECTION('ref_axis',(0.,-1.,1.83697019872103E-16));
#17611=DIRECTION('center_axis',(0.,1.83697019872103E-16,1.));
#17612=DIRECTION('ref_axis',(0.,1.,-1.83697019872103E-16));
#17613=DIRECTION('center_axis',(0.,1.83697019872103E-16,1.));
#17614=DIRECTION('ref_axis',(0.,-1.,1.83697019872103E-16));
#17615=DIRECTION('center_axis',(0.,1.83697019872103E-16,1.));
#17616=DIRECTION('ref_axis',(0.,-1.,1.83697019872103E-16));
#17617=DIRECTION('',(-8.65956056235488E-17,0.707106781186543,-0.707106781186552));
#17618=DIRECTION('center_axis',(0.,1.83697019872103E-16,1.));
#17619=DIRECTION('ref_axis',(0.,-1.,1.83697019872103E-16));
#17620=DIRECTION('center_axis',(0.,1.83697019872103E-16,1.));
#17621=DIRECTION('ref_axis',(0.,-1.,1.83697019872103E-16));
#17622=DIRECTION('',(0.,-1.83697019872103E-16,-1.));
#17623=DIRECTION('center_axis',(0.,-1.83697019872103E-16,-1.));
#17624=DIRECTION('ref_axis',(0.,1.,-1.83697019872103E-16));
#17625=DIRECTION('center_axis',(0.,1.83697019872103E-16,1.));
#17626=DIRECTION('ref_axis',(0.,-1.,1.83697019872103E-16));
#17627=DIRECTION('center_axis',(0.,-1.83697019872103E-16,-1.));
#17628=DIRECTION('ref_axis',(0.,1.,-1.83697019872103E-16));
#17629=DIRECTION('center_axis',(0.,1.83697019872103E-16,1.));
#17630=DIRECTION('ref_axis',(0.,-1.,1.83697019872103E-16));
#17631=DIRECTION('center_axis',(0.,-1.83697019872103E-16,-1.));
#17632=DIRECTION('ref_axis',(0.,1.,-1.83697019872103E-16));
#17633=DIRECTION('center_axis',(0.,1.83697019872103E-16,1.));
#17634=DIRECTION('ref_axis',(0.,-1.,1.83697019872103E-16));
#17635=DIRECTION('center_axis',(-0.781831482468031,0.623489801858732,6.91638013500059E-17));
#17636=DIRECTION('ref_axis',(0.,0.,-1.));
#17637=DIRECTION('center_axis',(0.781831482468031,-0.623489801858732,-6.91638013500059E-17));
#17638=DIRECTION('ref_axis',(-5.40744373425995E-17,4.31229247995119E-17,
-1.));
#17639=DIRECTION('center_axis',(0.623489801858732,0.781831482468031,0.));
#17640=DIRECTION('ref_axis',(0.,0.,1.));
#17641=DIRECTION('center_axis',(0.781831482468031,-0.623489801858732,-6.91638013500059E-17));
#17642=DIRECTION('ref_axis',(-5.40744373425995E-17,4.31229247995119E-17,
-1.));
#17643=DIRECTION('center_axis',(0.623489801858732,0.781831482468031,-1.22464679914735E-16));
#17644=DIRECTION('ref_axis',(0.,0.,-1.));
#17645=DIRECTION('center_axis',(1.79091352057932E-16,2.24573452299036E-16,
1.));
#17646=DIRECTION('ref_axis',(-5.50003967499518E-33,-1.,2.24573452299036E-16));
#17647=DIRECTION('center_axis',(1.79091352057932E-16,2.24573452299036E-16,
1.));
#17648=DIRECTION('ref_axis',(-5.5000396749952E-33,-1.,2.24573452299036E-16));
#17649=DIRECTION('center_axis',(1.79091352057932E-16,2.24573452299036E-16,
1.));
#17650=DIRECTION('ref_axis',(-5.50003967499518E-33,-1.,2.24573452299036E-16));
#17651=DIRECTION('center_axis',(-0.781831482468031,0.623489801858732,0.));
#17652=DIRECTION('ref_axis',(0.,0.,1.));
#17653=DIRECTION('center_axis',(1.43620113371566E-16,6.91638013500059E-17,
1.));
#17654=DIRECTION('ref_axis',(0.623489801858732,0.781831482468031,-1.43620113371566E-16));
#17655=DIRECTION('center_axis',(1.43620113371566E-16,6.91638013500059E-17,
1.));
#17656=DIRECTION('ref_axis',(0.623489801858732,0.781831482468031,-1.43620113371566E-16));
#17657=DIRECTION('center_axis',(1.43620113371566E-16,6.91638013500059E-17,
1.));
#17658=DIRECTION('ref_axis',(0.623489801858732,0.781831482468031,-1.43620113371566E-16));
#17659=DIRECTION('center_axis',(0.781831482468031,-0.623489801858732,-6.91638013500059E-17));
#17660=DIRECTION('ref_axis',(-5.40744373425995E-17,4.31229247995119E-17,
-1.));
#17661=DIRECTION('center_axis',(0.781831482468031,-0.623489801858732,-6.91638013500059E-17));
#17662=DIRECTION('ref_axis',(-5.40744373425995E-17,4.31229247995119E-17,
-1.));
#17663=DIRECTION('center_axis',(-0.974927912181823,-0.222520933956318,2.24573452299036E-16));
#17664=DIRECTION('ref_axis',(0.,-2.10741377257197E-16,-1.));
#17665=DIRECTION('center_axis',(0.974927912181823,0.222520933956318,-2.24573452299036E-16));
#17666=DIRECTION('ref_axis',(-1.71433215598957E-16,-2.58125940401653E-16,
-1.));
#17667=DIRECTION('center_axis',(-0.222520933956318,0.974927912181823,-3.85233095511903E-16));
#17668=DIRECTION('ref_axis',(0.,3.95140082357245E-16,1.));
#17669=DIRECTION('center_axis',(0.974927912181823,0.222520933956318,-2.24573452299036E-16));
#17670=DIRECTION('ref_axis',(-1.71433215598957E-16,-2.58125940401653E-16,
-1.));
#17671=DIRECTION('center_axis',(-0.222520933956318,0.974927912181823,-3.59586625308286E-16));
#17672=DIRECTION('ref_axis',(0.,-2.4905725751517E-16,-1.));
#17673=DIRECTION('center_axis',(7.97031498468594E-17,3.4920231590332E-16,
1.));
#17674=DIRECTION('ref_axis',(2.39882519785021E-33,-1.,3.4920231590332E-16));
#17675=DIRECTION('center_axis',(7.97031498468594E-17,3.4920231590332E-16,
1.));
#17676=DIRECTION('ref_axis',(2.39882519785021E-33,-1.,3.4920231590332E-16));
#17677=DIRECTION('center_axis',(7.97031498468594E-17,3.4920231590332E-16,
1.));
#17678=DIRECTION('ref_axis',(2.39882519785021E-33,-1.,3.4920231590332E-16));
#17679=DIRECTION('center_axis',(-0.974927912181823,-0.222520933956318,6.92755669385935E-17));
#17680=DIRECTION('ref_axis',(0.,3.11321571893962E-16,1.));
#17681=DIRECTION('center_axis',(1.79091352057932E-16,2.24573452299036E-16,
1.));
#17682=DIRECTION('ref_axis',(-0.222520933956318,0.974927912181823,-1.79091352057933E-16));
#17683=DIRECTION('center_axis',(1.79091352057932E-16,2.24573452299036E-16,
1.));
#17684=DIRECTION('ref_axis',(-0.222520933956318,0.974927912181823,-1.79091352057933E-16));
#17685=DIRECTION('center_axis',(1.79091352057932E-16,2.24573452299036E-16,
1.));
#17686=DIRECTION('ref_axis',(-0.222520933956318,0.974927912181823,-1.79091352057933E-16));
#17687=DIRECTION('center_axis',(0.974927912181823,0.222520933956318,-2.24573452299036E-16));
#17688=DIRECTION('ref_axis',(-1.64444757441796E-16,-2.88744376156862E-16,
-1.));
#17689=DIRECTION('center_axis',(0.974927912181823,0.222520933956318,-2.24573452299036E-16));
#17690=DIRECTION('ref_axis',(-1.64444757441796E-16,-2.88744376156862E-16,
-1.));
#17691=DIRECTION('center_axis',(-0.433883739117553,-0.900968867902422,3.4920231590332E-16));
#17692=DIRECTION('ref_axis',(0.,-4.21482754514395E-16,-1.));
#17693=DIRECTION('center_axis',(0.433883739117553,0.900968867902422,-3.4920231590332E-16));
#17694=DIRECTION('ref_axis',(1.97058769816641E-17,-3.97075180104293E-16,
-1.));
#17695=DIRECTION('center_axis',(-0.900968867902422,0.433883739117553,-2.28593141877839E-16));
#17696=DIRECTION('ref_axis',(0.,5.26853443142994E-16,1.));
#17697=DIRECTION('center_axis',(0.433883739117553,0.900968867902422,-3.4920231590332E-16));
#17698=DIRECTION('ref_axis',(1.97058769816641E-17,-3.97075180104293E-16,
-1.));
#17699=DIRECTION('center_axis',(-0.900968867902422,0.433883739117552,-3.33523066916777E-16));
#17700=DIRECTION('ref_axis',(0.,-4.9811451503034E-16,-1.));
#17701=DIRECTION('center_axis',(-7.97031498468617E-17,3.49202315903319E-16,
1.));
#17702=DIRECTION('ref_axis',(-2.39882519785018E-33,-1.,3.49202315903319E-16));
#17703=DIRECTION('center_axis',(-7.97031498468617E-17,3.49202315903319E-16,
1.));
#17704=DIRECTION('ref_axis',(-2.39882519785018E-33,-1.,3.49202315903319E-16));
#17705=DIRECTION('center_axis',(-7.97031498468617E-17,3.49202315903319E-16,
1.));
#17706=DIRECTION('ref_axis',(-2.39882519785018E-33,-1.,3.49202315903319E-16));
#17707=DIRECTION('center_axis',(-0.433883739117552,-0.900968867902422,5.60982088365811E-16));
#17708=DIRECTION('ref_axis',(0.,6.22643143787925E-16,1.));
#17709=DIRECTION('center_axis',(7.97031498468594E-17,3.4920231590332E-16,
1.));
#17710=DIRECTION('ref_axis',(-0.900968867902422,0.433883739117553,-7.97031498468594E-17));
#17711=DIRECTION('center_axis',(7.97031498468594E-17,3.4920231590332E-16,
1.));
#17712=DIRECTION('ref_axis',(-0.900968867902422,0.433883739117553,-7.97031498468594E-17));
#17713=DIRECTION('center_axis',(7.97031498468594E-17,3.4920231590332E-16,
1.));
#17714=DIRECTION('ref_axis',(-0.900968867902422,0.433883739117553,-7.97031498468594E-17));
#17715=DIRECTION('center_axis',(0.433883739117553,0.900968867902422,-3.4920231590332E-16));
#17716=DIRECTION('ref_axis',(4.4891409918625E-17,-4.09203893527874E-16,
-1.));
#17717=DIRECTION('center_axis',(0.433883739117553,0.900968867902422,-3.4920231590332E-16));
#17718=DIRECTION('ref_axis',(4.48914099186251E-17,-4.09203893527874E-16,
-1.));
#17719=DIRECTION('center_axis',(0.433883739117565,-0.900968867902416,3.49202315903319E-16));
#17720=DIRECTION('ref_axis',(0.,-4.21482754514395E-16,-1.));
#17721=DIRECTION('center_axis',(-0.433883739117565,0.900968867902416,-3.49202315903319E-16));
#17722=DIRECTION('ref_axis',(-1.97058769816642E-17,-3.97075180104295E-16,
-1.));
#17723=DIRECTION('center_axis',(-0.900968867902416,-0.433883739117565,2.28593141877845E-16));
#17724=DIRECTION('ref_axis',(0.,5.26853443142994E-16,1.));
#17725=DIRECTION('center_axis',(-0.433883739117565,0.900968867902416,-3.49202315903319E-16));
#17726=DIRECTION('ref_axis',(-1.97058769816642E-17,-3.97075180104295E-16,
-1.));
#17727=DIRECTION('center_axis',(-0.900968867902416,-0.433883739117565,8.85937070873124E-17));
#17728=DIRECTION('ref_axis',(0.,-4.9811451503034E-16,-1.));
#17729=DIRECTION('center_axis',(-1.79091352057933E-16,2.24573452299033E-16,
1.));
#17730=DIRECTION('ref_axis',(5.50003967499563E-33,-1.,2.24573452299033E-16));
#17731=DIRECTION('center_axis',(-1.79091352057933E-16,2.24573452299033E-16,
1.));
#17732=DIRECTION('ref_axis',(5.50003967499563E-33,-1.,2.24573452299033E-16));
#17733=DIRECTION('center_axis',(-1.79091352057933E-16,2.24573452299033E-16,
1.));
#17734=DIRECTION('ref_axis',(5.50003967499563E-33,-1.,2.24573452299033E-16));
#17735=DIRECTION('center_axis',(0.433883739117565,-0.900968867902416,5.60982088365808E-16));
#17736=DIRECTION('ref_axis',(0.,6.22643143787925E-16,1.));
#17737=DIRECTION('center_axis',(-7.97031498468617E-17,3.49202315903319E-16,
1.));
#17738=DIRECTION('ref_axis',(-0.900968867902416,-0.433883739117565,7.97031498468616E-17));
#17739=DIRECTION('center_axis',(-7.97031498468617E-17,3.49202315903319E-16,
1.));
#17740=DIRECTION('ref_axis',(-0.900968867902416,-0.433883739117565,7.97031498468616E-17));
#17741=DIRECTION('center_axis',(-7.97031498468617E-17,3.49202315903319E-16,
1.));
#17742=DIRECTION('ref_axis',(-0.900968867902416,-0.433883739117565,7.97031498468616E-17));
#17743=DIRECTION('center_axis',(-0.433883739117565,0.900968867902416,-3.49202315903319E-16));
#17744=DIRECTION('ref_axis',(-4.48914099186257E-17,-4.09203893527877E-16,
-1.));
#17745=DIRECTION('center_axis',(-0.433883739117565,0.900968867902416,-3.49202315903319E-16));
#17746=DIRECTION('ref_axis',(-4.48914099186258E-17,-4.09203893527877E-16,
-1.));
#17747=DIRECTION('center_axis',(0.974927912181826,-0.222520933956305,2.24573452299033E-16));
#17748=DIRECTION('ref_axis',(0.,-2.10741377257197E-16,-1.));
#17749=DIRECTION('center_axis',(-0.974927912181826,0.222520933956305,-2.24573452299033E-16));
#17750=DIRECTION('ref_axis',(1.71433215598957E-16,-2.58125940401651E-16,
-1.));
#17751=DIRECTION('center_axis',(-0.222520933956305,-0.974927912181826,1.28411031837301E-16));
#17752=DIRECTION('ref_axis',(0.,1.31713360785748E-16,1.));
#17753=DIRECTION('center_axis',(-0.974927912181826,0.222520933956305,-2.24573452299033E-16));
#17754=DIRECTION('ref_axis',(1.71433215598957E-16,-2.58125940401651E-16,
-1.));
#17755=DIRECTION('center_axis',(-0.222520933956305,-0.974927912181826,1.14657265478815E-16));
#17756=DIRECTION('ref_axis',(0.,-1.24528628757585E-16,-1.));
#17757=DIRECTION('center_axis',(-1.43620113371564E-16,6.91638013500039E-17,
1.));
#17758=DIRECTION('ref_axis',(1.,1.10509814492259E-33,1.43620113371564E-16));
#17759=DIRECTION('center_axis',(-1.43620113371564E-16,6.91638013500039E-17,
1.));
#17760=DIRECTION('ref_axis',(1.,1.10509814492259E-33,1.43620113371564E-16));
#17761=DIRECTION('center_axis',(-1.43620113371564E-16,6.91638013500039E-17,
1.));
#17762=DIRECTION('ref_axis',(1.,1.10509814492259E-33,1.43620113371564E-16));
#17763=DIRECTION('center_axis',(0.974927912181826,-0.222520933956305,3.46377834692947E-17));
#17764=DIRECTION('ref_axis',(0.,1.55660785946981E-16,1.));
#17765=DIRECTION('center_axis',(-1.79091352057933E-16,2.24573452299033E-16,
1.));
#17766=DIRECTION('ref_axis',(-0.222520933956305,-0.974927912181826,1.79091352057932E-16));
#17767=DIRECTION('center_axis',(-1.79091352057933E-16,2.24573452299033E-16,
1.));
#17768=DIRECTION('ref_axis',(-0.222520933956305,-0.974927912181826,1.79091352057932E-16));
#17769=DIRECTION('center_axis',(-1.79091352057933E-16,2.24573452299033E-16,
1.));
#17770=DIRECTION('ref_axis',(-0.222520933956305,-0.974927912181826,1.79091352057932E-16));
#17771=DIRECTION('center_axis',(-0.974927912181826,0.222520933956305,-2.24573452299033E-16));
#17772=DIRECTION('ref_axis',(1.64444757441797E-16,-2.8874437615686E-16,
-1.));
#17773=DIRECTION('center_axis',(-0.974927912181826,0.222520933956305,-2.24573452299033E-16));
#17774=DIRECTION('ref_axis',(1.64444757441797E-16,-2.8874437615686E-16,
-1.));
#17775=DIRECTION('center_axis',(0.781831482468022,0.623489801858743,6.91638013500039E-17));
#17776=DIRECTION('ref_axis',(0.,0.,-1.));
#17777=DIRECTION('center_axis',(-0.781831482468022,-0.623489801858743,-6.91638013500039E-17));
#17778=DIRECTION('ref_axis',(5.40744373425973E-17,4.31229247995114E-17,
-1.));
#17779=DIRECTION('center_axis',(0.623489801858743,-0.781831482468022,-2.05955304247934E-16));
#17780=DIRECTION('ref_axis',(0.,-2.63426721571497E-16,1.));
#17781=DIRECTION('center_axis',(-0.781831482468022,-0.623489801858743,-6.91638013500039E-17));
#17782=DIRECTION('ref_axis',(5.40744373425973E-17,4.31229247995114E-17,
-1.));
#17783=DIRECTION('center_axis',(0.623489801858743,-0.781831482468022,-1.22464679914735E-16));
#17784=DIRECTION('ref_axis',(0.,0.,-1.));
#17785=DIRECTION('center_axis',(0.,0.,-1.));
#17786=DIRECTION('ref_axis',(1.,0.,0.));
#17787=DIRECTION('center_axis',(0.781831482468022,0.623489801858743,0.));
#17788=DIRECTION('ref_axis',(0.,0.,1.));
#17789=DIRECTION('center_axis',(-1.43620113371564E-16,6.91638013500039E-17,
1.));
#17790=DIRECTION('ref_axis',(0.623489801858743,-0.781831482468022,1.43620113371564E-16));
#17791=DIRECTION('center_axis',(-1.43620113371564E-16,6.91638013500039E-17,
1.));
#17792=DIRECTION('ref_axis',(0.623489801858743,-0.781831482468022,1.43620113371564E-16));
#17793=DIRECTION('center_axis',(-1.43620113371564E-16,6.91638013500039E-17,
1.));
#17794=DIRECTION('ref_axis',(0.623489801858743,-0.781831482468022,1.43620113371564E-16));
#17795=DIRECTION('center_axis',(0.,0.,-1.));
#17796=DIRECTION('ref_axis',(1.,0.,0.));
#17797=DIRECTION('center_axis',(0.,0.,-1.));
#17798=DIRECTION('ref_axis',(1.,0.,0.));
#17799=DIRECTION('center_axis',(-0.781831482468022,-0.623489801858743,-6.91638013500039E-17));
#17800=DIRECTION('ref_axis',(5.40744373425973E-17,4.31229247995114E-17,
-1.));
#17801=DIRECTION('center_axis',(-0.781831482468022,-0.623489801858743,-6.91638013500039E-17));
#17802=DIRECTION('ref_axis',(5.40744373425973E-17,4.31229247995114E-17,
-1.));
#17803=DIRECTION('center_axis',(1.,0.,-1.22464679914735E-16));
#17804=DIRECTION('ref_axis',(-6.12323399573677E-17,0.,-1.));
#17805=DIRECTION('center_axis',(1.43620113371566E-16,6.91638013500059E-17,
1.));
#17806=DIRECTION('ref_axis',(1.,-1.10509814492274E-33,-1.43620113371566E-16));
#17807=DIRECTION('center_axis',(1.43620113371566E-16,6.91638013500059E-17,
1.));
#17808=DIRECTION('ref_axis',(1.,-1.10509814492274E-33,-1.43620113371566E-16));
#17809=DIRECTION('center_axis',(1.43620113371566E-16,6.91638013500059E-17,
1.));
#17810=DIRECTION('ref_axis',(1.,-1.10509814492274E-33,-1.43620113371566E-16));
#17811=DIRECTION('center_axis',(0.,1.,0.));
#17812=DIRECTION('ref_axis',(6.12323399573677E-17,0.,1.));
#17813=DIRECTION('center_axis',(0.,0.,1.));
#17814=DIRECTION('ref_axis',(1.,0.,0.));
#17815=DIRECTION('center_axis',(0.,0.,1.));
#17816=DIRECTION('ref_axis',(1.,0.,0.));
#17817=DIRECTION('center_axis',(0.,0.,1.));
#17818=DIRECTION('ref_axis',(1.,0.,0.));
#17819=DIRECTION('center_axis',(0.,-1.,0.));
#17820=DIRECTION('ref_axis',(0.,0.,-1.));
#17821=DIRECTION('center_axis',(0.,-1.,0.));
#17822=DIRECTION('ref_axis',(0.,0.,-1.));
#17823=DIRECTION('center_axis',(0.,1.,0.));
#17824=DIRECTION('ref_axis',(0.,0.,-1.));
#17825=DIRECTION('center_axis',(0.,-1.,0.));
#17826=DIRECTION('ref_axis',(0.,0.,-1.));
#17827=DIRECTION('center_axis',(1.,0.,-1.22464679914735E-16));
#17828=DIRECTION('ref_axis',(1.22464679914735E-16,0.,1.));
#17829=DIRECTION('center_axis',(0.,-1.,0.));
#17830=DIRECTION('ref_axis',(0.,0.,-1.));
#17831=DIRECTION('center_axis',(0.,0.,-1.));
#17832=DIRECTION('ref_axis',(-1.,0.,0.));
#17833=DIRECTION('center_axis',(0.,0.,-1.));
#17834=DIRECTION('ref_axis',(1.,0.,0.));
#17835=DIRECTION('center_axis',(0.,0.,-1.));
#17836=DIRECTION('ref_axis',(1.,0.,0.));
#17837=DIRECTION('center_axis',(0.,0.,-1.));
#17838=DIRECTION('ref_axis',(-1.,0.,0.));
#17839=DIRECTION('center_axis',(0.,0.,1.));
#17840=DIRECTION('ref_axis',(1.,0.,0.));
#17841=DIRECTION('center_axis',(0.,0.,1.));
#17842=DIRECTION('ref_axis',(1.,0.,0.));
#17843=DIRECTION('center_axis',(0.,0.,1.));
#17844=DIRECTION('ref_axis',(1.,0.,0.));
#17845=DIRECTION('center_axis',(0.,0.,1.));
#17846=DIRECTION('ref_axis',(1.,0.,0.));
#17847=DIRECTION('center_axis',(0.,-1.,0.));
#17848=DIRECTION('ref_axis',(0.,0.,-1.));
#17849=DIRECTION('center_axis',(0.,1.,0.));
#17850=DIRECTION('ref_axis',(0.,0.,1.));
#17851=DIRECTION('center_axis',(0.,0.,1.));
#17852=DIRECTION('ref_axis',(1.,0.,0.));
#17853=DIRECTION('center_axis',(0.,0.,-1.));
#17854=DIRECTION('ref_axis',(1.,0.,0.));
#17855=DIRECTION('center_axis',(0.,0.,1.));
#17856=DIRECTION('ref_axis',(1.,0.,0.));
#17857=DIRECTION('center_axis',(0.,0.,1.));
#17858=DIRECTION('ref_axis',(1.,0.,0.));
#17859=DIRECTION('center_axis',(0.,0.,1.));
#17860=DIRECTION('ref_axis',(1.,0.,0.));
#17861=DIRECTION('center_axis',(0.,0.,-1.));
#17862=DIRECTION('ref_axis',(1.,0.,0.));
#17863=DIRECTION('center_axis',(0.,0.,-1.));
#17864=DIRECTION('ref_axis',(-1.,0.,0.));
#17865=DIRECTION('center_axis',(0.,0.,-1.));
#17866=DIRECTION('ref_axis',(-1.,0.,0.));
#17867=DIRECTION('center_axis',(0.781831482468022,0.623489801858743,6.91638013500039E-17));
#17868=DIRECTION('ref_axis',(-1.43620113371564E-16,6.91638013500039E-17,
1.));
#17869=DIRECTION('center_axis',(-0.781831482468022,-0.623489801858743,-6.91638013500039E-17));
#17870=DIRECTION('ref_axis',(1.43620113371564E-16,-6.91638013500039E-17,
-1.));
#17871=DIRECTION('center_axis',(-1.43620113371564E-16,6.91638013500039E-17,
1.));
#17872=DIRECTION('ref_axis',(0.623489801858743,-0.781831482468022,1.43620113371564E-16));
#17873=DIRECTION('center_axis',(-1.43620113371564E-16,6.91638013500039E-17,
1.));
#17874=DIRECTION('ref_axis',(0.623489801858743,-0.781831482468022,1.43620113371564E-16));
#17875=DIRECTION('center_axis',(1.43620113371564E-16,-6.91638013500039E-17,
-1.));
#17876=DIRECTION('ref_axis',(0.623489801858743,-0.781831482468022,1.43620113371564E-16));
#17877=DIRECTION('center_axis',(-1.43620113371564E-16,6.91638013500039E-17,
1.));
#17878=DIRECTION('ref_axis',(0.623489801858743,-0.781831482468022,1.43620113371564E-16));
#17879=DIRECTION('center_axis',(1.43620113371564E-16,-6.91638013500039E-17,
-1.));
#17880=DIRECTION('ref_axis',(0.623489801858743,-0.781831482468022,1.43620113371564E-16));
#17881=DIRECTION('center_axis',(-1.43620113371564E-16,6.91638013500039E-17,
1.));
#17882=DIRECTION('ref_axis',(0.623489801858743,-0.781831482468022,1.43620113371564E-16));
#17883=DIRECTION('center_axis',(1.43620113371564E-16,-6.91638013500039E-17,
-1.));
#17884=DIRECTION('ref_axis',(-0.623489801858743,0.781831482468022,-1.43620113371564E-16));
#17885=DIRECTION('center_axis',(1.43620113371564E-16,-6.91638013500039E-17,
-1.));
#17886=DIRECTION('ref_axis',(-0.623489801858743,0.781831482468022,-1.43620113371564E-16));
#17887=DIRECTION('center_axis',(1.79091352057933E-16,-2.24573452299033E-16,
-1.));
#17888=DIRECTION('ref_axis',(0.222520933956305,0.974927912181826,-1.79091352057932E-16));
#17889=DIRECTION('center_axis',(1.79091352057933E-16,-2.24573452299033E-16,
-1.));
#17890=DIRECTION('ref_axis',(-0.222520933956305,-0.974927912181826,1.79091352057932E-16));
#17891=DIRECTION('center_axis',(1.79091352057933E-16,-2.24573452299033E-16,
-1.));
#17892=DIRECTION('ref_axis',(-0.222520933956305,-0.974927912181826,1.79091352057932E-16));
#17893=DIRECTION('center_axis',(1.79091352057933E-16,-2.24573452299033E-16,
-1.));
#17894=DIRECTION('ref_axis',(0.222520933956305,0.974927912181826,-1.79091352057932E-16));
#17895=DIRECTION('center_axis',(-1.79091352057933E-16,2.24573452299033E-16,
1.));
#17896=DIRECTION('ref_axis',(-0.222520933956305,-0.974927912181826,1.79091352057932E-16));
#17897=DIRECTION('center_axis',(-1.79091352057933E-16,2.24573452299033E-16,
1.));
#17898=DIRECTION('ref_axis',(-0.222520933956305,-0.974927912181826,1.79091352057932E-16));
#17899=DIRECTION('center_axis',(-1.79091352057933E-16,2.24573452299033E-16,
1.));
#17900=DIRECTION('ref_axis',(-0.222520933956305,-0.974927912181826,1.79091352057932E-16));
#17901=DIRECTION('center_axis',(-1.79091352057933E-16,2.24573452299033E-16,
1.));
#17902=DIRECTION('ref_axis',(-0.222520933956305,-0.974927912181826,1.79091352057932E-16));
#17903=DIRECTION('center_axis',(0.974927912181826,-0.222520933956305,2.24573452299033E-16));
#17904=DIRECTION('ref_axis',(-1.79091352057933E-16,2.24573452299033E-16,
1.));
#17905=DIRECTION('center_axis',(-0.974927912181826,0.222520933956305,-2.24573452299033E-16));
#17906=DIRECTION('ref_axis',(1.79091352057933E-16,-2.24573452299033E-16,
-1.));
#17907=DIRECTION('center_axis',(-1.79091352057933E-16,2.24573452299033E-16,
1.));
#17908=DIRECTION('ref_axis',(-0.222520933956305,-0.974927912181826,1.79091352057932E-16));
#17909=DIRECTION('center_axis',(-1.79091352057933E-16,2.24573452299033E-16,
1.));
#17910=DIRECTION('ref_axis',(-0.222520933956305,-0.974927912181826,1.79091352057932E-16));
#17911=DIRECTION('center_axis',(1.79091352057933E-16,-2.24573452299033E-16,
-1.));
#17912=DIRECTION('ref_axis',(-0.222520933956305,-0.974927912181826,1.79091352057932E-16));
#17913=DIRECTION('center_axis',(-1.79091352057933E-16,2.24573452299033E-16,
1.));
#17914=DIRECTION('ref_axis',(-0.222520933956305,-0.974927912181826,1.79091352057932E-16));
#17915=DIRECTION('center_axis',(1.79091352057933E-16,-2.24573452299033E-16,
-1.));
#17916=DIRECTION('ref_axis',(-0.222520933956305,-0.974927912181826,1.79091352057932E-16));
#17917=DIRECTION('center_axis',(-1.79091352057933E-16,2.24573452299033E-16,
1.));
#17918=DIRECTION('ref_axis',(-0.222520933956305,-0.974927912181826,1.79091352057932E-16));
#17919=DIRECTION('center_axis',(1.79091352057933E-16,-2.24573452299033E-16,
-1.));
#17920=DIRECTION('ref_axis',(0.222520933956305,0.974927912181826,-1.79091352057932E-16));
#17921=DIRECTION('center_axis',(1.79091352057933E-16,-2.24573452299033E-16,
-1.));
#17922=DIRECTION('ref_axis',(0.222520933956305,0.974927912181826,-1.79091352057932E-16));
#17923=DIRECTION('center_axis',(7.97031498468617E-17,-3.49202315903319E-16,
-1.));
#17924=DIRECTION('ref_axis',(0.900968867902416,0.433883739117565,-7.97031498468616E-17));
#17925=DIRECTION('center_axis',(7.97031498468617E-17,-3.49202315903319E-16,
-1.));
#17926=DIRECTION('ref_axis',(-0.900968867902416,-0.433883739117565,7.97031498468616E-17));
#17927=DIRECTION('center_axis',(7.97031498468617E-17,-3.49202315903319E-16,
-1.));
#17928=DIRECTION('ref_axis',(-0.900968867902416,-0.433883739117565,7.97031498468616E-17));
#17929=DIRECTION('center_axis',(7.97031498468617E-17,-3.49202315903319E-16,
-1.));
#17930=DIRECTION('ref_axis',(0.900968867902416,0.433883739117565,-7.97031498468616E-17));
#17931=DIRECTION('center_axis',(-7.97031498468617E-17,3.49202315903319E-16,
1.));
#17932=DIRECTION('ref_axis',(-0.900968867902416,-0.433883739117565,7.97031498468616E-17));
#17933=DIRECTION('center_axis',(-7.97031498468617E-17,3.49202315903319E-16,
1.));
#17934=DIRECTION('ref_axis',(-0.900968867902416,-0.433883739117565,7.97031498468616E-17));
#17935=DIRECTION('center_axis',(-7.97031498468617E-17,3.49202315903319E-16,
1.));
#17936=DIRECTION('ref_axis',(-0.900968867902416,-0.433883739117565,7.97031498468616E-17));
#17937=DIRECTION('center_axis',(-7.97031498468617E-17,3.49202315903319E-16,
1.));
#17938=DIRECTION('ref_axis',(-0.900968867902416,-0.433883739117565,7.97031498468616E-17));
#17939=DIRECTION('center_axis',(0.433883739117565,-0.900968867902416,3.49202315903319E-16));
#17940=DIRECTION('ref_axis',(-7.97031498468617E-17,3.49202315903319E-16,
1.));
#17941=DIRECTION('center_axis',(-0.433883739117565,0.900968867902416,-3.49202315903319E-16));
#17942=DIRECTION('ref_axis',(7.97031498468617E-17,-3.49202315903319E-16,
-1.));
#17943=DIRECTION('center_axis',(-7.97031498468617E-17,3.49202315903319E-16,
1.));
#17944=DIRECTION('ref_axis',(-0.900968867902416,-0.433883739117565,7.97031498468616E-17));
#17945=DIRECTION('center_axis',(-7.97031498468617E-17,3.49202315903319E-16,
1.));
#17946=DIRECTION('ref_axis',(-0.900968867902416,-0.433883739117565,7.97031498468616E-17));
#17947=DIRECTION('center_axis',(7.97031498468617E-17,-3.49202315903319E-16,
-1.));
#17948=DIRECTION('ref_axis',(-0.900968867902416,-0.433883739117565,7.97031498468616E-17));
#17949=DIRECTION('center_axis',(-7.97031498468617E-17,3.49202315903319E-16,
1.));
#17950=DIRECTION('ref_axis',(-0.900968867902416,-0.433883739117565,7.97031498468616E-17));
#17951=DIRECTION('center_axis',(7.97031498468617E-17,-3.49202315903319E-16,
-1.));
#17952=DIRECTION('ref_axis',(-0.900968867902416,-0.433883739117565,7.97031498468616E-17));
#17953=DIRECTION('center_axis',(-7.97031498468617E-17,3.49202315903319E-16,
1.));
#17954=DIRECTION('ref_axis',(-0.900968867902416,-0.433883739117565,7.97031498468616E-17));
#17955=DIRECTION('center_axis',(7.97031498468617E-17,-3.49202315903319E-16,
-1.));
#17956=DIRECTION('ref_axis',(0.900968867902416,0.433883739117565,-7.97031498468616E-17));
#17957=DIRECTION('center_axis',(7.97031498468617E-17,-3.49202315903319E-16,
-1.));
#17958=DIRECTION('ref_axis',(0.900968867902416,0.433883739117565,-7.97031498468616E-17));
#17959=DIRECTION('center_axis',(-7.97031498468594E-17,-3.4920231590332E-16,
-1.));
#17960=DIRECTION('ref_axis',(0.900968867902422,-0.433883739117553,7.97031498468594E-17));
#17961=DIRECTION('center_axis',(-7.97031498468594E-17,-3.4920231590332E-16,
-1.));
#17962=DIRECTION('ref_axis',(-0.900968867902422,0.433883739117553,-7.97031498468594E-17));
#17963=DIRECTION('center_axis',(-7.97031498468594E-17,-3.4920231590332E-16,
-1.));
#17964=DIRECTION('ref_axis',(-0.900968867902422,0.433883739117553,-7.97031498468594E-17));
#17965=DIRECTION('center_axis',(-7.97031498468594E-17,-3.4920231590332E-16,
-1.));
#17966=DIRECTION('ref_axis',(0.900968867902422,-0.433883739117553,7.97031498468594E-17));
#17967=DIRECTION('center_axis',(7.97031498468594E-17,3.4920231590332E-16,
1.));
#17968=DIRECTION('ref_axis',(-0.900968867902422,0.433883739117553,-7.97031498468594E-17));
#17969=DIRECTION('center_axis',(7.97031498468594E-17,3.4920231590332E-16,
1.));
#17970=DIRECTION('ref_axis',(-0.900968867902422,0.433883739117553,-7.97031498468594E-17));
#17971=DIRECTION('center_axis',(7.97031498468594E-17,3.4920231590332E-16,
1.));
#17972=DIRECTION('ref_axis',(-0.900968867902422,0.433883739117553,-7.97031498468594E-17));
#17973=DIRECTION('center_axis',(7.97031498468594E-17,3.4920231590332E-16,
1.));
#17974=DIRECTION('ref_axis',(-0.900968867902422,0.433883739117553,-7.97031498468594E-17));
#17975=DIRECTION('center_axis',(-0.433883739117553,-0.900968867902422,3.4920231590332E-16));
#17976=DIRECTION('ref_axis',(7.97031498468594E-17,3.4920231590332E-16,1.));
#17977=DIRECTION('center_axis',(0.433883739117553,0.900968867902422,-3.4920231590332E-16));
#17978=DIRECTION('ref_axis',(-7.97031498468594E-17,-3.4920231590332E-16,
-1.));
#17979=DIRECTION('center_axis',(7.97031498468594E-17,3.4920231590332E-16,
1.));
#17980=DIRECTION('ref_axis',(-0.900968867902422,0.433883739117553,-7.97031498468594E-17));
#17981=DIRECTION('center_axis',(7.97031498468594E-17,3.4920231590332E-16,
1.));
#17982=DIRECTION('ref_axis',(-0.900968867902422,0.433883739117553,-7.97031498468594E-17));
#17983=DIRECTION('center_axis',(-7.97031498468594E-17,-3.4920231590332E-16,
-1.));
#17984=DIRECTION('ref_axis',(-0.900968867902422,0.433883739117553,-7.97031498468594E-17));
#17985=DIRECTION('center_axis',(7.97031498468594E-17,3.4920231590332E-16,
1.));
#17986=DIRECTION('ref_axis',(-0.900968867902422,0.433883739117553,-7.97031498468594E-17));
#17987=DIRECTION('center_axis',(-7.97031498468594E-17,-3.4920231590332E-16,
-1.));
#17988=DIRECTION('ref_axis',(-0.900968867902422,0.433883739117553,-7.97031498468594E-17));
#17989=DIRECTION('center_axis',(7.97031498468594E-17,3.4920231590332E-16,
1.));
#17990=DIRECTION('ref_axis',(-0.900968867902422,0.433883739117553,-7.97031498468594E-17));
#17991=DIRECTION('center_axis',(-7.97031498468594E-17,-3.4920231590332E-16,
-1.));
#17992=DIRECTION('ref_axis',(0.900968867902422,-0.433883739117553,7.97031498468594E-17));
#17993=DIRECTION('center_axis',(-7.97031498468594E-17,-3.4920231590332E-16,
-1.));
#17994=DIRECTION('ref_axis',(0.900968867902422,-0.433883739117553,7.97031498468594E-17));
#17995=DIRECTION('center_axis',(-1.79091352057932E-16,-2.24573452299036E-16,
-1.));
#17996=DIRECTION('ref_axis',(0.222520933956318,-0.974927912181823,1.79091352057933E-16));
#17997=DIRECTION('center_axis',(-1.79091352057932E-16,-2.24573452299036E-16,
-1.));
#17998=DIRECTION('ref_axis',(-0.222520933956318,0.974927912181823,-1.79091352057933E-16));
#17999=DIRECTION('center_axis',(-1.79091352057932E-16,-2.24573452299036E-16,
-1.));
#18000=DIRECTION('ref_axis',(-0.222520933956318,0.974927912181823,-1.79091352057933E-16));
#18001=DIRECTION('center_axis',(-1.79091352057932E-16,-2.24573452299036E-16,
-1.));
#18002=DIRECTION('ref_axis',(0.222520933956318,-0.974927912181823,1.79091352057933E-16));
#18003=DIRECTION('center_axis',(1.79091352057932E-16,2.24573452299036E-16,
1.));
#18004=DIRECTION('ref_axis',(-0.222520933956318,0.974927912181823,-1.79091352057933E-16));
#18005=DIRECTION('center_axis',(1.79091352057932E-16,2.24573452299036E-16,
1.));
#18006=DIRECTION('ref_axis',(-0.222520933956318,0.974927912181823,-1.79091352057933E-16));
#18007=DIRECTION('center_axis',(1.79091352057932E-16,2.24573452299036E-16,
1.));
#18008=DIRECTION('ref_axis',(-0.222520933956318,0.974927912181823,-1.79091352057933E-16));
#18009=DIRECTION('center_axis',(1.79091352057932E-16,2.24573452299036E-16,
1.));
#18010=DIRECTION('ref_axis',(-0.222520933956318,0.974927912181823,-1.79091352057933E-16));
#18011=DIRECTION('center_axis',(-0.974927912181823,-0.222520933956318,2.24573452299036E-16));
#18012=DIRECTION('ref_axis',(1.79091352057932E-16,2.24573452299036E-16,
1.));
#18013=DIRECTION('center_axis',(0.974927912181823,0.222520933956318,-2.24573452299036E-16));
#18014=DIRECTION('ref_axis',(-1.79091352057932E-16,-2.24573452299036E-16,
-1.));
#18015=DIRECTION('center_axis',(1.79091352057932E-16,2.24573452299036E-16,
1.));
#18016=DIRECTION('ref_axis',(-0.222520933956318,0.974927912181823,-1.79091352057933E-16));
#18017=DIRECTION('center_axis',(1.79091352057932E-16,2.24573452299036E-16,
1.));
#18018=DIRECTION('ref_axis',(-0.222520933956318,0.974927912181823,-1.79091352057933E-16));
#18019=DIRECTION('center_axis',(-1.79091352057932E-16,-2.24573452299036E-16,
-1.));
#18020=DIRECTION('ref_axis',(-0.222520933956318,0.974927912181823,-1.79091352057933E-16));
#18021=DIRECTION('center_axis',(1.79091352057932E-16,2.24573452299036E-16,
1.));
#18022=DIRECTION('ref_axis',(-0.222520933956318,0.974927912181823,-1.79091352057933E-16));
#18023=DIRECTION('center_axis',(-1.79091352057932E-16,-2.24573452299036E-16,
-1.));
#18024=DIRECTION('ref_axis',(-0.222520933956318,0.974927912181823,-1.79091352057933E-16));
#18025=DIRECTION('center_axis',(1.79091352057932E-16,2.24573452299036E-16,
1.));
#18026=DIRECTION('ref_axis',(-0.222520933956318,0.974927912181823,-1.79091352057933E-16));
#18027=DIRECTION('center_axis',(-1.79091352057932E-16,-2.24573452299036E-16,
-1.));
#18028=DIRECTION('ref_axis',(0.222520933956318,-0.974927912181823,1.79091352057933E-16));
#18029=DIRECTION('center_axis',(-1.79091352057932E-16,-2.24573452299036E-16,
-1.));
#18030=DIRECTION('ref_axis',(0.222520933956318,-0.974927912181823,1.79091352057933E-16));
#18031=DIRECTION('center_axis',(-1.43620113371566E-16,-6.91638013500059E-17,
-1.));
#18032=DIRECTION('ref_axis',(-0.623489801858732,-0.781831482468031,1.43620113371566E-16));
#18033=DIRECTION('center_axis',(-1.43620113371566E-16,-6.91638013500059E-17,
-1.));
#18034=DIRECTION('ref_axis',(0.623489801858732,0.781831482468031,-1.43620113371566E-16));
#18035=DIRECTION('center_axis',(-1.43620113371566E-16,-6.91638013500059E-17,
-1.));
#18036=DIRECTION('ref_axis',(0.623489801858732,0.781831482468031,-1.43620113371566E-16));
#18037=DIRECTION('center_axis',(-1.43620113371566E-16,-6.91638013500059E-17,
-1.));
#18038=DIRECTION('ref_axis',(-0.623489801858732,-0.781831482468031,1.43620113371566E-16));
#18039=DIRECTION('center_axis',(1.43620113371566E-16,6.91638013500059E-17,
1.));
#18040=DIRECTION('ref_axis',(0.623489801858732,0.781831482468031,-1.43620113371566E-16));
#18041=DIRECTION('center_axis',(1.43620113371566E-16,6.91638013500059E-17,
1.));
#18042=DIRECTION('ref_axis',(0.623489801858732,0.781831482468031,-1.43620113371566E-16));
#18043=DIRECTION('center_axis',(1.43620113371566E-16,6.91638013500059E-17,
1.));
#18044=DIRECTION('ref_axis',(0.623489801858732,0.781831482468031,-1.43620113371566E-16));
#18045=DIRECTION('center_axis',(1.43620113371566E-16,6.91638013500059E-17,
1.));
#18046=DIRECTION('ref_axis',(0.623489801858732,0.781831482468031,-1.43620113371566E-16));
#18047=DIRECTION('center_axis',(-0.781831482468031,0.623489801858732,6.91638013500059E-17));
#18048=DIRECTION('ref_axis',(1.43620113371566E-16,6.91638013500061E-17,
1.));
#18049=DIRECTION('center_axis',(0.781831482468031,-0.623489801858732,-6.91638013500059E-17));
#18050=DIRECTION('ref_axis',(-1.43620113371566E-16,-6.91638013500061E-17,
-1.));
#18051=DIRECTION('center_axis',(1.43620113371566E-16,6.91638013500059E-17,
1.));
#18052=DIRECTION('ref_axis',(0.623489801858732,0.781831482468031,-1.43620113371566E-16));
#18053=DIRECTION('center_axis',(1.43620113371566E-16,6.91638013500059E-17,
1.));
#18054=DIRECTION('ref_axis',(0.623489801858732,0.781831482468031,-1.43620113371566E-16));
#18055=DIRECTION('center_axis',(-1.43620113371566E-16,-6.91638013500059E-17,
-1.));
#18056=DIRECTION('ref_axis',(0.623489801858732,0.781831482468031,-1.43620113371566E-16));
#18057=DIRECTION('center_axis',(1.43620113371566E-16,6.91638013500059E-17,
1.));
#18058=DIRECTION('ref_axis',(0.623489801858732,0.781831482468031,-1.43620113371566E-16));
#18059=DIRECTION('center_axis',(-1.43620113371566E-16,-6.91638013500059E-17,
-1.));
#18060=DIRECTION('ref_axis',(0.623489801858732,0.781831482468031,-1.43620113371566E-16));
#18061=DIRECTION('center_axis',(1.43620113371566E-16,6.91638013500059E-17,
1.));
#18062=DIRECTION('ref_axis',(0.623489801858732,0.781831482468031,-1.43620113371566E-16));
#18063=DIRECTION('center_axis',(-1.43620113371566E-16,-6.91638013500059E-17,
-1.));
#18064=DIRECTION('ref_axis',(-0.623489801858732,-0.781831482468031,1.43620113371566E-16));
#18065=DIRECTION('center_axis',(-1.43620113371566E-16,-6.91638013500059E-17,
-1.));
#18066=DIRECTION('ref_axis',(-0.623489801858732,-0.781831482468031,1.43620113371566E-16));
#18067=DIRECTION('center_axis',(0.,0.,1.));
#18068=DIRECTION('ref_axis',(1.,0.,0.));
#18069=DIRECTION('center_axis',(0.,0.,1.));
#18070=DIRECTION('ref_axis',(1.,0.,0.));
#18071=DIRECTION('center_axis',(0.,0.,-1.));
#18072=DIRECTION('ref_axis',(1.,0.,0.));
#18073=DIRECTION('center_axis',(0.,0.,1.));
#18074=DIRECTION('ref_axis',(1.,0.,0.));
#18075=DIRECTION('center_axis',(0.,0.,-1.));
#18076=DIRECTION('ref_axis',(1.,0.,0.));
#18077=DIRECTION('center_axis',(0.,0.,1.));
#18078=DIRECTION('ref_axis',(1.,0.,0.));
#18079=DIRECTION('center_axis',(0.,0.,-1.));
#18080=DIRECTION('ref_axis',(-1.,0.,0.));
#18081=DIRECTION('center_axis',(0.,0.,-1.));
#18082=DIRECTION('ref_axis',(-1.,0.,0.));
#18083=DIRECTION('axis',(0.,0.,1.));
#18084=DIRECTION('refdir',(1.,0.,0.));
#18085=DIRECTION('center_axis',(0.,-1.83697019872103E-16,-1.));
#18086=DIRECTION('ref_axis',(0.,-1.,1.83697019872103E-16));
#18087=DIRECTION('center_axis',(0.,1.83697019872103E-16,1.));
#18088=DIRECTION('ref_axis',(0.,-1.,1.83697019872103E-16));
#18089=DIRECTION('center_axis',(-1.,1.22464679914735E-16,-2.24963967399279E-32));
#18090=DIRECTION('ref_axis',(1.22464679914735E-16,1.,-1.83697019872103E-16));
#18091=DIRECTION('center_axis',(0.,1.83697019872103E-16,1.));
#18092=DIRECTION('ref_axis',(0.,-1.,1.83697019872103E-16));
#18093=DIRECTION('center_axis',(0.,1.83697019872103E-16,1.));
#18094=DIRECTION('ref_axis',(0.,1.,-2.09599627067876E-16));
#18095=DIRECTION('center_axis',(0.,-1.83697019872103E-16,-1.));
#18096=DIRECTION('ref_axis',(0.,1.,-1.83697019872103E-16));
#18097=DIRECTION('center_axis',(1.,1.22464679914735E-16,-2.24963967399279E-32));
#18098=DIRECTION('ref_axis',(1.22464679914735E-16,-1.,1.30999766917423E-16));
#18099=DIRECTION('center_axis',(0.,1.83697019872103E-16,1.));
#18100=DIRECTION('ref_axis',(0.,1.,-1.83697019872103E-16));
#18101=DIRECTION('center_axis',(0.,1.83697019872103E-16,1.));
#18102=DIRECTION('ref_axis',(0.,1.,-1.83697019872103E-16));
#18103=DIRECTION('center_axis',(0.,-1.83697019872103E-16,-1.));
#18104=DIRECTION('ref_axis',(0.,1.,-1.83697019872103E-16));
#18105=DIRECTION('center_axis',(0.,1.83697019872103E-16,1.));
#18106=DIRECTION('ref_axis',(0.,1.,-2.09599627067876E-16));
#18107=DIRECTION('center_axis',(0.,-1.83697019872103E-16,-1.));
#18108=DIRECTION('ref_axis',(0.,1.,-1.83697019872103E-16));
#18109=DIRECTION('center_axis',(1.,1.22464679914735E-16,-2.24963967399279E-32));
#18110=DIRECTION('ref_axis',(1.22464679914735E-16,-1.,1.30999766917423E-16));
#18111=DIRECTION('center_axis',(0.,1.83697019872103E-16,1.));
#18112=DIRECTION('ref_axis',(0.,-1.,1.83697019872103E-16));
#18113=DIRECTION('center_axis',(0.,-1.83697019872103E-16,-1.));
#18114=DIRECTION('ref_axis',(0.,1.,-1.83697019872103E-16));
#18115=DIRECTION('center_axis',(0.,-1.83697019872103E-16,-1.));
#18116=DIRECTION('ref_axis',(0.,-1.,1.83697019872103E-16));
#18117=DIRECTION('',(8.65956056235483E-17,0.707106781186539,-0.707106781186556));
#18118=DIRECTION('center_axis',(0.,1.83697019872103E-16,1.));
#18119=DIRECTION('ref_axis',(0.,-1.,1.83697019872103E-16));
#18120=DIRECTION('center_axis',(0.,1.83697019872103E-16,1.));
#18121=DIRECTION('ref_axis',(0.,-1.,1.83697019872103E-16));
#18122=DIRECTION('',(0.,1.83697019872103E-16,1.));
#18123=DIRECTION('center_axis',(0.,1.83697019872103E-16,1.));
#18124=DIRECTION('ref_axis',(0.,1.,-1.83697019872103E-16));
#18125=DIRECTION('',(8.65956056235483E-17,-0.707106781186539,0.707106781186556));
#18126=DIRECTION('center_axis',(0.,1.83697019872103E-16,1.));
#18127=DIRECTION('ref_axis',(0.,-1.,1.83697019872103E-16));
#18128=DIRECTION('center_axis',(0.,1.83697019872103E-16,1.));
#18129=DIRECTION('ref_axis',(0.,-1.,1.83697019872103E-16));
#18130=DIRECTION('center_axis',(0.,1.83697019872103E-16,1.));
#18131=DIRECTION('ref_axis',(0.,-1.,1.83697019872103E-16));
#18132=DIRECTION('',(0.,-1.83697019872103E-16,-1.));
#18133=DIRECTION('center_axis',(0.,1.83697019872103E-16,1.));
#18134=DIRECTION('ref_axis',(0.,-1.,1.83697019872103E-16));
#18135=DIRECTION('',(0.,-1.83697019872103E-16,-1.));
#18136=DIRECTION('center_axis',(0.,1.83697019872103E-16,1.));
#18137=DIRECTION('ref_axis',(0.,-1.,1.83697019872103E-16));
#18138=DIRECTION('center_axis',(0.,-1.83697019872103E-16,-1.));
#18139=DIRECTION('ref_axis',(0.,1.,-1.83697019872103E-16));
#18140=DIRECTION('center_axis',(0.,1.83697019872103E-16,1.));
#18141=DIRECTION('ref_axis',(0.,-1.,1.83697019872103E-16));
#18142=DIRECTION('center_axis',(-1.,0.,0.));
#18143=DIRECTION('ref_axis',(0.,1.,0.));
#18144=DIRECTION('center_axis',(0.,1.22464679914735E-16,1.));
#18145=DIRECTION('ref_axis',(0.,-1.,1.22464679914735E-16));
#18146=DIRECTION('center_axis',(-0.623489801858732,0.781831482468031,-1.43620113371566E-16));
#18147=DIRECTION('ref_axis',(0.781831482468031,0.623489801858732,6.91638013500061E-17));
#18148=DIRECTION('center_axis',(-4.78733711238555E-17,1.45519280364738E-16,
1.));
#18149=DIRECTION('ref_axis',(-0.781831482468031,-0.623489801858732,5.33008785647293E-17));
#18150=DIRECTION('center_axis',(0.222520933956319,0.974927912181823,-1.79091352057932E-16));
#18151=DIRECTION('ref_axis',(0.974927912181823,-0.222520933956319,2.24573452299036E-16));
#18152=DIRECTION('center_axis',(-5.96971173526444E-17,1.97322497347747E-16,
1.));
#18153=DIRECTION('ref_axis',(-0.974927912181823,0.222520933956319,-1.02108772384301E-16));
#18154=DIRECTION('center_axis',(0.900968867902422,0.433883739117552,-7.97031498468594E-17));
#18155=DIRECTION('ref_axis',(0.433883739117552,-0.900968867902422,3.4920231590332E-16));
#18156=DIRECTION('center_axis',(-2.65677166156194E-17,2.38865451882509E-16,
1.));
#18157=DIRECTION('ref_axis',(-0.433883739117552,0.900968867902422,-2.26737635988585E-16));
#18158=DIRECTION('center_axis',(0.900968867902416,-0.433883739117565,7.97031498468616E-17));
#18159=DIRECTION('ref_axis',(-0.433883739117565,-0.900968867902416,3.49202315903319E-16));
#18160=DIRECTION('center_axis',(2.65677166156204E-17,2.38865451882508E-16,
1.));
#18161=DIRECTION('ref_axis',(0.433883739117565,0.900968867902416,-2.26737635988584E-16));
#18162=DIRECTION('center_axis',(0.222520933956305,-0.974927912181826,1.79091352057933E-16));
#18163=DIRECTION('ref_axis',(-0.974927912181826,-0.222520933956305,2.24573452299033E-16));
#18164=DIRECTION('center_axis',(5.9697117352644E-17,1.97322497347747E-16,
1.));
#18165=DIRECTION('ref_axis',(0.974927912181826,0.222520933956305,-1.02108772384298E-16));
#18166=DIRECTION('center_axis',(-0.623489801858743,-0.781831482468022,1.43620113371564E-16));
#18167=DIRECTION('ref_axis',(-0.781831482468022,0.623489801858743,6.91638013500039E-17));
#18168=DIRECTION('center_axis',(4.78733711238546E-17,1.45519280364737E-16,
1.));
#18169=DIRECTION('ref_axis',(0.781831482468022,-0.623489801858743,5.33008785647315E-17));
#18170=DIRECTION('center_axis',(0.,1.83697019872103E-16,1.));
#18171=DIRECTION('ref_axis',(0.,1.,-1.62614292875575E-16));
#18172=DIRECTION('center_axis',(0.,-1.83697019872103E-16,-1.));
#18173=DIRECTION('ref_axis',(0.,1.,-1.83697019872103E-16));
#18174=DIRECTION('center_axis',(1.,1.22464679914735E-16,-2.24963967399279E-32));
#18175=DIRECTION('ref_axis',(1.22464679914735E-16,-1.,2.03267866094469E-16));
#18176=DIRECTION('center_axis',(0.,1.83697019872103E-16,1.));
#18177=DIRECTION('ref_axis',(0.,1.,-1.83697019872103E-16));
#18178=DIRECTION('center_axis',(0.,1.83697019872103E-16,1.));
#18179=DIRECTION('ref_axis',(0.,1.,-1.83697019872103E-16));
#18180=DIRECTION('center_axis',(0.,-1.83697019872103E-16,-1.));
#18181=DIRECTION('ref_axis',(0.,-1.,1.64970202400831E-16));
#18182=DIRECTION('center_axis',(0.,1.83697019872103E-16,1.));
#18183=DIRECTION('ref_axis',(0.,-1.,1.83697019872103E-16));
#18184=DIRECTION('center_axis',(1.,-1.22464679914735E-16,2.24963967399279E-32));
#18185=DIRECTION('ref_axis',(1.22464679914735E-16,1.,-2.06212753001039E-16));
#18186=DIRECTION('center_axis',(0.,-1.83697019872103E-16,-1.));
#18187=DIRECTION('ref_axis',(0.,-1.,1.83697019872103E-16));
#18188=DIRECTION('center_axis',(0.,-1.83697019872103E-16,-1.));
#18189=DIRECTION('ref_axis',(0.,-1.,1.62614292875575E-16));
#18190=DIRECTION('center_axis',(0.,1.83697019872103E-16,1.));
#18191=DIRECTION('ref_axis',(0.,-1.,1.83697019872103E-16));
#18192=DIRECTION('center_axis',(1.,-1.22464679914735E-16,2.24963967399279E-32));
#18193=DIRECTION('ref_axis',(1.22464679914735E-16,1.,-2.03267866094469E-16));
#18194=DIRECTION('center_axis',(0.,-1.83697019872103E-16,-1.));
#18195=DIRECTION('ref_axis',(0.,-1.,1.83697019872103E-16));
#18196=DIRECTION('center_axis',(0.,1.83697019872103E-16,1.));
#18197=DIRECTION('ref_axis',(0.,1.,-1.64970202400831E-16));
#18198=DIRECTION('center_axis',(0.,-1.83697019872103E-16,-1.));
#18199=DIRECTION('ref_axis',(0.,1.,-1.83697019872103E-16));
#18200=DIRECTION('center_axis',(1.,1.22464679914735E-16,-2.24963967399279E-32));
#18201=DIRECTION('ref_axis',(1.22464679914735E-16,-1.,2.06212753001039E-16));
#18202=DIRECTION('center_axis',(0.,1.83697019872103E-16,1.));
#18203=DIRECTION('ref_axis',(0.,1.,-1.83697019872103E-16));
#18204=DIRECTION('center_axis',(0.,-1.83697019872103E-16,-1.));
#18205=DIRECTION('ref_axis',(0.,1.,-1.83697019872103E-16));
#18206=DIRECTION('center_axis',(0.,1.83697019872103E-16,1.));
#18207=DIRECTION('ref_axis',(0.,-1.,1.83697019872103E-16));
#18208=DIRECTION('center_axis',(0.,1.83697019872103E-16,1.));
#18209=DIRECTION('ref_axis',(0.,-1.,1.83697019872103E-16));
#18210=DIRECTION('',(0.,1.83697019872103E-16,1.));
#18211=DIRECTION('center_axis',(0.,1.83697019872103E-16,1.));
#18212=DIRECTION('ref_axis',(0.,-1.,1.83697019872103E-16));
#18213=DIRECTION('center_axis',(0.,1.83697019872103E-16,1.));
#18214=DIRECTION('ref_axis',(0.,-1.,1.83697019872103E-16));
#18215=DIRECTION('',(0.,1.83697019872103E-16,1.));
#18216=DIRECTION('center_axis',(0.,1.83697019872103E-16,1.));
#18217=DIRECTION('ref_axis',(0.,-1.,1.83697019872103E-16));
#18218=DIRECTION('center_axis',(0.,1.83697019872103E-16,1.));
#18219=DIRECTION('ref_axis',(0.,-1.,1.83697019872103E-16));
#18220=DIRECTION('center_axis',(0.,1.83697019872103E-16,1.));
#18221=DIRECTION('ref_axis',(0.,-1.,1.83697019872103E-16));
#18222=DIRECTION('',(0.,1.83697019872103E-16,1.));
#18223=DIRECTION('center_axis',(0.,-1.83697019872103E-16,-1.));
#18224=DIRECTION('ref_axis',(0.,-1.,1.83697019872103E-16));
#18225=DIRECTION('center_axis',(-1.,1.22464679914735E-16,-2.24963967399279E-32));
#18226=DIRECTION('ref_axis',(1.22464679914735E-16,1.,-1.83697019872103E-16));
#18227=DIRECTION('center_axis',(0.,1.83697019872103E-16,1.));
#18228=DIRECTION('ref_axis',(0.,-1.,1.83697019872103E-16));
#18229=DIRECTION('center_axis',(0.,1.83697019872103E-16,1.));
#18230=DIRECTION('ref_axis',(0.,-1.,1.83697019872103E-16));
#18231=DIRECTION('',(0.,1.83697019872103E-16,1.));
#18232=DIRECTION('center_axis',(0.,1.83697019872103E-16,1.));
#18233=DIRECTION('ref_axis',(0.,-1.,1.83697019872103E-16));
#18234=DIRECTION('center_axis',(0.,1.83697019872103E-16,1.));
#18235=DIRECTION('ref_axis',(0.,-1.,1.83697019872103E-16));
#18236=DIRECTION('',(0.,1.83697019872103E-16,1.));
#18237=DIRECTION('center_axis',(0.,1.83697019872103E-16,1.));
#18238=DIRECTION('ref_axis',(0.,-1.,1.83697019872103E-16));
#18239=DIRECTION('center_axis',(0.,1.83697019872103E-16,1.));
#18240=DIRECTION('ref_axis',(0.,-1.,1.83697019872103E-16));
#18241=DIRECTION('',(0.,1.83697019872103E-16,1.));
#18242=DIRECTION('center_axis',(0.,1.83697019872103E-16,1.));
#18243=DIRECTION('ref_axis',(0.,-1.,1.83697019872103E-16));
#18244=DIRECTION('center_axis',(0.,-1.83697019872103E-16,-1.));
#18245=DIRECTION('ref_axis',(0.,-1.,1.83697019872103E-16));
#18246=DIRECTION('center_axis',(0.,1.83697019872103E-16,1.));
#18247=DIRECTION('ref_axis',(0.,-1.,1.83697019872103E-16));
#18248=DIRECTION('',(-8.65956056235488E-17,-0.707106781186543,0.707106781186552));
#18249=DIRECTION('center_axis',(0.,1.83697019872103E-16,1.));
#18250=DIRECTION('ref_axis',(0.,-1.,1.83697019872103E-16));
#18251=DIRECTION('center_axis',(0.,1.83697019872103E-16,1.));
#18252=DIRECTION('ref_axis',(0.,1.,-1.83697019872103E-16));
#18253=DIRECTION('center_axis',(0.,1.83697019872103E-16,1.));
#18254=DIRECTION('ref_axis',(0.,-1.,1.83697019872103E-16));
#18255=DIRECTION('center_axis',(0.,1.83697019872103E-16,1.));
#18256=DIRECTION('ref_axis',(0.,-1.,1.83697019872103E-16));
#18257=DIRECTION('',(-8.65956056235488E-17,0.707106781186543,-0.707106781186552));
#18258=DIRECTION('center_axis',(0.,1.83697019872103E-16,1.));
#18259=DIRECTION('ref_axis',(0.,-1.,1.83697019872103E-16));
#18260=DIRECTION('center_axis',(0.,1.83697019872103E-16,1.));
#18261=DIRECTION('ref_axis',(0.,-1.,1.83697019872103E-16));
#18262=DIRECTION('',(0.,-1.83697019872103E-16,-1.));
#18263=DIRECTION('center_axis',(0.,-1.83697019872103E-16,-1.));
#18264=DIRECTION('ref_axis',(0.,1.,-1.83697019872103E-16));
#18265=DIRECTION('center_axis',(0.,1.83697019872103E-16,1.));
#18266=DIRECTION('ref_axis',(0.,-1.,1.83697019872103E-16));
#18267=DIRECTION('center_axis',(0.,-1.83697019872103E-16,-1.));
#18268=DIRECTION('ref_axis',(0.,1.,-1.83697019872103E-16));
#18269=DIRECTION('center_axis',(0.,1.83697019872103E-16,1.));
#18270=DIRECTION('ref_axis',(0.,-1.,1.83697019872103E-16));
#18271=DIRECTION('center_axis',(0.,-1.83697019872103E-16,-1.));
#18272=DIRECTION('ref_axis',(0.,1.,-1.83697019872103E-16));
#18273=DIRECTION('center_axis',(0.,1.83697019872103E-16,1.));
#18274=DIRECTION('ref_axis',(0.,-1.,1.83697019872103E-16));
#18275=DIRECTION('center_axis',(-0.781831482468031,0.623489801858732,6.91638013500059E-17));
#18276=DIRECTION('ref_axis',(0.,0.,-1.));
#18277=DIRECTION('center_axis',(0.781831482468031,-0.623489801858732,-6.91638013500059E-17));
#18278=DIRECTION('ref_axis',(-5.40744373425995E-17,4.31229247995119E-17,
-1.));
#18279=DIRECTION('center_axis',(0.623489801858732,0.781831482468031,0.));
#18280=DIRECTION('ref_axis',(0.,0.,1.));
#18281=DIRECTION('center_axis',(0.781831482468031,-0.623489801858732,-6.91638013500059E-17));
#18282=DIRECTION('ref_axis',(-5.40744373425995E-17,4.31229247995119E-17,
-1.));
#18283=DIRECTION('center_axis',(0.623489801858732,0.781831482468031,-1.22464679914735E-16));
#18284=DIRECTION('ref_axis',(0.,0.,-1.));
#18285=DIRECTION('center_axis',(1.79091352057932E-16,2.24573452299036E-16,
1.));
#18286=DIRECTION('ref_axis',(-5.50003967499518E-33,-1.,2.24573452299036E-16));
#18287=DIRECTION('center_axis',(1.79091352057932E-16,2.24573452299036E-16,
1.));
#18288=DIRECTION('ref_axis',(-5.5000396749952E-33,-1.,2.24573452299036E-16));
#18289=DIRECTION('center_axis',(1.79091352057932E-16,2.24573452299036E-16,
1.));
#18290=DIRECTION('ref_axis',(-5.50003967499518E-33,-1.,2.24573452299036E-16));
#18291=DIRECTION('center_axis',(-0.781831482468031,0.623489801858732,0.));
#18292=DIRECTION('ref_axis',(0.,0.,1.));
#18293=DIRECTION('center_axis',(1.43620113371566E-16,6.91638013500059E-17,
1.));
#18294=DIRECTION('ref_axis',(0.623489801858732,0.781831482468031,-1.43620113371566E-16));
#18295=DIRECTION('center_axis',(1.43620113371566E-16,6.91638013500059E-17,
1.));
#18296=DIRECTION('ref_axis',(0.623489801858732,0.781831482468031,-1.43620113371566E-16));
#18297=DIRECTION('center_axis',(1.43620113371566E-16,6.91638013500059E-17,
1.));
#18298=DIRECTION('ref_axis',(0.623489801858732,0.781831482468031,-1.43620113371566E-16));
#18299=DIRECTION('center_axis',(0.781831482468031,-0.623489801858732,-6.91638013500059E-17));
#18300=DIRECTION('ref_axis',(-5.40744373425995E-17,4.31229247995119E-17,
-1.));
#18301=DIRECTION('center_axis',(0.781831482468031,-0.623489801858732,-6.91638013500059E-17));
#18302=DIRECTION('ref_axis',(-5.40744373425995E-17,4.31229247995119E-17,
-1.));
#18303=DIRECTION('center_axis',(-0.974927912181823,-0.222520933956318,2.24573452299036E-16));
#18304=DIRECTION('ref_axis',(0.,-2.10741377257197E-16,-1.));
#18305=DIRECTION('center_axis',(0.974927912181823,0.222520933956318,-2.24573452299036E-16));
#18306=DIRECTION('ref_axis',(-1.71433215598957E-16,-2.58125940401653E-16,
-1.));
#18307=DIRECTION('center_axis',(-0.222520933956318,0.974927912181823,-3.85233095511903E-16));
#18308=DIRECTION('ref_axis',(0.,3.95140082357245E-16,1.));
#18309=DIRECTION('center_axis',(0.974927912181823,0.222520933956318,-2.24573452299036E-16));
#18310=DIRECTION('ref_axis',(-1.71433215598957E-16,-2.58125940401653E-16,
-1.));
#18311=DIRECTION('center_axis',(-0.222520933956318,0.974927912181823,-3.59586625308286E-16));
#18312=DIRECTION('ref_axis',(0.,-2.4905725751517E-16,-1.));
#18313=DIRECTION('center_axis',(7.97031498468594E-17,3.4920231590332E-16,
1.));
#18314=DIRECTION('ref_axis',(2.39882519785021E-33,-1.,3.4920231590332E-16));
#18315=DIRECTION('center_axis',(7.97031498468594E-17,3.4920231590332E-16,
1.));
#18316=DIRECTION('ref_axis',(2.39882519785021E-33,-1.,3.4920231590332E-16));
#18317=DIRECTION('center_axis',(7.97031498468594E-17,3.4920231590332E-16,
1.));
#18318=DIRECTION('ref_axis',(2.39882519785021E-33,-1.,3.4920231590332E-16));
#18319=DIRECTION('center_axis',(-0.974927912181823,-0.222520933956318,6.92755669385935E-17));
#18320=DIRECTION('ref_axis',(0.,3.11321571893962E-16,1.));
#18321=DIRECTION('center_axis',(1.79091352057932E-16,2.24573452299036E-16,
1.));
#18322=DIRECTION('ref_axis',(-0.222520933956318,0.974927912181823,-1.79091352057933E-16));
#18323=DIRECTION('center_axis',(1.79091352057932E-16,2.24573452299036E-16,
1.));
#18324=DIRECTION('ref_axis',(-0.222520933956318,0.974927912181823,-1.79091352057933E-16));
#18325=DIRECTION('center_axis',(1.79091352057932E-16,2.24573452299036E-16,
1.));
#18326=DIRECTION('ref_axis',(-0.222520933956318,0.974927912181823,-1.79091352057933E-16));
#18327=DIRECTION('center_axis',(0.974927912181823,0.222520933956318,-2.24573452299036E-16));
#18328=DIRECTION('ref_axis',(-1.64444757441796E-16,-2.88744376156862E-16,
-1.));
#18329=DIRECTION('center_axis',(0.974927912181823,0.222520933956318,-2.24573452299036E-16));
#18330=DIRECTION('ref_axis',(-1.64444757441796E-16,-2.88744376156862E-16,
-1.));
#18331=DIRECTION('center_axis',(-0.433883739117553,-0.900968867902422,3.4920231590332E-16));
#18332=DIRECTION('ref_axis',(0.,-4.21482754514395E-16,-1.));
#18333=DIRECTION('center_axis',(0.433883739117553,0.900968867902422,-3.4920231590332E-16));
#18334=DIRECTION('ref_axis',(1.97058769816641E-17,-3.97075180104293E-16,
-1.));
#18335=DIRECTION('center_axis',(-0.900968867902422,0.433883739117553,-2.28593141877839E-16));
#18336=DIRECTION('ref_axis',(0.,5.26853443142994E-16,1.));
#18337=DIRECTION('center_axis',(0.433883739117553,0.900968867902422,-3.4920231590332E-16));
#18338=DIRECTION('ref_axis',(1.97058769816641E-17,-3.97075180104293E-16,
-1.));
#18339=DIRECTION('center_axis',(-0.900968867902422,0.433883739117552,-3.33523066916777E-16));
#18340=DIRECTION('ref_axis',(0.,-4.9811451503034E-16,-1.));
#18341=DIRECTION('center_axis',(-7.97031498468617E-17,3.49202315903319E-16,
1.));
#18342=DIRECTION('ref_axis',(-2.39882519785018E-33,-1.,3.49202315903319E-16));
#18343=DIRECTION('center_axis',(-7.97031498468617E-17,3.49202315903319E-16,
1.));
#18344=DIRECTION('ref_axis',(-2.39882519785018E-33,-1.,3.49202315903319E-16));
#18345=DIRECTION('center_axis',(-7.97031498468617E-17,3.49202315903319E-16,
1.));
#18346=DIRECTION('ref_axis',(-2.39882519785018E-33,-1.,3.49202315903319E-16));
#18347=DIRECTION('center_axis',(-0.433883739117552,-0.900968867902422,5.60982088365811E-16));
#18348=DIRECTION('ref_axis',(0.,6.22643143787925E-16,1.));
#18349=DIRECTION('center_axis',(7.97031498468594E-17,3.4920231590332E-16,
1.));
#18350=DIRECTION('ref_axis',(-0.900968867902422,0.433883739117553,-7.97031498468594E-17));
#18351=DIRECTION('center_axis',(7.97031498468594E-17,3.4920231590332E-16,
1.));
#18352=DIRECTION('ref_axis',(-0.900968867902422,0.433883739117553,-7.97031498468594E-17));
#18353=DIRECTION('center_axis',(7.97031498468594E-17,3.4920231590332E-16,
1.));
#18354=DIRECTION('ref_axis',(-0.900968867902422,0.433883739117553,-7.97031498468594E-17));
#18355=DIRECTION('center_axis',(0.433883739117553,0.900968867902422,-3.4920231590332E-16));
#18356=DIRECTION('ref_axis',(4.4891409918625E-17,-4.09203893527874E-16,
-1.));
#18357=DIRECTION('center_axis',(0.433883739117553,0.900968867902422,-3.4920231590332E-16));
#18358=DIRECTION('ref_axis',(4.48914099186251E-17,-4.09203893527874E-16,
-1.));
#18359=DIRECTION('center_axis',(0.433883739117565,-0.900968867902416,3.49202315903319E-16));
#18360=DIRECTION('ref_axis',(0.,-4.21482754514395E-16,-1.));
#18361=DIRECTION('center_axis',(-0.433883739117565,0.900968867902416,-3.49202315903319E-16));
#18362=DIRECTION('ref_axis',(-1.97058769816642E-17,-3.97075180104295E-16,
-1.));
#18363=DIRECTION('center_axis',(-0.900968867902416,-0.433883739117565,2.28593141877845E-16));
#18364=DIRECTION('ref_axis',(0.,5.26853443142994E-16,1.));
#18365=DIRECTION('center_axis',(-0.433883739117565,0.900968867902416,-3.49202315903319E-16));
#18366=DIRECTION('ref_axis',(-1.97058769816642E-17,-3.97075180104295E-16,
-1.));
#18367=DIRECTION('center_axis',(-0.900968867902416,-0.433883739117565,8.85937070873124E-17));
#18368=DIRECTION('ref_axis',(0.,-4.9811451503034E-16,-1.));
#18369=DIRECTION('center_axis',(-1.79091352057933E-16,2.24573452299033E-16,
1.));
#18370=DIRECTION('ref_axis',(5.50003967499563E-33,-1.,2.24573452299033E-16));
#18371=DIRECTION('center_axis',(-1.79091352057933E-16,2.24573452299033E-16,
1.));
#18372=DIRECTION('ref_axis',(5.50003967499563E-33,-1.,2.24573452299033E-16));
#18373=DIRECTION('center_axis',(-1.79091352057933E-16,2.24573452299033E-16,
1.));
#18374=DIRECTION('ref_axis',(5.50003967499563E-33,-1.,2.24573452299033E-16));
#18375=DIRECTION('center_axis',(0.433883739117565,-0.900968867902416,5.60982088365808E-16));
#18376=DIRECTION('ref_axis',(0.,6.22643143787925E-16,1.));
#18377=DIRECTION('center_axis',(-7.97031498468617E-17,3.49202315903319E-16,
1.));
#18378=DIRECTION('ref_axis',(-0.900968867902416,-0.433883739117565,7.97031498468616E-17));
#18379=DIRECTION('center_axis',(-7.97031498468617E-17,3.49202315903319E-16,
1.));
#18380=DIRECTION('ref_axis',(-0.900968867902416,-0.433883739117565,7.97031498468616E-17));
#18381=DIRECTION('center_axis',(-7.97031498468617E-17,3.49202315903319E-16,
1.));
#18382=DIRECTION('ref_axis',(-0.900968867902416,-0.433883739117565,7.97031498468616E-17));
#18383=DIRECTION('center_axis',(-0.433883739117565,0.900968867902416,-3.49202315903319E-16));
#18384=DIRECTION('ref_axis',(-4.48914099186257E-17,-4.09203893527877E-16,
-1.));
#18385=DIRECTION('center_axis',(-0.433883739117565,0.900968867902416,-3.49202315903319E-16));
#18386=DIRECTION('ref_axis',(-4.48914099186258E-17,-4.09203893527877E-16,
-1.));
#18387=DIRECTION('center_axis',(0.974927912181826,-0.222520933956305,2.24573452299033E-16));
#18388=DIRECTION('ref_axis',(0.,-2.10741377257197E-16,-1.));
#18389=DIRECTION('center_axis',(-0.974927912181826,0.222520933956305,-2.24573452299033E-16));
#18390=DIRECTION('ref_axis',(1.71433215598957E-16,-2.58125940401651E-16,
-1.));
#18391=DIRECTION('center_axis',(-0.222520933956305,-0.974927912181826,1.28411031837301E-16));
#18392=DIRECTION('ref_axis',(0.,1.31713360785748E-16,1.));
#18393=DIRECTION('center_axis',(-0.974927912181826,0.222520933956305,-2.24573452299033E-16));
#18394=DIRECTION('ref_axis',(1.71433215598957E-16,-2.58125940401651E-16,
-1.));
#18395=DIRECTION('center_axis',(-0.222520933956305,-0.974927912181826,1.14657265478815E-16));
#18396=DIRECTION('ref_axis',(0.,-1.24528628757585E-16,-1.));
#18397=DIRECTION('center_axis',(-1.43620113371564E-16,6.91638013500039E-17,
1.));
#18398=DIRECTION('ref_axis',(1.,1.10509814492259E-33,1.43620113371564E-16));
#18399=DIRECTION('center_axis',(-1.43620113371564E-16,6.91638013500039E-17,
1.));
#18400=DIRECTION('ref_axis',(1.,1.10509814492259E-33,1.43620113371564E-16));
#18401=DIRECTION('center_axis',(-1.43620113371564E-16,6.91638013500039E-17,
1.));
#18402=DIRECTION('ref_axis',(1.,1.10509814492259E-33,1.43620113371564E-16));
#18403=DIRECTION('center_axis',(0.974927912181826,-0.222520933956305,3.46377834692947E-17));
#18404=DIRECTION('ref_axis',(0.,1.55660785946981E-16,1.));
#18405=DIRECTION('center_axis',(-1.79091352057933E-16,2.24573452299033E-16,
1.));
#18406=DIRECTION('ref_axis',(-0.222520933956305,-0.974927912181826,1.79091352057932E-16));
#18407=DIRECTION('center_axis',(-1.79091352057933E-16,2.24573452299033E-16,
1.));
#18408=DIRECTION('ref_axis',(-0.222520933956305,-0.974927912181826,1.79091352057932E-16));
#18409=DIRECTION('center_axis',(-1.79091352057933E-16,2.24573452299033E-16,
1.));
#18410=DIRECTION('ref_axis',(-0.222520933956305,-0.974927912181826,1.79091352057932E-16));
#18411=DIRECTION('center_axis',(-0.974927912181826,0.222520933956305,-2.24573452299033E-16));
#18412=DIRECTION('ref_axis',(1.64444757441797E-16,-2.8874437615686E-16,
-1.));
#18413=DIRECTION('center_axis',(-0.974927912181826,0.222520933956305,-2.24573452299033E-16));
#18414=DIRECTION('ref_axis',(1.64444757441797E-16,-2.8874437615686E-16,
-1.));
#18415=DIRECTION('center_axis',(0.781831482468022,0.623489801858743,6.91638013500039E-17));
#18416=DIRECTION('ref_axis',(0.,0.,-1.));
#18417=DIRECTION('center_axis',(-0.781831482468022,-0.623489801858743,-6.91638013500039E-17));
#18418=DIRECTION('ref_axis',(5.40744373425973E-17,4.31229247995114E-17,
-1.));
#18419=DIRECTION('center_axis',(0.623489801858743,-0.781831482468022,-2.05955304247934E-16));
#18420=DIRECTION('ref_axis',(0.,-2.63426721571497E-16,1.));
#18421=DIRECTION('center_axis',(-0.781831482468022,-0.623489801858743,-6.91638013500039E-17));
#18422=DIRECTION('ref_axis',(5.40744373425973E-17,4.31229247995114E-17,
-1.));
#18423=DIRECTION('center_axis',(0.623489801858743,-0.781831482468022,-1.22464679914735E-16));
#18424=DIRECTION('ref_axis',(0.,0.,-1.));
#18425=DIRECTION('center_axis',(0.,0.,-1.));
#18426=DIRECTION('ref_axis',(1.,0.,0.));
#18427=DIRECTION('center_axis',(0.781831482468022,0.623489801858743,0.));
#18428=DIRECTION('ref_axis',(0.,0.,1.));
#18429=DIRECTION('center_axis',(-1.43620113371564E-16,6.91638013500039E-17,
1.));
#18430=DIRECTION('ref_axis',(0.623489801858743,-0.781831482468022,1.43620113371564E-16));
#18431=DIRECTION('center_axis',(-1.43620113371564E-16,6.91638013500039E-17,
1.));
#18432=DIRECTION('ref_axis',(0.623489801858743,-0.781831482468022,1.43620113371564E-16));
#18433=DIRECTION('center_axis',(-1.43620113371564E-16,6.91638013500039E-17,
1.));
#18434=DIRECTION('ref_axis',(0.623489801858743,-0.781831482468022,1.43620113371564E-16));
#18435=DIRECTION('center_axis',(0.,0.,-1.));
#18436=DIRECTION('ref_axis',(1.,0.,0.));
#18437=DIRECTION('center_axis',(0.,0.,-1.));
#18438=DIRECTION('ref_axis',(1.,0.,0.));
#18439=DIRECTION('center_axis',(-0.781831482468022,-0.623489801858743,-6.91638013500039E-17));
#18440=DIRECTION('ref_axis',(5.40744373425973E-17,4.31229247995114E-17,
-1.));
#18441=DIRECTION('center_axis',(-0.781831482468022,-0.623489801858743,-6.91638013500039E-17));
#18442=DIRECTION('ref_axis',(5.40744373425973E-17,4.31229247995114E-17,
-1.));
#18443=DIRECTION('center_axis',(1.,0.,-1.22464679914735E-16));
#18444=DIRECTION('ref_axis',(-6.12323399573677E-17,0.,-1.));
#18445=DIRECTION('center_axis',(1.43620113371566E-16,6.91638013500059E-17,
1.));
#18446=DIRECTION('ref_axis',(1.,-1.10509814492274E-33,-1.43620113371566E-16));
#18447=DIRECTION('center_axis',(1.43620113371566E-16,6.91638013500059E-17,
1.));
#18448=DIRECTION('ref_axis',(1.,-1.10509814492274E-33,-1.43620113371566E-16));
#18449=DIRECTION('center_axis',(1.43620113371566E-16,6.91638013500059E-17,
1.));
#18450=DIRECTION('ref_axis',(1.,-1.10509814492274E-33,-1.43620113371566E-16));
#18451=DIRECTION('center_axis',(0.,1.,0.));
#18452=DIRECTION('ref_axis',(6.12323399573677E-17,0.,1.));
#18453=DIRECTION('center_axis',(0.,0.,1.));
#18454=DIRECTION('ref_axis',(1.,0.,0.));
#18455=DIRECTION('center_axis',(0.,0.,1.));
#18456=DIRECTION('ref_axis',(1.,0.,0.));
#18457=DIRECTION('center_axis',(0.,0.,1.));
#18458=DIRECTION('ref_axis',(1.,0.,0.));
#18459=DIRECTION('center_axis',(0.,-1.,0.));
#18460=DIRECTION('ref_axis',(0.,0.,-1.));
#18461=DIRECTION('center_axis',(0.,-1.,0.));
#18462=DIRECTION('ref_axis',(0.,0.,-1.));
#18463=DIRECTION('center_axis',(0.,1.,0.));
#18464=DIRECTION('ref_axis',(0.,0.,-1.));
#18465=DIRECTION('center_axis',(0.,-1.,0.));
#18466=DIRECTION('ref_axis',(0.,0.,-1.));
#18467=DIRECTION('center_axis',(1.,0.,-1.22464679914735E-16));
#18468=DIRECTION('ref_axis',(1.22464679914735E-16,0.,1.));
#18469=DIRECTION('center_axis',(0.,-1.,0.));
#18470=DIRECTION('ref_axis',(0.,0.,-1.));
#18471=DIRECTION('center_axis',(0.,0.,-1.));
#18472=DIRECTION('ref_axis',(-1.,0.,0.));
#18473=DIRECTION('center_axis',(0.,0.,-1.));
#18474=DIRECTION('ref_axis',(1.,0.,0.));
#18475=DIRECTION('center_axis',(0.,0.,-1.));
#18476=DIRECTION('ref_axis',(1.,0.,0.));
#18477=DIRECTION('center_axis',(0.,0.,-1.));
#18478=DIRECTION('ref_axis',(-1.,0.,0.));
#18479=DIRECTION('center_axis',(0.,0.,1.));
#18480=DIRECTION('ref_axis',(1.,0.,0.));
#18481=DIRECTION('center_axis',(0.,0.,1.));
#18482=DIRECTION('ref_axis',(1.,0.,0.));
#18483=DIRECTION('center_axis',(0.,0.,1.));
#18484=DIRECTION('ref_axis',(1.,0.,0.));
#18485=DIRECTION('center_axis',(0.,0.,1.));
#18486=DIRECTION('ref_axis',(1.,0.,0.));
#18487=DIRECTION('center_axis',(0.,-1.,0.));
#18488=DIRECTION('ref_axis',(0.,0.,-1.));
#18489=DIRECTION('center_axis',(0.,1.,0.));
#18490=DIRECTION('ref_axis',(0.,0.,1.));
#18491=DIRECTION('center_axis',(0.,0.,1.));
#18492=DIRECTION('ref_axis',(1.,0.,0.));
#18493=DIRECTION('center_axis',(0.,0.,-1.));
#18494=DIRECTION('ref_axis',(1.,0.,0.));
#18495=DIRECTION('center_axis',(0.,0.,1.));
#18496=DIRECTION('ref_axis',(1.,0.,0.));
#18497=DIRECTION('center_axis',(0.,0.,1.));
#18498=DIRECTION('ref_axis',(1.,0.,0.));
#18499=DIRECTION('center_axis',(0.,0.,1.));
#18500=DIRECTION('ref_axis',(1.,0.,0.));
#18501=DIRECTION('center_axis',(0.,0.,-1.));
#18502=DIRECTION('ref_axis',(1.,0.,0.));
#18503=DIRECTION('center_axis',(0.,0.,-1.));
#18504=DIRECTION('ref_axis',(-1.,0.,0.));
#18505=DIRECTION('center_axis',(0.,0.,-1.));
#18506=DIRECTION('ref_axis',(-1.,0.,0.));
#18507=DIRECTION('center_axis',(0.781831482468022,0.623489801858743,6.91638013500039E-17));
#18508=DIRECTION('ref_axis',(-1.43620113371564E-16,6.91638013500039E-17,
1.));
#18509=DIRECTION('center_axis',(-0.781831482468022,-0.623489801858743,-6.91638013500039E-17));
#18510=DIRECTION('ref_axis',(1.43620113371564E-16,-6.91638013500039E-17,
-1.));
#18511=DIRECTION('center_axis',(-1.43620113371564E-16,6.91638013500039E-17,
1.));
#18512=DIRECTION('ref_axis',(0.623489801858743,-0.781831482468022,1.43620113371564E-16));
#18513=DIRECTION('center_axis',(-1.43620113371564E-16,6.91638013500039E-17,
1.));
#18514=DIRECTION('ref_axis',(0.623489801858743,-0.781831482468022,1.43620113371564E-16));
#18515=DIRECTION('center_axis',(1.43620113371564E-16,-6.91638013500039E-17,
-1.));
#18516=DIRECTION('ref_axis',(0.623489801858743,-0.781831482468022,1.43620113371564E-16));
#18517=DIRECTION('center_axis',(-1.43620113371564E-16,6.91638013500039E-17,
1.));
#18518=DIRECTION('ref_axis',(0.623489801858743,-0.781831482468022,1.43620113371564E-16));
#18519=DIRECTION('center_axis',(1.43620113371564E-16,-6.91638013500039E-17,
-1.));
#18520=DIRECTION('ref_axis',(0.623489801858743,-0.781831482468022,1.43620113371564E-16));
#18521=DIRECTION('center_axis',(-1.43620113371564E-16,6.91638013500039E-17,
1.));
#18522=DIRECTION('ref_axis',(0.623489801858743,-0.781831482468022,1.43620113371564E-16));
#18523=DIRECTION('center_axis',(1.43620113371564E-16,-6.91638013500039E-17,
-1.));
#18524=DIRECTION('ref_axis',(-0.623489801858743,0.781831482468022,-1.43620113371564E-16));
#18525=DIRECTION('center_axis',(1.43620113371564E-16,-6.91638013500039E-17,
-1.));
#18526=DIRECTION('ref_axis',(-0.623489801858743,0.781831482468022,-1.43620113371564E-16));
#18527=DIRECTION('center_axis',(1.79091352057933E-16,-2.24573452299033E-16,
-1.));
#18528=DIRECTION('ref_axis',(0.222520933956305,0.974927912181826,-1.79091352057932E-16));
#18529=DIRECTION('center_axis',(1.79091352057933E-16,-2.24573452299033E-16,
-1.));
#18530=DIRECTION('ref_axis',(-0.222520933956305,-0.974927912181826,1.79091352057932E-16));
#18531=DIRECTION('center_axis',(1.79091352057933E-16,-2.24573452299033E-16,
-1.));
#18532=DIRECTION('ref_axis',(-0.222520933956305,-0.974927912181826,1.79091352057932E-16));
#18533=DIRECTION('center_axis',(1.79091352057933E-16,-2.24573452299033E-16,
-1.));
#18534=DIRECTION('ref_axis',(0.222520933956305,0.974927912181826,-1.79091352057932E-16));
#18535=DIRECTION('center_axis',(-1.79091352057933E-16,2.24573452299033E-16,
1.));
#18536=DIRECTION('ref_axis',(-0.222520933956305,-0.974927912181826,1.79091352057932E-16));
#18537=DIRECTION('center_axis',(-1.79091352057933E-16,2.24573452299033E-16,
1.));
#18538=DIRECTION('ref_axis',(-0.222520933956305,-0.974927912181826,1.79091352057932E-16));
#18539=DIRECTION('center_axis',(-1.79091352057933E-16,2.24573452299033E-16,
1.));
#18540=DIRECTION('ref_axis',(-0.222520933956305,-0.974927912181826,1.79091352057932E-16));
#18541=DIRECTION('center_axis',(-1.79091352057933E-16,2.24573452299033E-16,
1.));
#18542=DIRECTION('ref_axis',(-0.222520933956305,-0.974927912181826,1.79091352057932E-16));
#18543=DIRECTION('center_axis',(0.974927912181826,-0.222520933956305,2.24573452299033E-16));
#18544=DIRECTION('ref_axis',(-1.79091352057933E-16,2.24573452299033E-16,
1.));
#18545=DIRECTION('center_axis',(-0.974927912181826,0.222520933956305,-2.24573452299033E-16));
#18546=DIRECTION('ref_axis',(1.79091352057933E-16,-2.24573452299033E-16,
-1.));
#18547=DIRECTION('center_axis',(-1.79091352057933E-16,2.24573452299033E-16,
1.));
#18548=DIRECTION('ref_axis',(-0.222520933956305,-0.974927912181826,1.79091352057932E-16));
#18549=DIRECTION('center_axis',(-1.79091352057933E-16,2.24573452299033E-16,
1.));
#18550=DIRECTION('ref_axis',(-0.222520933956305,-0.974927912181826,1.79091352057932E-16));
#18551=DIRECTION('center_axis',(1.79091352057933E-16,-2.24573452299033E-16,
-1.));
#18552=DIRECTION('ref_axis',(-0.222520933956305,-0.974927912181826,1.79091352057932E-16));
#18553=DIRECTION('center_axis',(-1.79091352057933E-16,2.24573452299033E-16,
1.));
#18554=DIRECTION('ref_axis',(-0.222520933956305,-0.974927912181826,1.79091352057932E-16));
#18555=DIRECTION('center_axis',(1.79091352057933E-16,-2.24573452299033E-16,
-1.));
#18556=DIRECTION('ref_axis',(-0.222520933956305,-0.974927912181826,1.79091352057932E-16));
#18557=DIRECTION('center_axis',(-1.79091352057933E-16,2.24573452299033E-16,
1.));
#18558=DIRECTION('ref_axis',(-0.222520933956305,-0.974927912181826,1.79091352057932E-16));
#18559=DIRECTION('center_axis',(1.79091352057933E-16,-2.24573452299033E-16,
-1.));
#18560=DIRECTION('ref_axis',(0.222520933956305,0.974927912181826,-1.79091352057932E-16));
#18561=DIRECTION('center_axis',(1.79091352057933E-16,-2.24573452299033E-16,
-1.));
#18562=DIRECTION('ref_axis',(0.222520933956305,0.974927912181826,-1.79091352057932E-16));
#18563=DIRECTION('center_axis',(7.97031498468617E-17,-3.49202315903319E-16,
-1.));
#18564=DIRECTION('ref_axis',(0.900968867902416,0.433883739117565,-7.97031498468616E-17));
#18565=DIRECTION('center_axis',(7.97031498468617E-17,-3.49202315903319E-16,
-1.));
#18566=DIRECTION('ref_axis',(-0.900968867902416,-0.433883739117565,7.97031498468616E-17));
#18567=DIRECTION('center_axis',(7.97031498468617E-17,-3.49202315903319E-16,
-1.));
#18568=DIRECTION('ref_axis',(-0.900968867902416,-0.433883739117565,7.97031498468616E-17));
#18569=DIRECTION('center_axis',(7.97031498468617E-17,-3.49202315903319E-16,
-1.));
#18570=DIRECTION('ref_axis',(0.900968867902416,0.433883739117565,-7.97031498468616E-17));
#18571=DIRECTION('center_axis',(-7.97031498468617E-17,3.49202315903319E-16,
1.));
#18572=DIRECTION('ref_axis',(-0.900968867902416,-0.433883739117565,7.97031498468616E-17));
#18573=DIRECTION('center_axis',(-7.97031498468617E-17,3.49202315903319E-16,
1.));
#18574=DIRECTION('ref_axis',(-0.900968867902416,-0.433883739117565,7.97031498468616E-17));
#18575=DIRECTION('center_axis',(-7.97031498468617E-17,3.49202315903319E-16,
1.));
#18576=DIRECTION('ref_axis',(-0.900968867902416,-0.433883739117565,7.97031498468616E-17));
#18577=DIRECTION('center_axis',(-7.97031498468617E-17,3.49202315903319E-16,
1.));
#18578=DIRECTION('ref_axis',(-0.900968867902416,-0.433883739117565,7.97031498468616E-17));
#18579=DIRECTION('center_axis',(0.433883739117565,-0.900968867902416,3.49202315903319E-16));
#18580=DIRECTION('ref_axis',(-7.97031498468617E-17,3.49202315903319E-16,
1.));
#18581=DIRECTION('center_axis',(-0.433883739117565,0.900968867902416,-3.49202315903319E-16));
#18582=DIRECTION('ref_axis',(7.97031498468617E-17,-3.49202315903319E-16,
-1.));
#18583=DIRECTION('center_axis',(-7.97031498468617E-17,3.49202315903319E-16,
1.));
#18584=DIRECTION('ref_axis',(-0.900968867902416,-0.433883739117565,7.97031498468616E-17));
#18585=DIRECTION('center_axis',(-7.97031498468617E-17,3.49202315903319E-16,
1.));
#18586=DIRECTION('ref_axis',(-0.900968867902416,-0.433883739117565,7.97031498468616E-17));
#18587=DIRECTION('center_axis',(7.97031498468617E-17,-3.49202315903319E-16,
-1.));
#18588=DIRECTION('ref_axis',(-0.900968867902416,-0.433883739117565,7.97031498468616E-17));
#18589=DIRECTION('center_axis',(-7.97031498468617E-17,3.49202315903319E-16,
1.));
#18590=DIRECTION('ref_axis',(-0.900968867902416,-0.433883739117565,7.97031498468616E-17));
#18591=DIRECTION('center_axis',(7.97031498468617E-17,-3.49202315903319E-16,
-1.));
#18592=DIRECTION('ref_axis',(-0.900968867902416,-0.433883739117565,7.97031498468616E-17));
#18593=DIRECTION('center_axis',(-7.97031498468617E-17,3.49202315903319E-16,
1.));
#18594=DIRECTION('ref_axis',(-0.900968867902416,-0.433883739117565,7.97031498468616E-17));
#18595=DIRECTION('center_axis',(7.97031498468617E-17,-3.49202315903319E-16,
-1.));
#18596=DIRECTION('ref_axis',(0.900968867902416,0.433883739117565,-7.97031498468616E-17));
#18597=DIRECTION('center_axis',(7.97031498468617E-17,-3.49202315903319E-16,
-1.));
#18598=DIRECTION('ref_axis',(0.900968867902416,0.433883739117565,-7.97031498468616E-17));
#18599=DIRECTION('center_axis',(-7.97031498468594E-17,-3.4920231590332E-16,
-1.));
#18600=DIRECTION('ref_axis',(0.900968867902422,-0.433883739117553,7.97031498468594E-17));
#18601=DIRECTION('center_axis',(-7.97031498468594E-17,-3.4920231590332E-16,
-1.));
#18602=DIRECTION('ref_axis',(-0.900968867902422,0.433883739117553,-7.97031498468594E-17));
#18603=DIRECTION('center_axis',(-7.97031498468594E-17,-3.4920231590332E-16,
-1.));
#18604=DIRECTION('ref_axis',(-0.900968867902422,0.433883739117553,-7.97031498468594E-17));
#18605=DIRECTION('center_axis',(-7.97031498468594E-17,-3.4920231590332E-16,
-1.));
#18606=DIRECTION('ref_axis',(0.900968867902422,-0.433883739117553,7.97031498468594E-17));
#18607=DIRECTION('center_axis',(7.97031498468594E-17,3.4920231590332E-16,
1.));
#18608=DIRECTION('ref_axis',(-0.900968867902422,0.433883739117553,-7.97031498468594E-17));
#18609=DIRECTION('center_axis',(7.97031498468594E-17,3.4920231590332E-16,
1.));
#18610=DIRECTION('ref_axis',(-0.900968867902422,0.433883739117553,-7.97031498468594E-17));
#18611=DIRECTION('center_axis',(7.97031498468594E-17,3.4920231590332E-16,
1.));
#18612=DIRECTION('ref_axis',(-0.900968867902422,0.433883739117553,-7.97031498468594E-17));
#18613=DIRECTION('center_axis',(7.97031498468594E-17,3.4920231590332E-16,
1.));
#18614=DIRECTION('ref_axis',(-0.900968867902422,0.433883739117553,-7.97031498468594E-17));
#18615=DIRECTION('center_axis',(-0.433883739117553,-0.900968867902422,3.4920231590332E-16));
#18616=DIRECTION('ref_axis',(7.97031498468594E-17,3.4920231590332E-16,1.));
#18617=DIRECTION('center_axis',(0.433883739117553,0.900968867902422,-3.4920231590332E-16));
#18618=DIRECTION('ref_axis',(-7.97031498468594E-17,-3.4920231590332E-16,
-1.));
#18619=DIRECTION('center_axis',(7.97031498468594E-17,3.4920231590332E-16,
1.));
#18620=DIRECTION('ref_axis',(-0.900968867902422,0.433883739117553,-7.97031498468594E-17));
#18621=DIRECTION('center_axis',(7.97031498468594E-17,3.4920231590332E-16,
1.));
#18622=DIRECTION('ref_axis',(-0.900968867902422,0.433883739117553,-7.97031498468594E-17));
#18623=DIRECTION('center_axis',(-7.97031498468594E-17,-3.4920231590332E-16,
-1.));
#18624=DIRECTION('ref_axis',(-0.900968867902422,0.433883739117553,-7.97031498468594E-17));
#18625=DIRECTION('center_axis',(7.97031498468594E-17,3.4920231590332E-16,
1.));
#18626=DIRECTION('ref_axis',(-0.900968867902422,0.433883739117553,-7.97031498468594E-17));
#18627=DIRECTION('center_axis',(-7.97031498468594E-17,-3.4920231590332E-16,
-1.));
#18628=DIRECTION('ref_axis',(-0.900968867902422,0.433883739117553,-7.97031498468594E-17));
#18629=DIRECTION('center_axis',(7.97031498468594E-17,3.4920231590332E-16,
1.));
#18630=DIRECTION('ref_axis',(-0.900968867902422,0.433883739117553,-7.97031498468594E-17));
#18631=DIRECTION('center_axis',(-7.97031498468594E-17,-3.4920231590332E-16,
-1.));
#18632=DIRECTION('ref_axis',(0.900968867902422,-0.433883739117553,7.97031498468594E-17));
#18633=DIRECTION('center_axis',(-7.97031498468594E-17,-3.4920231590332E-16,
-1.));
#18634=DIRECTION('ref_axis',(0.900968867902422,-0.433883739117553,7.97031498468594E-17));
#18635=DIRECTION('center_axis',(-1.79091352057932E-16,-2.24573452299036E-16,
-1.));
#18636=DIRECTION('ref_axis',(0.222520933956318,-0.974927912181823,1.79091352057933E-16));
#18637=DIRECTION('center_axis',(-1.79091352057932E-16,-2.24573452299036E-16,
-1.));
#18638=DIRECTION('ref_axis',(-0.222520933956318,0.974927912181823,-1.79091352057933E-16));
#18639=DIRECTION('center_axis',(-1.79091352057932E-16,-2.24573452299036E-16,
-1.));
#18640=DIRECTION('ref_axis',(-0.222520933956318,0.974927912181823,-1.79091352057933E-16));
#18641=DIRECTION('center_axis',(-1.79091352057932E-16,-2.24573452299036E-16,
-1.));
#18642=DIRECTION('ref_axis',(0.222520933956318,-0.974927912181823,1.79091352057933E-16));
#18643=DIRECTION('center_axis',(1.79091352057932E-16,2.24573452299036E-16,
1.));
#18644=DIRECTION('ref_axis',(-0.222520933956318,0.974927912181823,-1.79091352057933E-16));
#18645=DIRECTION('center_axis',(1.79091352057932E-16,2.24573452299036E-16,
1.));
#18646=DIRECTION('ref_axis',(-0.222520933956318,0.974927912181823,-1.79091352057933E-16));
#18647=DIRECTION('center_axis',(1.79091352057932E-16,2.24573452299036E-16,
1.));
#18648=DIRECTION('ref_axis',(-0.222520933956318,0.974927912181823,-1.79091352057933E-16));
#18649=DIRECTION('center_axis',(1.79091352057932E-16,2.24573452299036E-16,
1.));
#18650=DIRECTION('ref_axis',(-0.222520933956318,0.974927912181823,-1.79091352057933E-16));
#18651=DIRECTION('center_axis',(-0.974927912181823,-0.222520933956318,2.24573452299036E-16));
#18652=DIRECTION('ref_axis',(1.79091352057932E-16,2.24573452299036E-16,
1.));
#18653=DIRECTION('center_axis',(0.974927912181823,0.222520933956318,-2.24573452299036E-16));
#18654=DIRECTION('ref_axis',(-1.79091352057932E-16,-2.24573452299036E-16,
-1.));
#18655=DIRECTION('center_axis',(1.79091352057932E-16,2.24573452299036E-16,
1.));
#18656=DIRECTION('ref_axis',(-0.222520933956318,0.974927912181823,-1.79091352057933E-16));
#18657=DIRECTION('center_axis',(1.79091352057932E-16,2.24573452299036E-16,
1.));
#18658=DIRECTION('ref_axis',(-0.222520933956318,0.974927912181823,-1.79091352057933E-16));
#18659=DIRECTION('center_axis',(-1.79091352057932E-16,-2.24573452299036E-16,
-1.));
#18660=DIRECTION('ref_axis',(-0.222520933956318,0.974927912181823,-1.79091352057933E-16));
#18661=DIRECTION('center_axis',(1.79091352057932E-16,2.24573452299036E-16,
1.));
#18662=DIRECTION('ref_axis',(-0.222520933956318,0.974927912181823,-1.79091352057933E-16));
#18663=DIRECTION('center_axis',(-1.79091352057932E-16,-2.24573452299036E-16,
-1.));
#18664=DIRECTION('ref_axis',(-0.222520933956318,0.974927912181823,-1.79091352057933E-16));
#18665=DIRECTION('center_axis',(1.79091352057932E-16,2.24573452299036E-16,
1.));
#18666=DIRECTION('ref_axis',(-0.222520933956318,0.974927912181823,-1.79091352057933E-16));
#18667=DIRECTION('center_axis',(-1.79091352057932E-16,-2.24573452299036E-16,
-1.));
#18668=DIRECTION('ref_axis',(0.222520933956318,-0.974927912181823,1.79091352057933E-16));
#18669=DIRECTION('center_axis',(-1.79091352057932E-16,-2.24573452299036E-16,
-1.));
#18670=DIRECTION('ref_axis',(0.222520933956318,-0.974927912181823,1.79091352057933E-16));
#18671=DIRECTION('center_axis',(-1.43620113371566E-16,-6.91638013500059E-17,
-1.));
#18672=DIRECTION('ref_axis',(-0.623489801858732,-0.781831482468031,1.43620113371566E-16));
#18673=DIRECTION('center_axis',(-1.43620113371566E-16,-6.91638013500059E-17,
-1.));
#18674=DIRECTION('ref_axis',(0.623489801858732,0.781831482468031,-1.43620113371566E-16));
#18675=DIRECTION('center_axis',(-1.43620113371566E-16,-6.91638013500059E-17,
-1.));
#18676=DIRECTION('ref_axis',(0.623489801858732,0.781831482468031,-1.43620113371566E-16));
#18677=DIRECTION('center_axis',(-1.43620113371566E-16,-6.91638013500059E-17,
-1.));
#18678=DIRECTION('ref_axis',(-0.623489801858732,-0.781831482468031,1.43620113371566E-16));
#18679=DIRECTION('center_axis',(1.43620113371566E-16,6.91638013500059E-17,
1.));
#18680=DIRECTION('ref_axis',(0.623489801858732,0.781831482468031,-1.43620113371566E-16));
#18681=DIRECTION('center_axis',(1.43620113371566E-16,6.91638013500059E-17,
1.));
#18682=DIRECTION('ref_axis',(0.623489801858732,0.781831482468031,-1.43620113371566E-16));
#18683=DIRECTION('center_axis',(1.43620113371566E-16,6.91638013500059E-17,
1.));
#18684=DIRECTION('ref_axis',(0.623489801858732,0.781831482468031,-1.43620113371566E-16));
#18685=DIRECTION('center_axis',(1.43620113371566E-16,6.91638013500059E-17,
1.));
#18686=DIRECTION('ref_axis',(0.623489801858732,0.781831482468031,-1.43620113371566E-16));
#18687=DIRECTION('center_axis',(-0.781831482468031,0.623489801858732,6.91638013500059E-17));
#18688=DIRECTION('ref_axis',(1.43620113371566E-16,6.91638013500061E-17,
1.));
#18689=DIRECTION('center_axis',(0.781831482468031,-0.623489801858732,-6.91638013500059E-17));
#18690=DIRECTION('ref_axis',(-1.43620113371566E-16,-6.91638013500061E-17,
-1.));
#18691=DIRECTION('center_axis',(1.43620113371566E-16,6.91638013500059E-17,
1.));
#18692=DIRECTION('ref_axis',(0.623489801858732,0.781831482468031,-1.43620113371566E-16));
#18693=DIRECTION('center_axis',(1.43620113371566E-16,6.91638013500059E-17,
1.));
#18694=DIRECTION('ref_axis',(0.623489801858732,0.781831482468031,-1.43620113371566E-16));
#18695=DIRECTION('center_axis',(-1.43620113371566E-16,-6.91638013500059E-17,
-1.));
#18696=DIRECTION('ref_axis',(0.623489801858732,0.781831482468031,-1.43620113371566E-16));
#18697=DIRECTION('center_axis',(1.43620113371566E-16,6.91638013500059E-17,
1.));
#18698=DIRECTION('ref_axis',(0.623489801858732,0.781831482468031,-1.43620113371566E-16));
#18699=DIRECTION('center_axis',(-1.43620113371566E-16,-6.91638013500059E-17,
-1.));
#18700=DIRECTION('ref_axis',(0.623489801858732,0.781831482468031,-1.43620113371566E-16));
#18701=DIRECTION('center_axis',(1.43620113371566E-16,6.91638013500059E-17,
1.));
#18702=DIRECTION('ref_axis',(0.623489801858732,0.781831482468031,-1.43620113371566E-16));
#18703=DIRECTION('center_axis',(-1.43620113371566E-16,-6.91638013500059E-17,
-1.));
#18704=DIRECTION('ref_axis',(-0.623489801858732,-0.781831482468031,1.43620113371566E-16));
#18705=DIRECTION('center_axis',(-1.43620113371566E-16,-6.91638013500059E-17,
-1.));
#18706=DIRECTION('ref_axis',(-0.623489801858732,-0.781831482468031,1.43620113371566E-16));
#18707=DIRECTION('center_axis',(0.,0.,1.));
#18708=DIRECTION('ref_axis',(1.,0.,0.));
#18709=DIRECTION('center_axis',(0.,0.,1.));
#18710=DIRECTION('ref_axis',(1.,0.,0.));
#18711=DIRECTION('center_axis',(0.,0.,-1.));
#18712=DIRECTION('ref_axis',(1.,0.,0.));
#18713=DIRECTION('center_axis',(0.,0.,1.));
#18714=DIRECTION('ref_axis',(1.,0.,0.));
#18715=DIRECTION('center_axis',(0.,0.,-1.));
#18716=DIRECTION('ref_axis',(1.,0.,0.));
#18717=DIRECTION('center_axis',(0.,0.,1.));
#18718=DIRECTION('ref_axis',(1.,0.,0.));
#18719=DIRECTION('center_axis',(0.,0.,-1.));
#18720=DIRECTION('ref_axis',(-1.,0.,0.));
#18721=DIRECTION('center_axis',(0.,0.,-1.));
#18722=DIRECTION('ref_axis',(-1.,0.,0.));
#18723=DIRECTION('axis',(0.,0.,1.));
#18724=DIRECTION('refdir',(1.,0.,0.));
#18725=DIRECTION('center_axis',(0.,1.,1.28185868640845E-16));
#18726=DIRECTION('ref_axis',(0.,-1.28185868640845E-16,1.));
#18727=DIRECTION('center_axis',(0.,1.,0.));
#18728=DIRECTION('ref_axis',(0.,0.,1.));
#18729=DIRECTION('',(0.,1.,1.28185868640845E-16));
#18730=DIRECTION('center_axis',(0.,-1.,0.));
#18731=DIRECTION('ref_axis',(1.,0.,0.));
#18732=DIRECTION('center_axis',(0.,1.,0.));
#18733=DIRECTION('ref_axis',(0.,0.,1.));
#18734=DIRECTION('',(-1.,0.,0.));
#18735=DIRECTION('',(0.,0.,-1.));
#18736=DIRECTION('',(1.,0.,0.));
#18737=DIRECTION('',(0.,0.,1.));
#18738=DIRECTION('center_axis',(0.,1.,0.));
#18739=DIRECTION('ref_axis',(-1.57772181044206E-30,0.,1.));
#18740=DIRECTION('center_axis',(-3.15544362088403E-30,1.,-1.31112237000141E-14));
#18741=DIRECTION('ref_axis',(-1.57772181044206E-30,1.31112237000141E-14,
1.));
#18742=DIRECTION('',(-3.15544362088403E-30,1.,-1.31112237000141E-14));
#18743=DIRECTION('center_axis',(0.,-1.,0.));
#18744=DIRECTION('ref_axis',(1.,0.,0.));
#18745=DIRECTION('center_axis',(0.,1.,0.));
#18746=DIRECTION('ref_axis',(0.,0.,1.));
#18747=DIRECTION('',(-1.,0.,0.));
#18748=DIRECTION('',(0.,0.,1.));
#18749=DIRECTION('',(1.,0.,0.));
#18750=DIRECTION('',(0.,0.,-1.));
#18751=DIRECTION('center_axis',(-1.,0.,0.));
#18752=DIRECTION('ref_axis',(0.,0.,-1.));
#18753=DIRECTION('',(0.,-1.,0.));
#18754=DIRECTION('',(0.,-1.,0.));
#18755=DIRECTION('center_axis',(0.,0.,1.));
#18756=DIRECTION('ref_axis',(-1.,0.,0.));
#18757=DIRECTION('',(0.,-1.,0.));
#18758=DIRECTION('center_axis',(0.,0.,-1.));
#18759=DIRECTION('ref_axis',(1.,0.,0.));
#18760=DIRECTION('',(0.,-1.,0.));
#18761=DIRECTION('center_axis',(1.,0.,0.));
#18762=DIRECTION('ref_axis',(0.,0.,1.));
#18763=DIRECTION('axis',(0.,0.,1.));
#18764=DIRECTION('refdir',(1.,0.,0.));
#18765=DIRECTION('center_axis',(0.,-1.,0.));
#18766=DIRECTION('ref_axis',(-1.,0.,0.));
#18767=DIRECTION('center_axis',(0.,-1.,0.));
#18768=DIRECTION('ref_axis',(-1.,0.,0.));
#18769=DIRECTION('',(0.,-1.,0.));
#18770=DIRECTION('center_axis',(0.,1.,0.));
#18771=DIRECTION('ref_axis',(-1.,0.,0.));
#18772=DIRECTION('center_axis',(0.,-1.,0.));
#18773=DIRECTION('ref_axis',(-1.,0.,0.));
#18774=DIRECTION('center_axis',(0.,-1.,0.));
#18775=DIRECTION('ref_axis',(-1.,0.,0.));
#18776=DIRECTION('',(0.,-1.,0.));
#18777=DIRECTION('center_axis',(0.,1.,0.));
#18778=DIRECTION('ref_axis',(-1.,0.,0.));
#18779=DIRECTION('center_axis',(0.,1.,0.));
#18780=DIRECTION('ref_axis',(0.,0.,1.));
#18781=DIRECTION('',(-1.,0.,0.));
#18782=DIRECTION('',(0.,0.,-1.));
#18783=DIRECTION('',(1.,0.,0.));
#18784=DIRECTION('',(0.,0.,1.));
#18785=DIRECTION('center_axis',(1.,0.,0.));
#18786=DIRECTION('ref_axis',(0.,0.,-1.));
#18787=DIRECTION('',(0.,1.,0.));
#18788=DIRECTION('',(0.,0.,-1.));
#18789=DIRECTION('',(0.,1.,0.));
#18790=DIRECTION('center_axis',(0.,0.,-1.));
#18791=DIRECTION('ref_axis',(-1.,0.,0.));
#18792=DIRECTION('',(0.,1.,0.));
#18793=DIRECTION('',(-1.,0.,0.));
#18794=DIRECTION('center_axis',(0.,0.,1.));
#18795=DIRECTION('ref_axis',(1.,0.,0.));
#18796=DIRECTION('',(1.,0.,0.));
#18797=DIRECTION('',(0.,1.,0.));
#18798=DIRECTION('center_axis',(-1.,0.,0.));
#18799=DIRECTION('ref_axis',(0.,0.,1.));
#18800=DIRECTION('',(0.,0.,1.));
#18801=DIRECTION('center_axis',(0.,1.,0.));
#18802=DIRECTION('ref_axis',(0.,0.,1.));
#18803=DIRECTION('',(0.,-1.,-2.4980018054066E-16));
#18804=DIRECTION('',(1.,0.,0.));
#18805=DIRECTION('',(0.,-1.,8.74300631892311E-16));
#18806=DIRECTION('',(1.,0.,0.));
#18807=DIRECTION('',(-3.15544362088405E-30,1.,-1.32949207198862E-14));
#18808=DIRECTION('',(1.,3.15544362088407E-30,1.57772181044202E-30));
#18809=DIRECTION('',(0.,1.,-5.55111512312578E-17));
#18810=DIRECTION('',(1.,0.,0.));
#18811=DIRECTION('',(3.15544362088405E-30,1.,1.32949207198862E-14));
#18812=DIRECTION('',(1.,-3.15544362088407E-30,1.57772181044202E-30));
#18813=DIRECTION('',(0.,1.,5.55111512312578E-17));
#18814=DIRECTION('',(1.,0.,0.));
#18815=DIRECTION('',(0.,0.,1.));
#18816=DIRECTION('',(1.,0.,0.));
#18817=DIRECTION('',(0.,0.,1.));
#18818=DIRECTION('',(1.,0.,0.));
#18819=CARTESIAN_POINT('',(0.,0.,0.));
#18820=CARTESIAN_POINT('',(0.,0.,0.));
#18821=CARTESIAN_POINT('Origin',(0.,3.33066907387547E-15,7.50000243576834));
#18822=CARTESIAN_POINT('',(-7.5,4.09394740330526E-15,15.0000024357683));
#18823=CARTESIAN_POINT('Origin',(0.,2.98372437868011E-15,15.0000024357683));
#18824=CARTESIAN_POINT('',(-7.5,1.6739163200269E-14,57.5000024357683));
#18825=CARTESIAN_POINT('',(-7.5,4.24915417323598E-15,7.50000243576834));
#18826=CARTESIAN_POINT('Origin',(0.,1.58206781009085E-14,57.5000024357683));
#18827=CARTESIAN_POINT('Origin',(0.,3.33066907387547E-15,7.50000243576834));
#18828=CARTESIAN_POINT('',(-7.5,-8.49065503433768E-15,-43.4999975642317));
#18829=CARTESIAN_POINT('Origin',(0.,-9.4091401336982E-15,-43.4999975642317));
#18830=CARTESIAN_POINT('',(-7.5,3.46944695195362E-16,2.43576833591774E-6));
#18831=CARTESIAN_POINT('',(-7.5,4.24915417323598E-15,7.50000243576834));
#18832=CARTESIAN_POINT('Origin',(0.,-7.63278329429795E-16,2.43576833591774E-6));
#18833=CARTESIAN_POINT('Origin',(0.,1.69309011255336E-14,57.5000024357683));
#18834=CARTESIAN_POINT('Origin',(0.,-8.29891710907304E-15,-43.4999975642317));
#18835=CARTESIAN_POINT('Origin',(35.6951686664485,-6.98407602147876,0.));
#18836=CARTESIAN_POINT('',(34.7137772481474,-6.79205809501118,15.));
#18837=CARTESIAN_POINT('',(35.4762412689616,-7.95981717292705,15.));
#18838=CARTESIAN_POINT('Origin',(35.6951686664485,-6.98407602147876,15.));
#18839=CARTESIAN_POINT('',(35.4762412689616,-7.95981717292705,0.));
#18840=CARTESIAN_POINT('',(35.4762412689616,-7.95981717292705,0.));
#18841=CARTESIAN_POINT('',(34.7137772481474,-6.79205809501118,0.));
#18842=CARTESIAN_POINT('Origin',(35.6951686664485,-6.98407602147876,0.));
#18843=CARTESIAN_POINT('',(34.7137772481474,-6.79205809501118,0.));
#18844=CARTESIAN_POINT('Origin',(36.6758703925241,-8.22897839625062,0.));
#18845=CARTESIAN_POINT('',(36.6758703925241,-8.22897839625062,15.));
#18846=CARTESIAN_POINT('',(34.5041585975144,-7.74171062993033,15.));
#18847=CARTESIAN_POINT('',(36.6758703925241,-8.22897839625062,0.));
#18848=CARTESIAN_POINT('',(36.6758703925241,-8.22897839625062,0.));
#18849=CARTESIAN_POINT('',(34.5041585975144,-7.74171062993033,0.));
#18850=CARTESIAN_POINT('Origin',(32.9831349545516,-15.3308575288479,0.));
#18851=CARTESIAN_POINT('',(32.0763073136589,-14.909355892181,0.));
#18852=CARTESIAN_POINT('',(33.3795452283267,-14.4127840596497,0.));
#18853=CARTESIAN_POINT('Origin',(32.9831349545516,-15.3308575288479,0.));
#18854=CARTESIAN_POINT('',(33.3795452283267,-14.4127840596497,15.));
#18855=CARTESIAN_POINT('',(33.3795452283267,-14.4127840596497,0.));
#18856=CARTESIAN_POINT('',(32.0763073136589,-14.909355892181,15.));
#18857=CARTESIAN_POINT('Origin',(32.9831349545516,-15.3308575288479,15.));
#18858=CARTESIAN_POINT('',(32.0763073136589,-14.909355892181,0.));
#18859=CARTESIAN_POINT('Origin',(32.4649140177865,-14.0178601012327,0.));
#18860=CARTESIAN_POINT('',(34.5082745737944,-14.9001523628048,0.));
#18861=CARTESIAN_POINT('',(32.4649140177865,-14.0178601012327,0.));
#18862=CARTESIAN_POINT('',(34.5082745737944,-14.9001523628048,15.));
#18863=CARTESIAN_POINT('',(34.5082745737944,-14.9001523628048,0.));
#18864=CARTESIAN_POINT('',(32.4649140177865,-14.0178601012327,15.));
#18865=CARTESIAN_POINT('Origin',(31.7899245798369,-17.6726647455408,0.));
#18866=CARTESIAN_POINT('',(30.9159026789286,-17.1867782189396,15.));
#18867=CARTESIAN_POINT('',(31.280191653953,-18.5329974394853,15.));
#18868=CARTESIAN_POINT('Origin',(31.7899245798369,-17.6726647455408,15.));
#18869=CARTESIAN_POINT('',(31.280191653953,-18.5329974394853,0.));
#18870=CARTESIAN_POINT('',(31.280191653953,-18.5329974394853,0.));
#18871=CARTESIAN_POINT('',(30.9159026789286,-17.1867782189396,0.));
#18872=CARTESIAN_POINT('Origin',(31.7899245798369,-17.6726647455408,0.));
#18873=CARTESIAN_POINT('',(30.9159026789286,-17.1867782189396,0.));
#18874=CARTESIAN_POINT('Origin',(32.3379313568208,-19.1596907609891,0.));
#18875=CARTESIAN_POINT('',(32.3379313568208,-19.1596907609891,15.));
#18876=CARTESIAN_POINT('',(30.4230847232658,-18.0251757251071,15.));
#18877=CARTESIAN_POINT('',(32.3379313568208,-19.1596907609891,0.));
#18878=CARTESIAN_POINT('',(32.3379313568208,-19.1596907609891,0.));
#18879=CARTESIAN_POINT('',(30.4230847232658,-18.0251757251071,0.));
#18880=CARTESIAN_POINT('Origin',(26.6313299116137,-24.7728611819223,0.));
#18881=CARTESIAN_POINT('',(25.899136743473,-24.0917641517363,0.));
#18882=CARTESIAN_POINT('',(27.2920387896808,-24.0222189379449,0.));
#18883=CARTESIAN_POINT('Origin',(26.6313299116137,-24.7728611819223,0.));
#18884=CARTESIAN_POINT('',(27.2920387896808,-24.0222189379449,15.));
#18885=CARTESIAN_POINT('',(27.2920387896808,-24.0222189379449,0.));
#18886=CARTESIAN_POINT('',(25.899136743473,-24.0917641517363,15.));
#18887=CARTESIAN_POINT('Origin',(26.6313299116137,-24.7728611819223,15.));
#18888=CARTESIAN_POINT('',(25.899136743473,-24.0917641517363,0.));
#18889=CARTESIAN_POINT('Origin',(26.5442110315263,-23.3639873462087,0.));
#18890=CARTESIAN_POINT('',(28.2149191006268,-24.8345302882955,0.));
#18891=CARTESIAN_POINT('',(26.5442110315263,-23.3639873462087,0.));
#18892=CARTESIAN_POINT('',(28.2149191006268,-24.8345302882955,15.));
#18893=CARTESIAN_POINT('',(28.2149191006268,-24.8345302882955,0.));
#18894=CARTESIAN_POINT('',(26.5442110315263,-23.3639873462087,15.));
#18895=CARTESIAN_POINT('Origin',(24.7728611819222,-26.6313299116137,0.));
#18896=CARTESIAN_POINT('',(24.0917641517363,-25.899136743473,15.));
#18897=CARTESIAN_POINT('',(24.0222189379449,-27.2920387896808,15.));
#18898=CARTESIAN_POINT('Origin',(24.7728611819222,-26.6313299116137,15.));
#18899=CARTESIAN_POINT('',(24.0222189379449,-27.2920387896808,0.));
#18900=CARTESIAN_POINT('',(24.0222189379449,-27.2920387896808,0.));
#18901=CARTESIAN_POINT('',(24.0917641517363,-25.899136743473,0.));
#18902=CARTESIAN_POINT('Origin',(24.7728611819222,-26.6313299116137,0.));
#18903=CARTESIAN_POINT('',(24.0917641517363,-25.899136743473,0.));
#18904=CARTESIAN_POINT('Origin',(24.8345302882955,-28.2149191006269,0.));
#18905=CARTESIAN_POINT('',(24.8345302882955,-28.2149191006269,15.));
#18906=CARTESIAN_POINT('',(23.3639873462086,-26.5442110315263,15.));
#18907=CARTESIAN_POINT('',(24.8345302882955,-28.2149191006269,0.));
#18908=CARTESIAN_POINT('',(24.8345302882955,-28.2149191006269,0.));
#18909=CARTESIAN_POINT('',(23.3639873462086,-26.5442110315263,0.));
#18910=CARTESIAN_POINT('Origin',(17.6726647455408,-31.7899245798369,0.));
#18911=CARTESIAN_POINT('',(17.1867782189395,-30.9159026789286,0.));
#18912=CARTESIAN_POINT('',(18.5329974394853,-31.280191653953,0.));
#18913=CARTESIAN_POINT('Origin',(17.6726647455408,-31.7899245798369,0.));
#18914=CARTESIAN_POINT('',(18.5329974394853,-31.280191653953,15.));
#18915=CARTESIAN_POINT('',(18.5329974394853,-31.280191653953,0.));
#18916=CARTESIAN_POINT('',(17.1867782189395,-30.9159026789286,15.));
#18917=CARTESIAN_POINT('Origin',(17.6726647455408,-31.7899245798369,15.));
#18918=CARTESIAN_POINT('',(17.1867782189395,-30.9159026789286,0.));
#18919=CARTESIAN_POINT('Origin',(18.0251757251071,-30.4230847232658,0.));
#18920=CARTESIAN_POINT('',(19.1596907609891,-32.3379313568208,0.));
#18921=CARTESIAN_POINT('',(18.0251757251071,-30.4230847232658,0.));
#18922=CARTESIAN_POINT('',(19.1596907609891,-32.3379313568208,15.));
#18923=CARTESIAN_POINT('',(19.1596907609891,-32.3379313568208,0.));
#18924=CARTESIAN_POINT('',(18.0251757251071,-30.4230847232658,15.));
#18925=CARTESIAN_POINT('Origin',(15.3308575288479,-32.9831349545517,0.));
#18926=CARTESIAN_POINT('',(14.909355892181,-32.0763073136589,15.));
#18927=CARTESIAN_POINT('',(14.4127840596497,-33.3795452283267,15.));
#18928=CARTESIAN_POINT('Origin',(15.3308575288479,-32.9831349545517,15.));
#18929=CARTESIAN_POINT('',(14.4127840596497,-33.3795452283267,0.));
#18930=CARTESIAN_POINT('',(14.4127840596497,-33.3795452283267,0.));
#18931=CARTESIAN_POINT('',(14.909355892181,-32.0763073136589,0.));
#18932=CARTESIAN_POINT('Origin',(15.3308575288479,-32.9831349545517,0.));
#18933=CARTESIAN_POINT('',(14.909355892181,-32.0763073136589,0.));
#18934=CARTESIAN_POINT('Origin',(14.9001523628048,-34.5082745737944,0.));
#18935=CARTESIAN_POINT('',(14.9001523628048,-34.5082745737944,15.));
#18936=CARTESIAN_POINT('',(14.0178601012327,-32.4649140177865,15.));
#18937=CARTESIAN_POINT('',(14.9001523628048,-34.5082745737944,0.));
#18938=CARTESIAN_POINT('',(14.9001523628048,-34.5082745737944,0.));
#18939=CARTESIAN_POINT('',(14.0178601012327,-32.4649140177865,0.));
#18940=CARTESIAN_POINT('Origin',(6.98407602147874,-35.6951686664485,0.));
#18941=CARTESIAN_POINT('',(6.79205809501116,-34.7137772481474,0.));
#18942=CARTESIAN_POINT('',(7.95981717292703,-35.4762412689616,0.));
#18943=CARTESIAN_POINT('Origin',(6.98407602147874,-35.6951686664485,0.));
#18944=CARTESIAN_POINT('',(7.95981717292703,-35.4762412689616,15.));
#18945=CARTESIAN_POINT('',(7.95981717292703,-35.4762412689616,0.));
#18946=CARTESIAN_POINT('',(6.79205809501116,-34.7137772481474,15.));
#18947=CARTESIAN_POINT('Origin',(6.98407602147874,-35.6951686664485,15.));
#18948=CARTESIAN_POINT('',(6.79205809501116,-34.7137772481474,0.));
#18949=CARTESIAN_POINT('Origin',(7.74171062993031,-34.5041585975144,0.));
#18950=CARTESIAN_POINT('',(8.2289783962506,-36.6758703925241,0.));
#18951=CARTESIAN_POINT('',(7.74171062993031,-34.5041585975144,0.));
#18952=CARTESIAN_POINT('',(8.2289783962506,-36.6758703925241,15.));
#18953=CARTESIAN_POINT('',(8.2289783962506,-36.6758703925241,0.));
#18954=CARTESIAN_POINT('',(7.74171062993031,-34.5041585975144,15.));
#18955=CARTESIAN_POINT('Origin',(4.3881627244846,-36.1063209411239,0.));
#18956=CARTESIAN_POINT('',(4.2675159983083,-35.1136254352094,15.));
#18957=CARTESIAN_POINT('',(3.39252545782465,-36.199629211057,15.));
#18958=CARTESIAN_POINT('Origin',(4.3881627244846,-36.1063209411239,15.));
#18959=CARTESIAN_POINT('',(3.39252545782465,-36.199629211057,0.));
#18960=CARTESIAN_POINT('',(3.39252545782466,-36.199629211057,0.));
#18961=CARTESIAN_POINT('',(4.2675159983083,-35.1136254352094,0.));
#18962=CARTESIAN_POINT('Origin',(4.3881627244846,-36.1063209411239,0.));
#18963=CARTESIAN_POINT('',(4.2675159983083,-35.1136254352094,0.));
#18964=CARTESIAN_POINT('Origin',(3.50724370857672,-37.4237196983922,0.));
#18965=CARTESIAN_POINT('',(3.50724370857672,-37.4237196983922,15.));
#18966=CARTESIAN_POINT('',(3.29956704137369,-35.2077250236291,15.));
#18967=CARTESIAN_POINT('',(3.50724370857672,-37.4237196983922,0.));
#18968=CARTESIAN_POINT('',(3.50724370857672,-37.4237196983922,0.));
#18969=CARTESIAN_POINT('',(3.29956704137369,-35.2077250236291,0.));
#18970=CARTESIAN_POINT('Origin',(-4.38816272448462,-36.1063209411239,0.));
#18971=CARTESIAN_POINT('',(-4.26751599830832,-35.1136254352094,0.));
#18972=CARTESIAN_POINT('',(-3.39252545782467,-36.199629211057,0.));
#18973=CARTESIAN_POINT('Origin',(-4.38816272448462,-36.1063209411239,0.));
#18974=CARTESIAN_POINT('',(-3.39252545782467,-36.199629211057,15.));
#18975=CARTESIAN_POINT('',(-3.39252545782467,-36.199629211057,0.));
#18976=CARTESIAN_POINT('',(-4.26751599830832,-35.1136254352094,15.));
#18977=CARTESIAN_POINT('Origin',(-4.38816272448462,-36.1063209411239,15.));
#18978=CARTESIAN_POINT('',(-4.26751599830831,-35.1136254352094,0.));
#18979=CARTESIAN_POINT('Origin',(-3.29956704137371,-35.2077250236291,0.));
#18980=CARTESIAN_POINT('',(-3.50724370857673,-37.4237196983922,0.));
#18981=CARTESIAN_POINT('',(-3.29956704137371,-35.2077250236291,0.));
#18982=CARTESIAN_POINT('',(-3.50724370857673,-37.4237196983922,15.));
#18983=CARTESIAN_POINT('',(-3.50724370857673,-37.4237196983922,0.));
#18984=CARTESIAN_POINT('',(-3.29956704137371,-35.2077250236291,15.));
#18985=CARTESIAN_POINT('Origin',(-6.98407602147876,-35.6951686664485,0.));
#18986=CARTESIAN_POINT('',(-6.79205809501118,-34.7137772481474,15.));
#18987=CARTESIAN_POINT('',(-7.95981717292705,-35.4762412689616,15.));
#18988=CARTESIAN_POINT('Origin',(-6.98407602147876,-35.6951686664485,15.));
#18989=CARTESIAN_POINT('',(-7.95981717292705,-35.4762412689616,0.));
#18990=CARTESIAN_POINT('',(-7.95981717292705,-35.4762412689616,0.));
#18991=CARTESIAN_POINT('',(-6.79205809501118,-34.7137772481474,0.));
#18992=CARTESIAN_POINT('Origin',(-6.98407602147876,-35.6951686664485,0.));
#18993=CARTESIAN_POINT('',(-6.79205809501118,-34.7137772481474,0.));
#18994=CARTESIAN_POINT('Origin',(-8.22897839625062,-36.6758703925241,0.));
#18995=CARTESIAN_POINT('',(-8.22897839625062,-36.6758703925241,15.));
#18996=CARTESIAN_POINT('',(-7.74171062993033,-34.5041585975144,15.));
#18997=CARTESIAN_POINT('',(-8.22897839625062,-36.6758703925241,0.));
#18998=CARTESIAN_POINT('',(-8.22897839625062,-36.6758703925241,0.));
#18999=CARTESIAN_POINT('',(-7.74171062993033,-34.5041585975144,0.));
#19000=CARTESIAN_POINT('Origin',(-15.3308575288479,-32.9831349545516,0.));
#19001=CARTESIAN_POINT('',(-14.909355892181,-32.0763073136589,0.));
#19002=CARTESIAN_POINT('',(-14.4127840596497,-33.3795452283267,0.));
#19003=CARTESIAN_POINT('Origin',(-15.3308575288479,-32.9831349545516,0.));
#19004=CARTESIAN_POINT('',(-14.4127840596497,-33.3795452283267,15.));
#19005=CARTESIAN_POINT('',(-14.4127840596497,-33.3795452283267,0.));
#19006=CARTESIAN_POINT('',(-14.909355892181,-32.0763073136589,15.));
#19007=CARTESIAN_POINT('Origin',(-15.3308575288479,-32.9831349545516,15.));
#19008=CARTESIAN_POINT('',(-14.909355892181,-32.0763073136589,0.));
#19009=CARTESIAN_POINT('Origin',(-14.0178601012327,-32.4649140177865,0.));
#19010=CARTESIAN_POINT('',(-14.9001523628048,-34.5082745737944,0.));
#19011=CARTESIAN_POINT('',(-14.0178601012327,-32.4649140177865,0.));
#19012=CARTESIAN_POINT('',(-14.9001523628048,-34.5082745737944,15.));
#19013=CARTESIAN_POINT('',(-14.9001523628048,-34.5082745737944,0.));
#19014=CARTESIAN_POINT('',(-14.0178601012327,-32.4649140177865,15.));
#19015=CARTESIAN_POINT('Origin',(-17.6726647455408,-31.7899245798369,0.));
#19016=CARTESIAN_POINT('',(-17.1867782189396,-30.9159026789286,15.));
#19017=CARTESIAN_POINT('',(-18.5329974394853,-31.280191653953,15.));
#19018=CARTESIAN_POINT('Origin',(-17.6726647455408,-31.7899245798369,15.));
#19019=CARTESIAN_POINT('',(-18.5329974394853,-31.280191653953,0.));
#19020=CARTESIAN_POINT('',(-18.5329974394853,-31.280191653953,0.));
#19021=CARTESIAN_POINT('',(-17.1867782189396,-30.9159026789286,0.));
#19022=CARTESIAN_POINT('Origin',(-17.6726647455408,-31.7899245798369,0.));
#19023=CARTESIAN_POINT('',(-17.1867782189396,-30.9159026789286,0.));
#19024=CARTESIAN_POINT('Origin',(-19.1596907609891,-32.3379313568208,0.));
#19025=CARTESIAN_POINT('',(-19.1596907609891,-32.3379313568208,15.));
#19026=CARTESIAN_POINT('',(-18.0251757251071,-30.4230847232658,15.));
#19027=CARTESIAN_POINT('',(-19.1596907609891,-32.3379313568208,0.));
#19028=CARTESIAN_POINT('',(-19.1596907609891,-32.3379313568208,0.));
#19029=CARTESIAN_POINT('',(-18.0251757251071,-30.4230847232658,0.));
#19030=CARTESIAN_POINT('Origin',(-24.7728611819223,-26.6313299116137,0.));
#19031=CARTESIAN_POINT('',(-24.0917641517363,-25.899136743473,0.));
#19032=CARTESIAN_POINT('',(-24.0222189379449,-27.2920387896808,0.));
#19033=CARTESIAN_POINT('Origin',(-24.7728611819223,-26.6313299116137,0.));
#19034=CARTESIAN_POINT('',(-24.0222189379449,-27.2920387896808,15.));
#19035=CARTESIAN_POINT('',(-24.0222189379449,-27.2920387896808,0.));
#19036=CARTESIAN_POINT('',(-24.0917641517363,-25.899136743473,15.));
#19037=CARTESIAN_POINT('Origin',(-24.7728611819223,-26.6313299116137,15.));
#19038=CARTESIAN_POINT('',(-24.0917641517363,-25.899136743473,0.));
#19039=CARTESIAN_POINT('Origin',(-23.3639873462087,-26.5442110315263,0.));
#19040=CARTESIAN_POINT('',(-24.8345302882955,-28.2149191006268,0.));
#19041=CARTESIAN_POINT('',(-23.3639873462087,-26.5442110315263,0.));
#19042=CARTESIAN_POINT('',(-24.8345302882955,-28.2149191006268,15.));
#19043=CARTESIAN_POINT('',(-24.8345302882955,-28.2149191006268,0.));
#19044=CARTESIAN_POINT('',(-23.3639873462087,-26.5442110315263,15.));
#19045=CARTESIAN_POINT('Origin',(-26.6313299116137,-24.7728611819222,0.));
#19046=CARTESIAN_POINT('',(-25.899136743473,-24.0917641517363,15.));
#19047=CARTESIAN_POINT('',(-27.2920387896808,-24.0222189379449,15.));
#19048=CARTESIAN_POINT('Origin',(-26.6313299116137,-24.7728611819222,15.));
#19049=CARTESIAN_POINT('',(-27.2920387896808,-24.0222189379449,0.));
#19050=CARTESIAN_POINT('',(-27.2920387896808,-24.0222189379449,0.));
#19051=CARTESIAN_POINT('',(-25.899136743473,-24.0917641517363,0.));
#19052=CARTESIAN_POINT('Origin',(-26.6313299116137,-24.7728611819222,0.));
#19053=CARTESIAN_POINT('',(-25.899136743473,-24.0917641517363,0.));
#19054=CARTESIAN_POINT('Origin',(-28.2149191006269,-24.8345302882955,0.));
#19055=CARTESIAN_POINT('',(-28.2149191006269,-24.8345302882955,15.));
#19056=CARTESIAN_POINT('',(-26.5442110315263,-23.3639873462087,15.));
#19057=CARTESIAN_POINT('',(-28.2149191006269,-24.8345302882955,0.));
#19058=CARTESIAN_POINT('',(-28.2149191006269,-24.8345302882955,0.));
#19059=CARTESIAN_POINT('',(-26.5442110315263,-23.3639873462087,0.));
#19060=CARTESIAN_POINT('Origin',(-31.7899245798369,-17.6726647455408,0.));
#19061=CARTESIAN_POINT('',(-30.9159026789286,-17.1867782189396,0.));
#19062=CARTESIAN_POINT('',(-31.280191653953,-18.5329974394853,0.));
#19063=CARTESIAN_POINT('Origin',(-31.7899245798369,-17.6726647455408,0.));
#19064=CARTESIAN_POINT('',(-31.280191653953,-18.5329974394853,15.));
#19065=CARTESIAN_POINT('',(-31.280191653953,-18.5329974394853,0.));
#19066=CARTESIAN_POINT('',(-30.9159026789286,-17.1867782189396,15.));
#19067=CARTESIAN_POINT('Origin',(-31.7899245798369,-17.6726647455408,15.));
#19068=CARTESIAN_POINT('',(-30.9159026789286,-17.1867782189396,0.));
#19069=CARTESIAN_POINT('Origin',(-30.4230847232658,-18.0251757251071,0.));
#19070=CARTESIAN_POINT('',(-32.3379313568208,-19.1596907609891,0.));
#19071=CARTESIAN_POINT('',(-30.4230847232658,-18.0251757251071,0.));
#19072=CARTESIAN_POINT('',(-32.3379313568208,-19.1596907609891,15.));
#19073=CARTESIAN_POINT('',(-32.3379313568208,-19.1596907609891,0.));
#19074=CARTESIAN_POINT('',(-30.4230847232658,-18.0251757251071,15.));
#19075=CARTESIAN_POINT('Origin',(-32.9831349545517,-15.3308575288479,0.));
#19076=CARTESIAN_POINT('',(-32.0763073136589,-14.909355892181,15.));
#19077=CARTESIAN_POINT('',(-33.3795452283267,-14.4127840596497,15.));
#19078=CARTESIAN_POINT('Origin',(-32.9831349545517,-15.3308575288479,15.));
#19079=CARTESIAN_POINT('',(-33.3795452283267,-14.4127840596497,0.));
#19080=CARTESIAN_POINT('',(-33.3795452283267,-14.4127840596497,0.));
#19081=CARTESIAN_POINT('',(-32.0763073136589,-14.909355892181,0.));
#19082=CARTESIAN_POINT('Origin',(-32.9831349545517,-15.3308575288479,0.));
#19083=CARTESIAN_POINT('',(-32.0763073136589,-14.909355892181,0.));
#19084=CARTESIAN_POINT('Origin',(-34.5082745737944,-14.9001523628048,0.));
#19085=CARTESIAN_POINT('',(-34.5082745737944,-14.9001523628048,15.));
#19086=CARTESIAN_POINT('',(-32.4649140177865,-14.0178601012327,15.));
#19087=CARTESIAN_POINT('',(-34.5082745737944,-14.9001523628048,0.));
#19088=CARTESIAN_POINT('',(-34.5082745737944,-14.9001523628048,0.));
#19089=CARTESIAN_POINT('',(-32.4649140177865,-14.0178601012327,0.));
#19090=CARTESIAN_POINT('Origin',(-35.6951686664485,-6.98407602147875,0.));
#19091=CARTESIAN_POINT('',(-34.7137772481474,-6.79205809501117,0.));
#19092=CARTESIAN_POINT('',(-35.4762412689616,-7.95981717292703,0.));
#19093=CARTESIAN_POINT('Origin',(-35.6951686664485,-6.98407602147875,0.));
#19094=CARTESIAN_POINT('',(-35.4762412689616,-7.95981717292703,15.));
#19095=CARTESIAN_POINT('',(-35.4762412689616,-7.95981717292703,0.));
#19096=CARTESIAN_POINT('',(-34.7137772481474,-6.79205809501117,15.));
#19097=CARTESIAN_POINT('Origin',(-35.6951686664485,-6.98407602147875,15.));
#19098=CARTESIAN_POINT('',(-34.7137772481474,-6.79205809501117,0.));
#19099=CARTESIAN_POINT('Origin',(-34.5041585975144,-7.74171062993032,0.));
#19100=CARTESIAN_POINT('',(-36.6758703925241,-8.2289783962506,0.));
#19101=CARTESIAN_POINT('',(-34.5041585975144,-7.74171062993032,0.));
#19102=CARTESIAN_POINT('',(-36.6758703925241,-8.2289783962506,15.));
#19103=CARTESIAN_POINT('',(-36.6758703925241,-8.2289783962506,0.));
#19104=CARTESIAN_POINT('',(-34.5041585975144,-7.74171062993032,15.));
#19105=CARTESIAN_POINT('Origin',(-36.1063209411239,-4.3881627244846,0.));
#19106=CARTESIAN_POINT('',(-35.1136254352094,-4.2675159983083,15.));
#19107=CARTESIAN_POINT('',(-36.199629211057,-3.39252545782466,15.));
#19108=CARTESIAN_POINT('Origin',(-36.1063209411239,-4.3881627244846,15.));
#19109=CARTESIAN_POINT('',(-36.199629211057,-3.39252545782466,0.));
#19110=CARTESIAN_POINT('',(-36.199629211057,-3.39252545782466,0.));
#19111=CARTESIAN_POINT('',(-35.1136254352094,-4.2675159983083,0.));
#19112=CARTESIAN_POINT('Origin',(-36.1063209411239,-4.3881627244846,0.));
#19113=CARTESIAN_POINT('',(-35.1136254352094,-4.2675159983083,0.));
#19114=CARTESIAN_POINT('Origin',(-37.4237196983922,-3.50724370857673,0.));
#19115=CARTESIAN_POINT('',(-37.4237196983922,-3.50724370857673,15.));
#19116=CARTESIAN_POINT('',(-35.2077250236291,-3.29956704137369,15.));
#19117=CARTESIAN_POINT('',(-37.4237196983922,-3.50724370857673,0.));
#19118=CARTESIAN_POINT('',(-37.4237196983922,-3.50724370857673,0.));
#19119=CARTESIAN_POINT('',(-35.2077250236291,-3.29956704137369,0.));
#19120=CARTESIAN_POINT('Origin',(-36.1063209411239,4.38816272448462,0.));
#19121=CARTESIAN_POINT('',(-35.1136254352094,4.26751599830831,0.));
#19122=CARTESIAN_POINT('',(-36.199629211057,3.39252545782467,0.));
#19123=CARTESIAN_POINT('Origin',(-36.1063209411239,4.38816272448462,0.));
#19124=CARTESIAN_POINT('',(-36.199629211057,3.39252545782467,15.));
#19125=CARTESIAN_POINT('',(-36.199629211057,3.39252545782467,0.));
#19126=CARTESIAN_POINT('',(-35.1136254352094,4.26751599830831,15.));
#19127=CARTESIAN_POINT('Origin',(-36.1063209411239,4.38816272448462,15.));
#19128=CARTESIAN_POINT('',(-35.1136254352094,4.26751599830831,0.));
#19129=CARTESIAN_POINT('Origin',(-35.2077250236291,3.29956704137371,0.));
#19130=CARTESIAN_POINT('',(-37.4237196983923,3.50724370857673,0.));
#19131=CARTESIAN_POINT('',(-35.2077250236291,3.29956704137371,0.));
#19132=CARTESIAN_POINT('',(-37.4237196983923,3.50724370857673,15.));
#19133=CARTESIAN_POINT('',(-37.4237196983923,3.50724370857673,0.));
#19134=CARTESIAN_POINT('',(-35.2077250236291,3.29956704137371,15.));
#19135=CARTESIAN_POINT('Origin',(-35.6951686664485,6.98407602147875,0.));
#19136=CARTESIAN_POINT('',(-34.7137772481474,6.79205809501117,15.));
#19137=CARTESIAN_POINT('',(-35.4762412689616,7.95981717292704,15.));
#19138=CARTESIAN_POINT('Origin',(-35.6951686664485,6.98407602147875,15.));
#19139=CARTESIAN_POINT('',(-35.4762412689616,7.95981717292704,0.));
#19140=CARTESIAN_POINT('',(-35.4762412689616,7.95981717292705,0.));
#19141=CARTESIAN_POINT('',(-34.7137772481474,6.79205809501117,0.));
#19142=CARTESIAN_POINT('Origin',(-35.6951686664485,6.98407602147875,0.));
#19143=CARTESIAN_POINT('',(-34.7137772481474,6.79205809501117,0.));
#19144=CARTESIAN_POINT('Origin',(-36.6758703925241,8.22897839625061,0.));
#19145=CARTESIAN_POINT('',(-36.6758703925241,8.22897839625061,15.));
#19146=CARTESIAN_POINT('',(-34.5041585975144,7.74171062993032,15.));
#19147=CARTESIAN_POINT('',(-36.6758703925241,8.22897839625061,0.));
#19148=CARTESIAN_POINT('',(-36.6758703925241,8.22897839625061,0.));
#19149=CARTESIAN_POINT('',(-34.5041585975144,7.74171062993032,0.));
#19150=CARTESIAN_POINT('Origin',(-32.9831349545516,15.3308575288479,0.));
#19151=CARTESIAN_POINT('',(-32.0763073136589,14.909355892181,0.));
#19152=CARTESIAN_POINT('',(-33.3795452283267,14.4127840596497,0.));
#19153=CARTESIAN_POINT('Origin',(-32.9831349545516,15.3308575288479,0.));
#19154=CARTESIAN_POINT('',(-33.3795452283267,14.4127840596497,15.));
#19155=CARTESIAN_POINT('',(-33.3795452283267,14.4127840596497,0.));
#19156=CARTESIAN_POINT('',(-32.0763073136589,14.909355892181,15.));
#19157=CARTESIAN_POINT('Origin',(-32.9831349545516,15.3308575288479,15.));
#19158=CARTESIAN_POINT('',(-32.0763073136589,14.909355892181,0.));
#19159=CARTESIAN_POINT('Origin',(-32.4649140177865,14.0178601012327,0.));
#19160=CARTESIAN_POINT('',(-34.5082745737944,14.9001523628048,0.));
#19161=CARTESIAN_POINT('',(-32.4649140177865,14.0178601012327,0.));
#19162=CARTESIAN_POINT('',(-34.5082745737944,14.9001523628048,15.));
#19163=CARTESIAN_POINT('',(-34.5082745737944,14.9001523628048,0.));
#19164=CARTESIAN_POINT('',(-32.4649140177865,14.0178601012327,15.));
#19165=CARTESIAN_POINT('Origin',(-31.7899245798369,17.6726647455408,0.));
#19166=CARTESIAN_POINT('',(-30.9159026789286,17.1867782189396,15.));
#19167=CARTESIAN_POINT('',(-31.280191653953,18.5329974394853,15.));
#19168=CARTESIAN_POINT('Origin',(-31.7899245798369,17.6726647455408,15.));
#19169=CARTESIAN_POINT('',(-31.280191653953,18.5329974394853,0.));
#19170=CARTESIAN_POINT('',(-31.280191653953,18.5329974394853,0.));
#19171=CARTESIAN_POINT('',(-30.9159026789286,17.1867782189396,0.));
#19172=CARTESIAN_POINT('Origin',(-31.7899245798369,17.6726647455408,0.));
#19173=CARTESIAN_POINT('',(-30.9159026789286,17.1867782189396,0.));
#19174=CARTESIAN_POINT('Origin',(-32.3379313568208,19.1596907609891,0.));
#19175=CARTESIAN_POINT('',(-32.3379313568208,19.1596907609891,15.));
#19176=CARTESIAN_POINT('',(-30.4230847232658,18.0251757251071,15.));
#19177=CARTESIAN_POINT('',(-32.3379313568208,19.1596907609891,0.));
#19178=CARTESIAN_POINT('',(-32.3379313568208,19.1596907609891,0.));
#19179=CARTESIAN_POINT('',(-30.4230847232658,18.0251757251071,0.));
#19180=CARTESIAN_POINT('Origin',(-26.6313299116137,24.7728611819222,0.));
#19181=CARTESIAN_POINT('',(-25.899136743473,24.0917641517363,0.));
#19182=CARTESIAN_POINT('',(-27.2920387896808,24.0222189379449,0.));
#19183=CARTESIAN_POINT('Origin',(-26.6313299116137,24.7728611819222,0.));
#19184=CARTESIAN_POINT('',(-27.2920387896808,24.0222189379449,15.));
#19185=CARTESIAN_POINT('',(-27.2920387896808,24.0222189379449,0.));
#19186=CARTESIAN_POINT('',(-25.899136743473,24.0917641517363,15.));
#19187=CARTESIAN_POINT('Origin',(-26.6313299116137,24.7728611819222,15.));
#19188=CARTESIAN_POINT('',(-25.899136743473,24.0917641517363,0.));
#19189=CARTESIAN_POINT('Origin',(-26.5442110315263,23.3639873462087,0.));
#19190=CARTESIAN_POINT('',(-28.2149191006268,24.8345302882955,0.));
#19191=CARTESIAN_POINT('',(-26.5442110315263,23.3639873462087,0.));
#19192=CARTESIAN_POINT('',(-28.2149191006268,24.8345302882955,15.));
#19193=CARTESIAN_POINT('',(-28.2149191006268,24.8345302882955,0.));
#19194=CARTESIAN_POINT('',(-26.5442110315263,23.3639873462087,15.));
#19195=CARTESIAN_POINT('Origin',(-24.7728611819223,26.6313299116137,0.));
#19196=CARTESIAN_POINT('',(-24.0917641517363,25.899136743473,15.));
#19197=CARTESIAN_POINT('',(-24.0222189379449,27.2920387896808,15.));
#19198=CARTESIAN_POINT('Origin',(-24.7728611819223,26.6313299116137,15.));
#19199=CARTESIAN_POINT('',(-24.0222189379449,27.2920387896808,0.));
#19200=CARTESIAN_POINT('',(-24.0222189379449,27.2920387896808,0.));
#19201=CARTESIAN_POINT('',(-24.0917641517363,25.899136743473,0.));
#19202=CARTESIAN_POINT('Origin',(-24.7728611819223,26.6313299116137,0.));
#19203=CARTESIAN_POINT('',(-24.0917641517363,25.899136743473,0.));
#19204=CARTESIAN_POINT('Origin',(-24.8345302882955,28.2149191006269,0.));
#19205=CARTESIAN_POINT('',(-24.8345302882955,28.2149191006269,15.));
#19206=CARTESIAN_POINT('',(-23.3639873462087,26.5442110315263,15.));
#19207=CARTESIAN_POINT('',(-24.8345302882955,28.2149191006269,0.));
#19208=CARTESIAN_POINT('',(-24.8345302882955,28.2149191006269,0.));
#19209=CARTESIAN_POINT('',(-23.3639873462087,26.5442110315263,0.));
#19210=CARTESIAN_POINT('Origin',(-17.6726647455408,31.7899245798369,0.));
#19211=CARTESIAN_POINT('',(-17.1867782189395,30.9159026789286,0.));
#19212=CARTESIAN_POINT('',(-18.5329974394853,31.280191653953,0.));
#19213=CARTESIAN_POINT('Origin',(-17.6726647455408,31.7899245798369,0.));
#19214=CARTESIAN_POINT('',(-18.5329974394853,31.280191653953,15.));
#19215=CARTESIAN_POINT('',(-18.5329974394853,31.280191653953,0.));
#19216=CARTESIAN_POINT('',(-17.1867782189395,30.9159026789286,15.));
#19217=CARTESIAN_POINT('Origin',(-17.6726647455408,31.7899245798369,15.));
#19218=CARTESIAN_POINT('',(-17.1867782189395,30.9159026789286,0.));
#19219=CARTESIAN_POINT('Origin',(-18.0251757251071,30.4230847232658,0.));
#19220=CARTESIAN_POINT('',(-19.1596907609891,32.3379313568208,0.));
#19221=CARTESIAN_POINT('',(-18.0251757251071,30.4230847232658,0.));
#19222=CARTESIAN_POINT('',(-19.1596907609891,32.3379313568208,15.));
#19223=CARTESIAN_POINT('',(-19.1596907609891,32.3379313568208,0.));
#19224=CARTESIAN_POINT('',(-18.0251757251071,30.4230847232658,15.));
#19225=CARTESIAN_POINT('Origin',(-15.3308575288479,32.9831349545516,0.));
#19226=CARTESIAN_POINT('',(-14.909355892181,32.0763073136589,15.));
#19227=CARTESIAN_POINT('',(-14.4127840596497,33.3795452283267,15.));
#19228=CARTESIAN_POINT('Origin',(-15.3308575288479,32.9831349545516,15.));
#19229=CARTESIAN_POINT('',(-14.4127840596497,33.3795452283267,0.));
#19230=CARTESIAN_POINT('',(-14.4127840596497,33.3795452283267,0.));
#19231=CARTESIAN_POINT('',(-14.909355892181,32.0763073136589,0.));
#19232=CARTESIAN_POINT('Origin',(-15.3308575288479,32.9831349545516,0.));
#19233=CARTESIAN_POINT('',(-14.909355892181,32.0763073136589,0.));
#19234=CARTESIAN_POINT('Origin',(-14.9001523628048,34.5082745737944,0.));
#19235=CARTESIAN_POINT('',(-14.9001523628048,34.5082745737944,15.));
#19236=CARTESIAN_POINT('',(-14.0178601012327,32.4649140177865,15.));
#19237=CARTESIAN_POINT('',(-14.9001523628048,34.5082745737944,0.));
#19238=CARTESIAN_POINT('',(-14.9001523628048,34.5082745737944,0.));
#19239=CARTESIAN_POINT('',(-14.0178601012327,32.4649140177865,0.));
#19240=CARTESIAN_POINT('Origin',(-6.98407602147875,35.6951686664485,0.));
#19241=CARTESIAN_POINT('',(-6.79205809501117,34.7137772481474,0.));
#19242=CARTESIAN_POINT('',(-7.95981717292704,35.4762412689616,0.));
#19243=CARTESIAN_POINT('Origin',(-6.98407602147875,35.6951686664485,0.));
#19244=CARTESIAN_POINT('',(-7.95981717292704,35.4762412689616,15.));
#19245=CARTESIAN_POINT('',(-7.95981717292704,35.4762412689616,0.));
#19246=CARTESIAN_POINT('',(-6.79205809501117,34.7137772481474,15.));
#19247=CARTESIAN_POINT('Origin',(-6.98407602147875,35.6951686664485,15.));
#19248=CARTESIAN_POINT('',(-6.79205809501117,34.7137772481474,0.));
#19249=CARTESIAN_POINT('Origin',(-7.74171062993032,34.5041585975144,0.));
#19250=CARTESIAN_POINT('',(-8.22897839625061,36.6758703925241,0.));
#19251=CARTESIAN_POINT('',(-7.74171062993032,34.5041585975144,0.));
#19252=CARTESIAN_POINT('',(-8.22897839625061,36.6758703925241,15.));
#19253=CARTESIAN_POINT('',(-8.22897839625061,36.6758703925241,0.));
#19254=CARTESIAN_POINT('',(-7.74171062993032,34.5041585975144,15.));
#19255=CARTESIAN_POINT('Origin',(-4.38816272448461,36.1063209411239,0.));
#19256=CARTESIAN_POINT('',(-4.26751599830831,35.1136254352094,15.));
#19257=CARTESIAN_POINT('',(-3.39252545782466,36.199629211057,15.));
#19258=CARTESIAN_POINT('Origin',(-4.38816272448461,36.1063209411239,15.));
#19259=CARTESIAN_POINT('',(-3.39252545782466,36.199629211057,0.));
#19260=CARTESIAN_POINT('',(-3.39252545782466,36.199629211057,0.));
#19261=CARTESIAN_POINT('',(-4.26751599830831,35.1136254352094,0.));
#19262=CARTESIAN_POINT('Origin',(-4.38816272448461,36.1063209411239,0.));
#19263=CARTESIAN_POINT('',(-4.26751599830831,35.1136254352094,0.));
#19264=CARTESIAN_POINT('Origin',(-3.50724370857673,37.4237196983922,0.));
#19265=CARTESIAN_POINT('',(-3.50724370857673,37.4237196983922,15.));
#19266=CARTESIAN_POINT('',(-3.2995670413737,35.2077250236291,15.));
#19267=CARTESIAN_POINT('',(-3.50724370857673,37.4237196983922,0.));
#19268=CARTESIAN_POINT('',(-3.50724370857673,37.4237196983922,0.));
#19269=CARTESIAN_POINT('',(-3.2995670413737,35.2077250236291,0.));
#19270=CARTESIAN_POINT('Origin',(4.38816272448462,36.1063209411239,0.));
#19271=CARTESIAN_POINT('',(4.26751599830831,35.1136254352094,0.));
#19272=CARTESIAN_POINT('',(3.39252545782467,36.199629211057,0.));
#19273=CARTESIAN_POINT('Origin',(4.38816272448462,36.1063209411239,0.));
#19274=CARTESIAN_POINT('',(3.39252545782467,36.199629211057,15.));
#19275=CARTESIAN_POINT('',(3.39252545782467,36.199629211057,0.));
#19276=CARTESIAN_POINT('',(4.26751599830831,35.1136254352094,15.));
#19277=CARTESIAN_POINT('Origin',(4.38816272448462,36.1063209411239,15.));
#19278=CARTESIAN_POINT('',(4.26751599830831,35.1136254352094,0.));
#19279=CARTESIAN_POINT('Origin',(3.2995670413737,35.2077250236291,0.));
#19280=CARTESIAN_POINT('',(3.50724370857673,37.4237196983923,0.));
#19281=CARTESIAN_POINT('',(3.2995670413737,35.2077250236291,0.));
#19282=CARTESIAN_POINT('',(3.50724370857673,37.4237196983923,15.));
#19283=CARTESIAN_POINT('',(3.50724370857673,37.4237196983923,0.));
#19284=CARTESIAN_POINT('',(3.2995670413737,35.2077250236291,15.));
#19285=CARTESIAN_POINT('Origin',(6.98407602147876,35.6951686664485,0.));
#19286=CARTESIAN_POINT('',(6.79205809501118,34.7137772481474,15.));
#19287=CARTESIAN_POINT('',(7.95981717292704,35.4762412689616,15.));
#19288=CARTESIAN_POINT('Origin',(6.98407602147876,35.6951686664485,15.));
#19289=CARTESIAN_POINT('',(7.95981717292704,35.4762412689616,0.));
#19290=CARTESIAN_POINT('',(7.95981717292705,35.4762412689616,0.));
#19291=CARTESIAN_POINT('',(6.79205809501118,34.7137772481474,0.));
#19292=CARTESIAN_POINT('Origin',(6.98407602147876,35.6951686664485,0.));
#19293=CARTESIAN_POINT('',(6.79205809501118,34.7137772481474,0.));
#19294=CARTESIAN_POINT('Origin',(8.22897839625062,36.6758703925241,0.));
#19295=CARTESIAN_POINT('',(8.22897839625062,36.6758703925241,15.));
#19296=CARTESIAN_POINT('',(7.74171062993033,34.5041585975144,15.));
#19297=CARTESIAN_POINT('',(8.22897839625062,36.6758703925241,0.));
#19298=CARTESIAN_POINT('',(8.22897839625062,36.6758703925241,0.));
#19299=CARTESIAN_POINT('',(7.74171062993033,34.5041585975144,0.));
#19300=CARTESIAN_POINT('Origin',(15.3308575288479,32.9831349545517,0.));
#19301=CARTESIAN_POINT('',(14.909355892181,32.0763073136589,0.));
#19302=CARTESIAN_POINT('',(14.4127840596497,33.3795452283267,0.));
#19303=CARTESIAN_POINT('Origin',(15.3308575288479,32.9831349545517,0.));
#19304=CARTESIAN_POINT('',(14.4127840596497,33.3795452283267,15.));
#19305=CARTESIAN_POINT('',(14.4127840596497,33.3795452283267,0.));
#19306=CARTESIAN_POINT('',(14.909355892181,32.0763073136589,15.));
#19307=CARTESIAN_POINT('Origin',(15.3308575288479,32.9831349545517,15.));
#19308=CARTESIAN_POINT('',(14.909355892181,32.0763073136589,0.));
#19309=CARTESIAN_POINT('Origin',(14.0178601012327,32.4649140177865,0.));
#19310=CARTESIAN_POINT('',(14.9001523628048,34.5082745737944,0.));
#19311=CARTESIAN_POINT('',(14.0178601012327,32.4649140177865,0.));
#19312=CARTESIAN_POINT('',(14.9001523628048,34.5082745737944,15.));
#19313=CARTESIAN_POINT('',(14.9001523628048,34.5082745737944,0.));
#19314=CARTESIAN_POINT('',(14.0178601012327,32.4649140177865,15.));
#19315=CARTESIAN_POINT('Origin',(17.6726647455408,31.7899245798369,0.));
#19316=CARTESIAN_POINT('',(17.1867782189396,30.9159026789286,15.));
#19317=CARTESIAN_POINT('',(18.5329974394853,31.280191653953,15.));
#19318=CARTESIAN_POINT('Origin',(17.6726647455408,31.7899245798369,15.));
#19319=CARTESIAN_POINT('',(18.5329974394853,31.280191653953,0.));
#19320=CARTESIAN_POINT('',(18.5329974394853,31.280191653953,0.));
#19321=CARTESIAN_POINT('',(17.1867782189396,30.9159026789286,0.));
#19322=CARTESIAN_POINT('Origin',(17.6726647455408,31.7899245798369,0.));
#19323=CARTESIAN_POINT('',(17.1867782189396,30.9159026789286,0.));
#19324=CARTESIAN_POINT('Origin',(19.1596907609891,32.3379313568208,0.));
#19325=CARTESIAN_POINT('',(19.1596907609891,32.3379313568208,15.));
#19326=CARTESIAN_POINT('',(18.0251757251071,30.4230847232658,15.));
#19327=CARTESIAN_POINT('',(19.1596907609891,32.3379313568208,0.));
#19328=CARTESIAN_POINT('',(19.1596907609891,32.3379313568208,0.));
#19329=CARTESIAN_POINT('',(18.0251757251071,30.4230847232658,0.));
#19330=CARTESIAN_POINT('Origin',(24.7728611819223,26.6313299116137,0.));
#19331=CARTESIAN_POINT('',(24.0917641517363,25.899136743473,0.));
#19332=CARTESIAN_POINT('',(24.0222189379449,27.2920387896808,0.));
#19333=CARTESIAN_POINT('Origin',(24.7728611819223,26.6313299116137,0.));
#19334=CARTESIAN_POINT('',(24.0222189379449,27.2920387896808,15.));
#19335=CARTESIAN_POINT('',(24.0222189379449,27.2920387896808,0.));
#19336=CARTESIAN_POINT('',(24.0917641517363,25.899136743473,15.));
#19337=CARTESIAN_POINT('Origin',(24.7728611819223,26.6313299116137,15.));
#19338=CARTESIAN_POINT('',(24.0917641517363,25.899136743473,0.));
#19339=CARTESIAN_POINT('Origin',(23.3639873462087,26.5442110315263,0.));
#19340=CARTESIAN_POINT('',(24.8345302882955,28.2149191006268,0.));
#19341=CARTESIAN_POINT('',(23.3639873462087,26.5442110315263,0.));
#19342=CARTESIAN_POINT('',(24.8345302882955,28.2149191006268,15.));
#19343=CARTESIAN_POINT('',(24.8345302882955,28.2149191006268,0.));
#19344=CARTESIAN_POINT('',(23.3639873462087,26.5442110315263,15.));
#19345=CARTESIAN_POINT('Origin',(26.6313299116137,24.7728611819223,0.));
#19346=CARTESIAN_POINT('',(25.899136743473,24.0917641517363,15.));
#19347=CARTESIAN_POINT('',(27.2920387896808,24.0222189379449,15.));
#19348=CARTESIAN_POINT('Origin',(26.6313299116137,24.7728611819223,15.));
#19349=CARTESIAN_POINT('',(27.2920387896808,24.0222189379449,0.));
#19350=CARTESIAN_POINT('',(27.2920387896808,24.0222189379449,0.));
#19351=CARTESIAN_POINT('',(25.899136743473,24.0917641517363,0.));
#19352=CARTESIAN_POINT('Origin',(26.6313299116137,24.7728611819223,0.));
#19353=CARTESIAN_POINT('',(25.899136743473,24.0917641517363,0.));
#19354=CARTESIAN_POINT('Origin',(28.2149191006269,24.8345302882955,0.));
#19355=CARTESIAN_POINT('',(28.2149191006269,24.8345302882955,15.));
#19356=CARTESIAN_POINT('',(26.5442110315263,23.3639873462087,15.));
#19357=CARTESIAN_POINT('',(28.2149191006269,24.8345302882955,0.));
#19358=CARTESIAN_POINT('',(28.2149191006269,24.8345302882955,0.));
#19359=CARTESIAN_POINT('',(26.5442110315263,23.3639873462087,0.));
#19360=CARTESIAN_POINT('Origin',(31.7899245798369,17.6726647455408,0.));
#19361=CARTESIAN_POINT('',(30.9159026789286,17.1867782189396,0.));
#19362=CARTESIAN_POINT('',(31.280191653953,18.5329974394853,0.));
#19363=CARTESIAN_POINT('Origin',(31.7899245798369,17.6726647455408,0.));
#19364=CARTESIAN_POINT('',(31.280191653953,18.5329974394853,15.));
#19365=CARTESIAN_POINT('',(31.280191653953,18.5329974394853,0.));
#19366=CARTESIAN_POINT('',(30.9159026789286,17.1867782189396,15.));
#19367=CARTESIAN_POINT('Origin',(31.7899245798369,17.6726647455408,15.));
#19368=CARTESIAN_POINT('',(30.9159026789286,17.1867782189396,0.));
#19369=CARTESIAN_POINT('Origin',(30.4230847232658,18.0251757251071,0.));
#19370=CARTESIAN_POINT('',(32.3379313568208,19.1596907609891,0.));
#19371=CARTESIAN_POINT('',(30.4230847232658,18.0251757251071,0.));
#19372=CARTESIAN_POINT('',(32.3379313568208,19.1596907609891,15.));
#19373=CARTESIAN_POINT('',(32.3379313568208,19.1596907609891,0.));
#19374=CARTESIAN_POINT('',(30.4230847232658,18.0251757251071,15.));
#19375=CARTESIAN_POINT('Origin',(32.9831349545516,15.3308575288479,0.));
#19376=CARTESIAN_POINT('',(32.0763073136589,14.909355892181,15.));
#19377=CARTESIAN_POINT('',(33.3795452283267,14.4127840596497,15.));
#19378=CARTESIAN_POINT('Origin',(32.9831349545516,15.3308575288479,15.));
#19379=CARTESIAN_POINT('',(33.3795452283267,14.4127840596497,0.));
#19380=CARTESIAN_POINT('',(33.3795452283267,14.4127840596497,0.));
#19381=CARTESIAN_POINT('',(32.0763073136589,14.909355892181,0.));
#19382=CARTESIAN_POINT('Origin',(32.9831349545516,15.3308575288479,0.));
#19383=CARTESIAN_POINT('',(32.0763073136589,14.909355892181,0.));
#19384=CARTESIAN_POINT('Origin',(34.5082745737944,14.9001523628048,0.));
#19385=CARTESIAN_POINT('',(34.5082745737944,14.9001523628048,15.));
#19386=CARTESIAN_POINT('',(32.4649140177865,14.0178601012327,15.));
#19387=CARTESIAN_POINT('',(34.5082745737944,14.9001523628048,0.));
#19388=CARTESIAN_POINT('',(34.5082745737944,14.9001523628048,0.));
#19389=CARTESIAN_POINT('',(32.4649140177865,14.0178601012327,0.));
#19390=CARTESIAN_POINT('Origin',(35.6951686664485,6.98407602147875,0.));
#19391=CARTESIAN_POINT('',(34.7137772481474,6.79205809501117,0.));
#19392=CARTESIAN_POINT('',(35.4762412689616,7.95981717292704,0.));
#19393=CARTESIAN_POINT('Origin',(35.6951686664485,6.98407602147875,0.));
#19394=CARTESIAN_POINT('',(35.4762412689616,7.95981717292704,15.));
#19395=CARTESIAN_POINT('',(35.4762412689616,7.95981717292704,0.));
#19396=CARTESIAN_POINT('',(34.7137772481474,6.79205809501117,15.));
#19397=CARTESIAN_POINT('Origin',(35.6951686664485,6.98407602147875,15.));
#19398=CARTESIAN_POINT('',(34.7137772481474,6.79205809501117,0.));
#19399=CARTESIAN_POINT('Origin',(34.5041585975144,7.74171062993032,0.));
#19400=CARTESIAN_POINT('',(36.6758703925241,8.22897839625061,0.));
#19401=CARTESIAN_POINT('',(34.5041585975144,7.74171062993032,0.));
#19402=CARTESIAN_POINT('',(36.6758703925241,8.22897839625061,15.));
#19403=CARTESIAN_POINT('',(36.6758703925241,8.22897839625061,0.));
#19404=CARTESIAN_POINT('',(34.5041585975144,7.74171062993032,15.));
#19405=CARTESIAN_POINT('Ctrl Pts',(42.2550026135057,-12.2684454652018,0.));
#19406=CARTESIAN_POINT('Ctrl Pts',(42.2550026135057,-12.2684454652018,18.));
#19407=CARTESIAN_POINT('Ctrl Pts',(42.2409327400055,-12.2530833383985,0.));
#19408=CARTESIAN_POINT('Ctrl Pts',(42.2409327400055,-12.2530833383985,18.));
#19409=CARTESIAN_POINT('Ctrl Pts',(42.2127669677092,-12.222401466668,0.));
#19410=CARTESIAN_POINT('Ctrl Pts',(42.2127669677092,-12.222401466668,18.));
#19411=CARTESIAN_POINT('Ctrl Pts',(42.1704402333854,-12.1765058047069,0.));
#19412=CARTESIAN_POINT('Ctrl Pts',(42.1704402333854,-12.1765058047069,18.));
#19413=CARTESIAN_POINT('Ctrl Pts',(42.1138483839101,-12.1155659644537,0.));
#19414=CARTESIAN_POINT('Ctrl Pts',(42.1138483839101,-12.1155659644537,18.));
#19415=CARTESIAN_POINT('Ctrl Pts',(42.0428479428228,-12.0398158079102,0.));
#19416=CARTESIAN_POINT('Ctrl Pts',(42.0428479428228,-12.0398158079102,18.));
#19417=CARTESIAN_POINT('Ctrl Pts',(41.9715865222182,-11.9644914999263,0.));
#19418=CARTESIAN_POINT('Ctrl Pts',(41.9715865222182,-11.9644914999263,18.));
#19419=CARTESIAN_POINT('Ctrl Pts',(41.9000638152266,-11.8895948153349,0.));
#19420=CARTESIAN_POINT('Ctrl Pts',(41.9000638152266,-11.8895948153349,18.));
#19421=CARTESIAN_POINT('Ctrl Pts',(41.8282796562569,-11.81512813804,0.));
#19422=CARTESIAN_POINT('Ctrl Pts',(41.8282796562569,-11.81512813804,18.));
#19423=CARTESIAN_POINT('Ctrl Pts',(41.7562341395977,-11.7410945211992,0.));
#19424=CARTESIAN_POINT('Ctrl Pts',(41.7562341395977,-11.7410945211992,18.));
#19425=CARTESIAN_POINT('Ctrl Pts',(41.6839275596248,-11.6674975352852,0.));
#19426=CARTESIAN_POINT('Ctrl Pts',(41.6839275596248,-11.6674975352852,18.));
#19427=CARTESIAN_POINT('Ctrl Pts',(41.6113603270596,-11.5943410868252,0.));
#19428=CARTESIAN_POINT('Ctrl Pts',(41.6113603270596,-11.5943410868252,18.));
#19429=CARTESIAN_POINT('Ctrl Pts',(41.5385328935506,-11.5216292382388,0.));
#19430=CARTESIAN_POINT('Ctrl Pts',(41.5385328935506,-11.5216292382388,18.));
#19431=CARTESIAN_POINT('Ctrl Pts',(41.4654456796071,-11.449366039385,0.));
#19432=CARTESIAN_POINT('Ctrl Pts',(41.4654456796071,-11.449366039385,18.));
#19433=CARTESIAN_POINT('Ctrl Pts',(41.3920989905986,-11.3775553120177,0.));
#19434=CARTESIAN_POINT('Ctrl Pts',(41.3920989905986,-11.3775553120177,18.));
#19435=CARTESIAN_POINT('Ctrl Pts',(41.3184930194148,-11.3062006993745,0.));
#19436=CARTESIAN_POINT('Ctrl Pts',(41.3184930194148,-11.3062006993745,18.));
#19437=CARTESIAN_POINT('Ctrl Pts',(41.2446278781981,-11.2353057980338,0.));
#19438=CARTESIAN_POINT('Ctrl Pts',(41.2446278781981,-11.2353057980338,18.));
#19439=CARTESIAN_POINT('Ctrl Pts',(41.1705036228854,-11.1648742640378,0.));
#19440=CARTESIAN_POINT('Ctrl Pts',(41.1705036228854,-11.1648742640378,18.));
#19441=CARTESIAN_POINT('Ctrl Pts',(41.0961202807715,-11.0949099155251,0.));
#19442=CARTESIAN_POINT('Ctrl Pts',(41.0961202807715,-11.0949099155251,18.));
#19443=CARTESIAN_POINT('Ctrl Pts',(41.0214778832142,-11.0254168609972,0.));
#19444=CARTESIAN_POINT('Ctrl Pts',(41.0214778832142,-11.0254168609972,18.));
#19445=CARTESIAN_POINT('Ctrl Pts',(40.9465764747798,-10.956399476781,0.));
#19446=CARTESIAN_POINT('Ctrl Pts',(40.9465764747798,-10.956399476781,18.));
#19447=CARTESIAN_POINT('Ctrl Pts',(40.8714161092412,-10.8878623066647,0.));
#19448=CARTESIAN_POINT('Ctrl Pts',(40.8714161092412,-10.8878623066647,18.));
#19449=CARTESIAN_POINT('Ctrl Pts',(40.7959968527561,-10.8198099757795,0.));
#19450=CARTESIAN_POINT('Ctrl Pts',(40.7959968527561,-10.8198099757795,18.));
#19451=CARTESIAN_POINT('Ctrl Pts',(40.7203187831783,-10.7522471109694,0.));
#19452=CARTESIAN_POINT('Ctrl Pts',(40.7203187831783,-10.7522471109694,18.));
#19453=CARTESIAN_POINT('Ctrl Pts',(40.6443819999244,-10.6851782157325,0.));
#19454=CARTESIAN_POINT('Ctrl Pts',(40.6443819999244,-10.6851782157325,18.));
#19455=CARTESIAN_POINT('Ctrl Pts',(40.5681866012103,-10.618607730849,0.));
#19456=CARTESIAN_POINT('Ctrl Pts',(40.5681866012103,-10.618607730849,18.));
#19457=CARTESIAN_POINT('Ctrl Pts',(40.4917326404439,-10.5525402237951,0.));
#19458=CARTESIAN_POINT('Ctrl Pts',(40.4917326404439,-10.5525402237951,18.));
#19459=CARTESIAN_POINT('Ctrl Pts',(40.4150200869536,-10.48698054978,0.));
#19460=CARTESIAN_POINT('Ctrl Pts',(40.4150200869536,-10.48698054978,18.));
#19461=CARTESIAN_POINT('Ctrl Pts',(40.3380487942952,-10.4219339932951,0.));
#19462=CARTESIAN_POINT('Ctrl Pts',(40.3380487942952,-10.4219339932951,18.));
#19463=CARTESIAN_POINT('Ctrl Pts',(40.2608184485326,-10.3574064830678,0.));
#19464=CARTESIAN_POINT('Ctrl Pts',(40.2608184485326,-10.3574064830678,18.));
#19465=CARTESIAN_POINT('Ctrl Pts',(40.1833286010098,-10.2934044990237,0.));
#19466=CARTESIAN_POINT('Ctrl Pts',(40.1833286010098,-10.2934044990237,18.));
#19467=CARTESIAN_POINT('Ctrl Pts',(40.1055787732578,-10.2299347125857,0.));
#19468=CARTESIAN_POINT('Ctrl Pts',(40.1055787732578,-10.2299347125857,18.));
#19469=CARTESIAN_POINT('Ctrl Pts',(40.0275685525923,-10.1670036683795,0.));
#19470=CARTESIAN_POINT('Ctrl Pts',(40.0275685525923,-10.1670036683795,18.));
#19471=CARTESIAN_POINT('Ctrl Pts',(39.9492976736738,-10.1046175096878,0.));
#19472=CARTESIAN_POINT('Ctrl Pts',(39.9492976736738,-10.1046175096878,18.));
#19473=CARTESIAN_POINT('Ctrl Pts',(39.8707661565233,-10.0427815229883,0.));
#19474=CARTESIAN_POINT('Ctrl Pts',(39.8707661565233,-10.0427815229883,18.));
#19475=CARTESIAN_POINT('Ctrl Pts',(39.7919742367922,-9.98150036150824,0.));
#19476=CARTESIAN_POINT('Ctrl Pts',(39.7919742367922,-9.98150036150824,18.));
#19477=CARTESIAN_POINT('Ctrl Pts',(39.712922089547,-9.92077894513193,0.));
#19478=CARTESIAN_POINT('Ctrl Pts',(39.712922089547,-9.92077894513193,18.));
#19479=CARTESIAN_POINT('Ctrl Pts',(39.6336095893767,-9.86062324242561,0.));
#19480=CARTESIAN_POINT('Ctrl Pts',(39.6336095893767,-9.86062324242561,18.));
#19481=CARTESIAN_POINT('Ctrl Pts',(39.5540361022309,-9.80104095251614,0.));
#19482=CARTESIAN_POINT('Ctrl Pts',(39.5540361022309,-9.80104095251614,18.));
#19483=CARTESIAN_POINT('Ctrl Pts',(39.4742001555227,-9.74204258152664,0.));
#19484=CARTESIAN_POINT('Ctrl Pts',(39.4742001555227,-9.74204258152664,18.));
#19485=CARTESIAN_POINT('Ctrl Pts',(39.3940995760289,-9.68364100883828,0.));
#19486=CARTESIAN_POINT('Ctrl Pts',(39.3940995760289,-9.68364100883828,18.));
#19487=CARTESIAN_POINT('Ctrl Pts',(39.3137321153686,-9.62584947846544,0.));
#19488=CARTESIAN_POINT('Ctrl Pts',(39.3137321153686,-9.62584947846544,18.));
#19489=CARTESIAN_POINT('Ctrl Pts',(39.2330959982788,-9.56867984233624,0.));
#19490=CARTESIAN_POINT('Ctrl Pts',(39.2330959982788,-9.56867984233624,18.));
#19491=CARTESIAN_POINT('Ctrl Pts',(39.1521903958955,-9.51214104535621,0.));
#19492=CARTESIAN_POINT('Ctrl Pts',(39.1521903958955,-9.51214104535621,18.));
#19493=CARTESIAN_POINT('Ctrl Pts',(39.0710161994951,-9.45623664577432,0.));
#19494=CARTESIAN_POINT('Ctrl Pts',(39.0710161994951,-9.45623664577432,18.));
#19495=CARTESIAN_POINT('Ctrl Pts',(38.9895756526779,-9.40096600877644,0.));
#19496=CARTESIAN_POINT('Ctrl Pts',(38.9895756526779,-9.40096600877644,18.));
#19497=CARTESIAN_POINT('Ctrl Pts',(38.9078708427078,-9.34632917154637,0.));
#19498=CARTESIAN_POINT('Ctrl Pts',(38.9078708427078,-9.34632917154637,18.));
#19499=CARTESIAN_POINT('Ctrl Pts',(38.8259023794241,-9.29233110570904,0.));
#19500=CARTESIAN_POINT('Ctrl Pts',(38.8259023794241,-9.29233110570904,18.));
#19501=CARTESIAN_POINT('Ctrl Pts',(38.7436682576832,-9.23898539199332,0.));
#19502=CARTESIAN_POINT('Ctrl Pts',(38.7436682576832,-9.23898539199332,18.));
#19503=CARTESIAN_POINT('Ctrl Pts',(38.6611620045193,-9.1863201939433,0.));
#19504=CARTESIAN_POINT('Ctrl Pts',(38.6611620045193,-9.1863201939433,18.));
#19505=CARTESIAN_POINT('Ctrl Pts',(38.5783736628826,-9.13437512010587,0.));
#19506=CARTESIAN_POINT('Ctrl Pts',(38.5783736628826,-9.13437512010587,18.));
#19507=CARTESIAN_POINT('Ctrl Pts',(38.4952932486131,-9.08319014288087,0.));
#19508=CARTESIAN_POINT('Ctrl Pts',(38.4952932486131,-9.08319014288087,18.));
#19509=CARTESIAN_POINT('Ctrl Pts',(38.4119138099805,-9.03279579360191,0.));
#19510=CARTESIAN_POINT('Ctrl Pts',(38.4119138099805,-9.03279579360191,18.));
#19511=CARTESIAN_POINT('Ctrl Pts',(38.3282340281403,-8.98320483785761,0.));
#19512=CARTESIAN_POINT('Ctrl Pts',(38.3282340281403,-8.98320483785761,18.));
#19513=CARTESIAN_POINT('Ctrl Pts',(38.2442625706309,-8.9343983099634,0.));
#19514=CARTESIAN_POINT('Ctrl Pts',(38.2442625706309,-8.9343983099634,18.));
#19515=CARTESIAN_POINT('Ctrl Pts',(38.1600150482528,-8.88633535238435,0.));
#19516=CARTESIAN_POINT('Ctrl Pts',(38.1600150482528,-8.88633535238435,18.));
#19517=CARTESIAN_POINT('Ctrl Pts',(38.0755058326913,-8.8389795976335,0.));
#19518=CARTESIAN_POINT('Ctrl Pts',(38.0755058326913,-8.8389795976335,18.));
#19519=CARTESIAN_POINT('Ctrl Pts',(37.9907407304174,-8.79232279131093,0.));
#19520=CARTESIAN_POINT('Ctrl Pts',(37.9907407304174,-8.79232279131093,18.));
#19521=CARTESIAN_POINT('Ctrl Pts',(37.9057107230066,-8.74640499479003,0.));
#19522=CARTESIAN_POINT('Ctrl Pts',(37.9057107230066,-8.74640499479003,18.));
#19523=CARTESIAN_POINT('Ctrl Pts',(37.8203816669031,-8.70134776631144,0.));
#19524=CARTESIAN_POINT('Ctrl Pts',(37.8203816669031,-8.70134776631144,18.));
#19525=CARTESIAN_POINT('Ctrl Pts',(37.7347032383719,-8.65732553894525,0.));
#19526=CARTESIAN_POINT('Ctrl Pts',(37.7347032383719,-8.65732553894525,18.));
#19527=CARTESIAN_POINT('Ctrl Pts',(37.6486274754754,-8.61450621749156,0.));
#19528=CARTESIAN_POINT('Ctrl Pts',(37.6486274754754,-8.61450621749156,18.));
#19529=CARTESIAN_POINT('Ctrl Pts',(37.5621256752108,-8.57299698459467,0.));
#19530=CARTESIAN_POINT('Ctrl Pts',(37.5621256752108,-8.57299698459467,18.));
#19531=CARTESIAN_POINT('Ctrl Pts',(37.4752030152968,-8.53279758643785,0.));
#19532=CARTESIAN_POINT('Ctrl Pts',(37.4752030152968,-8.53279758643785,18.));
#19533=CARTESIAN_POINT('Ctrl Pts',(37.3879218093514,-8.49372546467076,0.));
#19534=CARTESIAN_POINT('Ctrl Pts',(37.3879218093514,-8.49372546467076,18.));
#19535=CARTESIAN_POINT('Ctrl Pts',(37.3003733151561,-8.45550849433961,0.));
#19536=CARTESIAN_POINT('Ctrl Pts',(37.3003733151561,-8.45550849433961,18.));
#19537=CARTESIAN_POINT('Ctrl Pts',(37.2126332013933,-8.41793088313261,0.));
#19538=CARTESIAN_POINT('Ctrl Pts',(37.2126332013933,-8.41793088313261,18.));
#19539=CARTESIAN_POINT('Ctrl Pts',(37.1247207489179,-8.38096706211449,0.));
#19540=CARTESIAN_POINT('Ctrl Pts',(37.1247207489179,-8.38096706211449,18.));
#19541=CARTESIAN_POINT('Ctrl Pts',(37.0365602155148,-8.3449081895264,0.));
#19542=CARTESIAN_POINT('Ctrl Pts',(37.0365602155148,-8.3449081895264,18.));
#19543=CARTESIAN_POINT('Ctrl Pts',(36.9479311729484,-8.31052547794592,0.));
#19544=CARTESIAN_POINT('Ctrl Pts',(36.9479311729484,-8.31052547794592,18.));
#19545=CARTESIAN_POINT('Ctrl Pts',(36.8585291300917,-8.27886599440786,0.));
#19546=CARTESIAN_POINT('Ctrl Pts',(36.8585291300917,-8.27886599440786,18.));
#19547=CARTESIAN_POINT('Ctrl Pts',(36.7861403757604,-8.25656657451821,0.));
#19548=CARTESIAN_POINT('Ctrl Pts',(36.7861403757604,-8.25656657451821,18.));
#19549=CARTESIAN_POINT('Ctrl Pts',(36.7312504697652,-8.24192165947368,0.));
#19550=CARTESIAN_POINT('Ctrl Pts',(36.7312504697652,-8.24192165947368,18.));
#19551=CARTESIAN_POINT('Ctrl Pts',(36.6943771018148,-8.23313075335377,0.));
#19552=CARTESIAN_POINT('Ctrl Pts',(36.6943771018148,-8.23313075335377,18.));
#19553=CARTESIAN_POINT('Ctrl Pts',(36.6758703925241,-8.22897839625062,0.));
#19554=CARTESIAN_POINT('Ctrl Pts',(36.6758703925241,-8.22897839625062,18.));
#19555=CARTESIAN_POINT('',(42.2550026135057,-12.2684454652017,0.));
#19556=CARTESIAN_POINT('Ctrl Pts',(36.6758703925241,-8.22897839625062,0.));
#19557=CARTESIAN_POINT('Ctrl Pts',(36.6943771018148,-8.23313075335377,0.));
#19558=CARTESIAN_POINT('Ctrl Pts',(36.7312504697652,-8.24192165947368,0.));
#19559=CARTESIAN_POINT('Ctrl Pts',(36.7861403757604,-8.25656657451821,0.));
#19560=CARTESIAN_POINT('Ctrl Pts',(36.8585291300917,-8.27886599440786,0.));
#19561=CARTESIAN_POINT('Ctrl Pts',(36.9479311729484,-8.31052547794592,0.));
#19562=CARTESIAN_POINT('Ctrl Pts',(37.0365602155148,-8.3449081895264,0.));
#19563=CARTESIAN_POINT('Ctrl Pts',(37.1247207489179,-8.38096706211449,0.));
#19564=CARTESIAN_POINT('Ctrl Pts',(37.2126332013933,-8.41793088313261,0.));
#19565=CARTESIAN_POINT('Ctrl Pts',(37.3003733151561,-8.45550849433961,0.));
#19566=CARTESIAN_POINT('Ctrl Pts',(37.3879218093514,-8.49372546467076,0.));
#19567=CARTESIAN_POINT('Ctrl Pts',(37.4752030152968,-8.53279758643785,0.));
#19568=CARTESIAN_POINT('Ctrl Pts',(37.5621256752108,-8.57299698459467,0.));
#19569=CARTESIAN_POINT('Ctrl Pts',(37.6486274754754,-8.61450621749156,0.));
#19570=CARTESIAN_POINT('Ctrl Pts',(37.7347032383719,-8.65732553894525,0.));
#19571=CARTESIAN_POINT('Ctrl Pts',(37.8203816669031,-8.70134776631144,0.));
#19572=CARTESIAN_POINT('Ctrl Pts',(37.9057107230066,-8.74640499479003,0.));
#19573=CARTESIAN_POINT('Ctrl Pts',(37.9907407304174,-8.79232279131093,0.));
#19574=CARTESIAN_POINT('Ctrl Pts',(38.0755058326913,-8.8389795976335,0.));
#19575=CARTESIAN_POINT('Ctrl Pts',(38.1600150482528,-8.88633535238435,0.));
#19576=CARTESIAN_POINT('Ctrl Pts',(38.2442625706309,-8.9343983099634,0.));
#19577=CARTESIAN_POINT('Ctrl Pts',(38.3282340281403,-8.98320483785761,0.));
#19578=CARTESIAN_POINT('Ctrl Pts',(38.4119138099805,-9.03279579360191,0.));
#19579=CARTESIAN_POINT('Ctrl Pts',(38.4952932486131,-9.08319014288087,0.));
#19580=CARTESIAN_POINT('Ctrl Pts',(38.5783736628826,-9.13437512010587,0.));
#19581=CARTESIAN_POINT('Ctrl Pts',(38.6611620045193,-9.1863201939433,0.));
#19582=CARTESIAN_POINT('Ctrl Pts',(38.7436682576832,-9.23898539199332,0.));
#19583=CARTESIAN_POINT('Ctrl Pts',(38.8259023794241,-9.29233110570904,0.));
#19584=CARTESIAN_POINT('Ctrl Pts',(38.9078708427078,-9.34632917154637,0.));
#19585=CARTESIAN_POINT('Ctrl Pts',(38.9895756526779,-9.40096600877644,0.));
#19586=CARTESIAN_POINT('Ctrl Pts',(39.0710161994951,-9.45623664577432,0.));
#19587=CARTESIAN_POINT('Ctrl Pts',(39.1521903958955,-9.51214104535621,0.));
#19588=CARTESIAN_POINT('Ctrl Pts',(39.2330959982788,-9.56867984233624,0.));
#19589=CARTESIAN_POINT('Ctrl Pts',(39.3137321153686,-9.62584947846544,0.));
#19590=CARTESIAN_POINT('Ctrl Pts',(39.3940995760289,-9.68364100883828,0.));
#19591=CARTESIAN_POINT('Ctrl Pts',(39.4742001555227,-9.74204258152664,0.));
#19592=CARTESIAN_POINT('Ctrl Pts',(39.5540361022309,-9.80104095251614,0.));
#19593=CARTESIAN_POINT('Ctrl Pts',(39.6336095893767,-9.86062324242561,0.));
#19594=CARTESIAN_POINT('Ctrl Pts',(39.712922089547,-9.92077894513193,0.));
#19595=CARTESIAN_POINT('Ctrl Pts',(39.7919742367922,-9.98150036150824,0.));
#19596=CARTESIAN_POINT('Ctrl Pts',(39.8707661565233,-10.0427815229883,0.));
#19597=CARTESIAN_POINT('Ctrl Pts',(39.9492976736738,-10.1046175096878,0.));
#19598=CARTESIAN_POINT('Ctrl Pts',(40.0275685525923,-10.1670036683795,0.));
#19599=CARTESIAN_POINT('Ctrl Pts',(40.1055787732578,-10.2299347125857,0.));
#19600=CARTESIAN_POINT('Ctrl Pts',(40.1833286010098,-10.2934044990237,0.));
#19601=CARTESIAN_POINT('Ctrl Pts',(40.2608184485326,-10.3574064830678,0.));
#19602=CARTESIAN_POINT('Ctrl Pts',(40.3380487942952,-10.4219339932951,0.));
#19603=CARTESIAN_POINT('Ctrl Pts',(40.4150200869536,-10.48698054978,0.));
#19604=CARTESIAN_POINT('Ctrl Pts',(40.4917326404439,-10.5525402237951,0.));
#19605=CARTESIAN_POINT('Ctrl Pts',(40.5681866012103,-10.618607730849,0.));
#19606=CARTESIAN_POINT('Ctrl Pts',(40.6443819999244,-10.6851782157325,0.));
#19607=CARTESIAN_POINT('Ctrl Pts',(40.7203187831783,-10.7522471109694,0.));
#19608=CARTESIAN_POINT('Ctrl Pts',(40.7959968527561,-10.8198099757795,0.));
#19609=CARTESIAN_POINT('Ctrl Pts',(40.8714161092412,-10.8878623066647,0.));
#19610=CARTESIAN_POINT('Ctrl Pts',(40.9465764747798,-10.956399476781,0.));
#19611=CARTESIAN_POINT('Ctrl Pts',(41.0214778832142,-11.0254168609972,0.));
#19612=CARTESIAN_POINT('Ctrl Pts',(41.0961202807715,-11.0949099155251,0.));
#19613=CARTESIAN_POINT('Ctrl Pts',(41.1705036228854,-11.1648742640378,0.));
#19614=CARTESIAN_POINT('Ctrl Pts',(41.2446278781981,-11.2353057980338,0.));
#19615=CARTESIAN_POINT('Ctrl Pts',(41.3184930194148,-11.3062006993745,0.));
#19616=CARTESIAN_POINT('Ctrl Pts',(41.3920989905986,-11.3775553120177,0.));
#19617=CARTESIAN_POINT('Ctrl Pts',(41.4654456796071,-11.449366039385,0.));
#19618=CARTESIAN_POINT('Ctrl Pts',(41.5385328935506,-11.5216292382388,0.));
#19619=CARTESIAN_POINT('Ctrl Pts',(41.6113603270596,-11.5943410868252,0.));
#19620=CARTESIAN_POINT('Ctrl Pts',(41.6839275596248,-11.6674975352852,0.));
#19621=CARTESIAN_POINT('Ctrl Pts',(41.7562341395977,-11.7410945211992,0.));
#19622=CARTESIAN_POINT('Ctrl Pts',(41.8282796562569,-11.81512813804,0.));
#19623=CARTESIAN_POINT('Ctrl Pts',(41.9000638152266,-11.8895948153349,0.));
#19624=CARTESIAN_POINT('Ctrl Pts',(41.9715865222182,-11.9644914999263,0.));
#19625=CARTESIAN_POINT('Ctrl Pts',(42.0571002269437,-12.054880669507,0.));
#19626=CARTESIAN_POINT('Ctrl Pts',(42.1280354231517,-12.1307372881904,0.));
#19627=CARTESIAN_POINT('Ctrl Pts',(42.18457517013,-12.1917619768791,0.));
#19628=CARTESIAN_POINT('Ctrl Pts',(42.2268628664988,-12.2377212115625,0.));
#19629=CARTESIAN_POINT('Ctrl Pts',(42.2550026135057,-12.2684454652018,0.));
#19630=CARTESIAN_POINT('',(42.2550026135057,-12.2684454652017,15.));
#19631=CARTESIAN_POINT('Ctrl Pts',(42.2550026135057,-12.2684454652018,15.));
#19632=CARTESIAN_POINT('Ctrl Pts',(42.2409327400055,-12.2530833383985,15.));
#19633=CARTESIAN_POINT('Ctrl Pts',(42.2127669677092,-12.222401466668,15.));
#19634=CARTESIAN_POINT('Ctrl Pts',(42.1704402333854,-12.1765058047069,15.));
#19635=CARTESIAN_POINT('Ctrl Pts',(42.1138483839101,-12.1155659644537,15.));
#19636=CARTESIAN_POINT('Ctrl Pts',(42.0428479428228,-12.0398158079102,15.));
#19637=CARTESIAN_POINT('Ctrl Pts',(41.9715865222182,-11.9644914999263,15.));
#19638=CARTESIAN_POINT('Ctrl Pts',(41.9000638152266,-11.8895948153349,15.));
#19639=CARTESIAN_POINT('Ctrl Pts',(41.8282796562569,-11.81512813804,15.));
#19640=CARTESIAN_POINT('Ctrl Pts',(41.7562341395977,-11.7410945211992,15.));
#19641=CARTESIAN_POINT('Ctrl Pts',(41.6839275596248,-11.6674975352852,15.));
#19642=CARTESIAN_POINT('Ctrl Pts',(41.6113603270596,-11.5943410868252,15.));
#19643=CARTESIAN_POINT('Ctrl Pts',(41.5385328935506,-11.5216292382388,15.));
#19644=CARTESIAN_POINT('Ctrl Pts',(41.4654456796071,-11.449366039385,15.));
#19645=CARTESIAN_POINT('Ctrl Pts',(41.3920989905986,-11.3775553120177,15.));
#19646=CARTESIAN_POINT('Ctrl Pts',(41.3184930194148,-11.3062006993745,15.));
#19647=CARTESIAN_POINT('Ctrl Pts',(41.2446278781981,-11.2353057980338,15.));
#19648=CARTESIAN_POINT('Ctrl Pts',(41.1705036228854,-11.1648742640378,15.));
#19649=CARTESIAN_POINT('Ctrl Pts',(41.0961202807715,-11.0949099155251,15.));
#19650=CARTESIAN_POINT('Ctrl Pts',(41.0214778832142,-11.0254168609972,15.));
#19651=CARTESIAN_POINT('Ctrl Pts',(40.9465764747798,-10.956399476781,15.));
#19652=CARTESIAN_POINT('Ctrl Pts',(40.8714161092412,-10.8878623066647,15.));
#19653=CARTESIAN_POINT('Ctrl Pts',(40.7959968527561,-10.8198099757795,15.));
#19654=CARTESIAN_POINT('Ctrl Pts',(40.7203187831783,-10.7522471109694,15.));
#19655=CARTESIAN_POINT('Ctrl Pts',(40.6443819999244,-10.6851782157325,15.));
#19656=CARTESIAN_POINT('Ctrl Pts',(40.5681866012103,-10.618607730849,15.));
#19657=CARTESIAN_POINT('Ctrl Pts',(40.4917326404439,-10.5525402237951,15.));
#19658=CARTESIAN_POINT('Ctrl Pts',(40.4150200869536,-10.48698054978,15.));
#19659=CARTESIAN_POINT('Ctrl Pts',(40.3380487942952,-10.4219339932951,15.));
#19660=CARTESIAN_POINT('Ctrl Pts',(40.2608184485326,-10.3574064830678,15.));
#19661=CARTESIAN_POINT('Ctrl Pts',(40.1833286010098,-10.2934044990237,15.));
#19662=CARTESIAN_POINT('Ctrl Pts',(40.1055787732578,-10.2299347125857,15.));
#19663=CARTESIAN_POINT('Ctrl Pts',(40.0275685525923,-10.1670036683795,15.));
#19664=CARTESIAN_POINT('Ctrl Pts',(39.9492976736738,-10.1046175096878,15.));
#19665=CARTESIAN_POINT('Ctrl Pts',(39.8707661565233,-10.0427815229883,15.));
#19666=CARTESIAN_POINT('Ctrl Pts',(39.7919742367922,-9.98150036150824,15.));
#19667=CARTESIAN_POINT('Ctrl Pts',(39.712922089547,-9.92077894513193,15.));
#19668=CARTESIAN_POINT('Ctrl Pts',(39.6336095893767,-9.86062324242561,15.));
#19669=CARTESIAN_POINT('Ctrl Pts',(39.5540361022309,-9.80104095251614,15.));
#19670=CARTESIAN_POINT('Ctrl Pts',(39.4742001555227,-9.74204258152664,15.));
#19671=CARTESIAN_POINT('Ctrl Pts',(39.3940995760289,-9.68364100883828,15.));
#19672=CARTESIAN_POINT('Ctrl Pts',(39.3137321153686,-9.62584947846544,15.));
#19673=CARTESIAN_POINT('Ctrl Pts',(39.2330959982788,-9.56867984233624,15.));
#19674=CARTESIAN_POINT('Ctrl Pts',(39.1521903958955,-9.51214104535621,15.));
#19675=CARTESIAN_POINT('Ctrl Pts',(39.0710161994951,-9.45623664577432,15.));
#19676=CARTESIAN_POINT('Ctrl Pts',(38.9895756526779,-9.40096600877644,15.));
#19677=CARTESIAN_POINT('Ctrl Pts',(38.9078708427078,-9.34632917154637,15.));
#19678=CARTESIAN_POINT('Ctrl Pts',(38.8259023794241,-9.29233110570904,15.));
#19679=CARTESIAN_POINT('Ctrl Pts',(38.7436682576832,-9.23898539199332,15.));
#19680=CARTESIAN_POINT('Ctrl Pts',(38.6611620045193,-9.1863201939433,15.));
#19681=CARTESIAN_POINT('Ctrl Pts',(38.5783736628826,-9.13437512010587,15.));
#19682=CARTESIAN_POINT('Ctrl Pts',(38.4952932486131,-9.08319014288087,15.));
#19683=CARTESIAN_POINT('Ctrl Pts',(38.4119138099805,-9.03279579360191,15.));
#19684=CARTESIAN_POINT('Ctrl Pts',(38.3282340281403,-8.98320483785761,15.));
#19685=CARTESIAN_POINT('Ctrl Pts',(38.2442625706309,-8.9343983099634,15.));
#19686=CARTESIAN_POINT('Ctrl Pts',(38.1600150482528,-8.88633535238435,15.));
#19687=CARTESIAN_POINT('Ctrl Pts',(38.0755058326913,-8.8389795976335,15.));
#19688=CARTESIAN_POINT('Ctrl Pts',(37.9907407304174,-8.79232279131093,15.));
#19689=CARTESIAN_POINT('Ctrl Pts',(37.9057107230066,-8.74640499479003,15.));
#19690=CARTESIAN_POINT('Ctrl Pts',(37.8203816669031,-8.70134776631144,15.));
#19691=CARTESIAN_POINT('Ctrl Pts',(37.7347032383719,-8.65732553894525,15.));
#19692=CARTESIAN_POINT('Ctrl Pts',(37.6486274754754,-8.61450621749156,15.));
#19693=CARTESIAN_POINT('Ctrl Pts',(37.5621256752108,-8.57299698459467,15.));
#19694=CARTESIAN_POINT('Ctrl Pts',(37.4752030152968,-8.53279758643785,15.));
#19695=CARTESIAN_POINT('Ctrl Pts',(37.3879218093514,-8.49372546467076,15.));
#19696=CARTESIAN_POINT('Ctrl Pts',(37.3003733151561,-8.45550849433961,15.));
#19697=CARTESIAN_POINT('Ctrl Pts',(37.2126332013933,-8.41793088313261,15.));
#19698=CARTESIAN_POINT('Ctrl Pts',(37.1247207489179,-8.38096706211449,15.));
#19699=CARTESIAN_POINT('Ctrl Pts',(37.0365602155148,-8.3449081895264,15.));
#19700=CARTESIAN_POINT('Ctrl Pts',(36.9479311729484,-8.31052547794592,15.));
#19701=CARTESIAN_POINT('Ctrl Pts',(36.8585291300917,-8.27886599440786,15.));
#19702=CARTESIAN_POINT('Ctrl Pts',(36.7861403757604,-8.25656657451821,15.));
#19703=CARTESIAN_POINT('Ctrl Pts',(36.7312504697652,-8.24192165947368,15.));
#19704=CARTESIAN_POINT('Ctrl Pts',(36.6943771018148,-8.23313075335377,15.));
#19705=CARTESIAN_POINT('Ctrl Pts',(36.6758703925241,-8.22897839625062,15.));
#19706=CARTESIAN_POINT('',(42.2550026135057,-12.2684454652017,0.));
#19707=CARTESIAN_POINT('Origin',(1.07784724682657E-11,-3.50213800024364E-12,
0.));
#19708=CARTESIAN_POINT('',(41.396226524684,-14.911486495888,0.));
#19709=CARTESIAN_POINT('Origin',(1.07784724682657E-11,-3.50213800024364E-12,
0.));
#19710=CARTESIAN_POINT('',(41.396226524684,-14.911486495888,15.));
#19711=CARTESIAN_POINT('Origin',(1.07784724682657E-11,-3.50213800024364E-12,
15.));
#19712=CARTESIAN_POINT('',(41.396226524684,-14.911486495888,0.));
#19713=CARTESIAN_POINT('Ctrl Pts',(34.5082745737944,-14.9001523628048,0.));
#19714=CARTESIAN_POINT('Ctrl Pts',(34.5082745737944,-14.9001523628048,18.));
#19715=CARTESIAN_POINT('Ctrl Pts',(34.525687510388,-14.9076710061311,0.));
#19716=CARTESIAN_POINT('Ctrl Pts',(34.525687510388,-14.9076710061311,18.));
#19717=CARTESIAN_POINT('Ctrl Pts',(34.5606858566713,-14.9222326355678,0.));
#19718=CARTESIAN_POINT('Ctrl Pts',(34.5606858566713,-14.9222326355678,18.));
#19719=CARTESIAN_POINT('Ctrl Pts',(34.6137007885254,-14.9426481276593,0.));
#19720=CARTESIAN_POINT('Ctrl Pts',(34.6137007885254,-14.9426481276593,18.));
#19721=CARTESIAN_POINT('Ctrl Pts',(34.6853717911268,-14.9671565602316,0.));
#19722=CARTESIAN_POINT('Ctrl Pts',(34.6853717911268,-14.9671565602316,18.));
#19723=CARTESIAN_POINT('Ctrl Pts',(34.7763085406486,-14.9940927023322,0.));
#19724=CARTESIAN_POINT('Ctrl Pts',(34.7763085406486,-14.9940927023322,18.));
#19725=CARTESIAN_POINT('Ctrl Pts',(34.8682205930809,-15.0183713484962,0.));
#19726=CARTESIAN_POINT('Ctrl Pts',(34.8682205930809,-15.0183713484962,18.));
#19727=CARTESIAN_POINT('Ctrl Pts',(34.9607388363587,-15.041018569143,0.));
#19728=CARTESIAN_POINT('Ctrl Pts',(34.9607388363587,-15.041018569143,18.));
#19729=CARTESIAN_POINT('Ctrl Pts',(35.0535882932913,-15.0627878528202,0.));
#19730=CARTESIAN_POINT('Ctrl Pts',(35.0535882932913,-15.0627878528202,18.));
#19731=CARTESIAN_POINT('Ctrl Pts',(35.1466591020976,-15.08395927165,0.));
#19732=CARTESIAN_POINT('Ctrl Pts',(35.1466591020976,-15.08395927165,18.));
#19733=CARTESIAN_POINT('Ctrl Pts',(35.2399506932815,-15.104500806927,0.));
#19734=CARTESIAN_POINT('Ctrl Pts',(35.2399506932815,-15.104500806927,18.));
#19735=CARTESIAN_POINT('Ctrl Pts',(35.3335286891314,-15.1241934020682,0.));
#19736=CARTESIAN_POINT('Ctrl Pts',(35.3335286891314,-15.1241934020682,18.));
#19737=CARTESIAN_POINT('Ctrl Pts',(35.4274792115856,-15.1427632633831,0.));
#19738=CARTESIAN_POINT('Ctrl Pts',(35.4274792115856,-15.1427632633831,18.));
#19739=CARTESIAN_POINT('Ctrl Pts',(35.5218591529745,-15.1600260710384,0.));
#19740=CARTESIAN_POINT('Ctrl Pts',(35.5218591529745,-15.1600260710384,18.));
#19741=CARTESIAN_POINT('Ctrl Pts',(35.6166644736253,-15.1759785763051,0.));
#19742=CARTESIAN_POINT('Ctrl Pts',(35.6166644736253,-15.1759785763051,18.));
#19743=CARTESIAN_POINT('Ctrl Pts',(35.7118553943773,-15.1907243629659,0.));
#19744=CARTESIAN_POINT('Ctrl Pts',(35.7118553943773,-15.1907243629659,18.));
#19745=CARTESIAN_POINT('Ctrl Pts',(35.8073720252878,-15.2044274601769,0.));
#19746=CARTESIAN_POINT('Ctrl Pts',(35.8073720252878,-15.2044274601769,18.));
#19747=CARTESIAN_POINT('Ctrl Pts',(35.9031525499277,-15.2172585668056,0.));
#19748=CARTESIAN_POINT('Ctrl Pts',(35.9031525499277,-15.2172585668056,18.));
#19749=CARTESIAN_POINT('Ctrl Pts',(35.9991531408727,-15.2293360946131,0.));
#19750=CARTESIAN_POINT('Ctrl Pts',(35.9991531408727,-15.2293360946131,18.));
#19751=CARTESIAN_POINT('Ctrl Pts',(36.095357546697,-15.240697754828,0.));
#19752=CARTESIAN_POINT('Ctrl Pts',(36.095357546697,-15.240697754828,18.));
#19753=CARTESIAN_POINT('Ctrl Pts',(36.1917659216814,-15.2513334565427,0.));
#19754=CARTESIAN_POINT('Ctrl Pts',(36.1917659216814,-15.2513334565427,18.));
#19755=CARTESIAN_POINT('Ctrl Pts',(36.2883880151607,-15.2612053303774,0.));
#19756=CARTESIAN_POINT('Ctrl Pts',(36.2883880151607,-15.2612053303774,18.));
#19757=CARTESIAN_POINT('Ctrl Pts',(36.3852352131887,-15.2702711460937,0.));
#19758=CARTESIAN_POINT('Ctrl Pts',(36.3852352131887,-15.2702711460937,18.));
#19759=CARTESIAN_POINT('Ctrl Pts',(36.4823116513289,-15.2785104654792,0.));
#19760=CARTESIAN_POINT('Ctrl Pts',(36.4823116513289,-15.2785104654792,18.));
#19761=CARTESIAN_POINT('Ctrl Pts',(36.5796108931244,-15.2859343913094,0.));
#19762=CARTESIAN_POINT('Ctrl Pts',(36.5796108931244,-15.2859343913094,18.));
#19763=CARTESIAN_POINT('Ctrl Pts',(36.6771206167755,-15.2925717100767,0.));
#19764=CARTESIAN_POINT('Ctrl Pts',(36.6771206167755,-15.2925717100767,18.));
#19765=CARTESIAN_POINT('Ctrl Pts',(36.7748254044502,-15.2984606286738,0.));
#19766=CARTESIAN_POINT('Ctrl Pts',(36.7748254044502,-15.2984606286738,18.));
#19767=CARTESIAN_POINT('Ctrl Pts',(36.8727100302512,-15.3036390436952,0.));
#19768=CARTESIAN_POINT('Ctrl Pts',(36.8727100302512,-15.3036390436952,18.));
#19769=CARTESIAN_POINT('Ctrl Pts',(36.970763176802,-15.3081335446406,0.));
#19770=CARTESIAN_POINT('Ctrl Pts',(36.970763176802,-15.3081335446406,18.));
#19771=CARTESIAN_POINT('Ctrl Pts',(37.0689784837457,-15.3119562971444,0.));
#19772=CARTESIAN_POINT('Ctrl Pts',(37.0689784837457,-15.3119562971444,18.));
#19773=CARTESIAN_POINT('Ctrl Pts',(37.1673525354641,-15.3151109648809,0.));
#19774=CARTESIAN_POINT('Ctrl Pts',(37.1673525354641,-15.3151109648809,18.));
#19775=CARTESIAN_POINT('Ctrl Pts',(37.2658836214694,-15.3175963510698,0.));
#19776=CARTESIAN_POINT('Ctrl Pts',(37.2658836214694,-15.3175963510698,18.));
#19777=CARTESIAN_POINT('Ctrl Pts',(37.3645702997848,-15.3194106233802,0.));
#19778=CARTESIAN_POINT('Ctrl Pts',(37.3645702997848,-15.3194106233802,18.));
#19779=CARTESIAN_POINT('Ctrl Pts',(37.4634097578665,-15.3205561366169,0.));
#19780=CARTESIAN_POINT('Ctrl Pts',(37.4634097578665,-15.3205561366169,18.));
#19781=CARTESIAN_POINT('Ctrl Pts',(37.562397408596,-15.3210406145546,0.));
#19782=CARTESIAN_POINT('Ctrl Pts',(37.562397408596,-15.3210406145546,18.));
#19783=CARTESIAN_POINT('Ctrl Pts',(37.6615277218027,-15.3208746890781,0.));
#19784=CARTESIAN_POINT('Ctrl Pts',(37.6615277218027,-15.3208746890781,18.));
#19785=CARTESIAN_POINT('Ctrl Pts',(37.7607947318286,-15.320070396385,0.));
#19786=CARTESIAN_POINT('Ctrl Pts',(37.7607947318286,-15.320070396385,18.));
#19787=CARTESIAN_POINT('Ctrl Pts',(37.8601926265378,-15.3186394335023,0.));
#19788=CARTESIAN_POINT('Ctrl Pts',(37.8601926265378,-15.3186394335023,18.));
#19789=CARTESIAN_POINT('Ctrl Pts',(37.959716421934,-15.3165911656268,0.));
#19790=CARTESIAN_POINT('Ctrl Pts',(37.959716421934,-15.3165911656268,18.));
#19791=CARTESIAN_POINT('Ctrl Pts',(38.0593621055415,-15.3139321941687,0.));
#19792=CARTESIAN_POINT('Ctrl Pts',(38.0593621055415,-15.3139321941687,18.));
#19793=CARTESIAN_POINT('Ctrl Pts',(38.1591262705847,-15.310667421514,0.));
#19794=CARTESIAN_POINT('Ctrl Pts',(38.1591262705847,-15.310667421514,18.));
#19795=CARTESIAN_POINT('Ctrl Pts',(38.2590058835965,-15.3068007250314,0.));
#19796=CARTESIAN_POINT('Ctrl Pts',(38.2590058835965,-15.3068007250314,18.));
#19797=CARTESIAN_POINT('Ctrl Pts',(38.3589980188324,-15.3023357307483,0.));
#19798=CARTESIAN_POINT('Ctrl Pts',(38.3589980188324,-15.3023357307483,18.));
#19799=CARTESIAN_POINT('Ctrl Pts',(38.4590995527814,-15.297276703747,0.));
#19800=CARTESIAN_POINT('Ctrl Pts',(38.4590995527814,-15.297276703747,18.));
#19801=CARTESIAN_POINT('Ctrl Pts',(38.5593070891769,-15.2916287700102,0.));
#19802=CARTESIAN_POINT('Ctrl Pts',(38.5593070891769,-15.2916287700102,18.));
#19803=CARTESIAN_POINT('Ctrl Pts',(38.659617115053,-15.2853974668211,0.));
#19804=CARTESIAN_POINT('Ctrl Pts',(38.659617115053,-15.2853974668211,18.));
#19805=CARTESIAN_POINT('Ctrl Pts',(38.7600260961351,-15.2785884727112,0.));
#19806=CARTESIAN_POINT('Ctrl Pts',(38.7600260961351,-15.2785884727112,18.));
#19807=CARTESIAN_POINT('Ctrl Pts',(38.860530586589,-15.2712072937639,0.));
#19808=CARTESIAN_POINT('Ctrl Pts',(38.860530586589,-15.2712072937639,18.));
#19809=CARTESIAN_POINT('Ctrl Pts',(38.9611273555758,-15.2632589109473,0.));
#19810=CARTESIAN_POINT('Ctrl Pts',(38.9611273555758,-15.2632589109473,18.));
#19811=CARTESIAN_POINT('Ctrl Pts',(39.061813415425,-15.2547476855825,0.));
#19812=CARTESIAN_POINT('Ctrl Pts',(39.061813415425,-15.2547476855825,18.));
#19813=CARTESIAN_POINT('Ctrl Pts',(39.1625859371304,-15.2456775636447,0.));
#19814=CARTESIAN_POINT('Ctrl Pts',(39.1625859371304,-15.2456775636447,18.));
#19815=CARTESIAN_POINT('Ctrl Pts',(39.2634421927888,-15.2360522089072,0.));
#19816=CARTESIAN_POINT('Ctrl Pts',(39.2634421927888,-15.2360522089072,18.));
#19817=CARTESIAN_POINT('Ctrl Pts',(39.3643794927167,-15.225875156307,0.));
#19818=CARTESIAN_POINT('Ctrl Pts',(39.3643794927167,-15.225875156307,18.));
#19819=CARTESIAN_POINT('Ctrl Pts',(39.4653951093947,-15.2151499908149,0.));
#19820=CARTESIAN_POINT('Ctrl Pts',(39.4653951093947,-15.2151499908149,18.));
#19821=CARTESIAN_POINT('Ctrl Pts',(39.5664862602472,-15.2038804098649,0.));
#19822=CARTESIAN_POINT('Ctrl Pts',(39.5664862602472,-15.2038804098649,18.));
#19823=CARTESIAN_POINT('Ctrl Pts',(39.6676501731673,-15.1920701163804,0.));
#19824=CARTESIAN_POINT('Ctrl Pts',(39.6676501731673,-15.1920701163804,18.));
#19825=CARTESIAN_POINT('Ctrl Pts',(39.7688841338802,-15.1797227547562,0.));
#19826=CARTESIAN_POINT('Ctrl Pts',(39.7688841338802,-15.1797227547562,18.));
#19827=CARTESIAN_POINT('Ctrl Pts',(39.8701855339908,-15.1668418393198,0.));
#19828=CARTESIAN_POINT('Ctrl Pts',(39.8701855339908,-15.1668418393198,18.));
#19829=CARTESIAN_POINT('Ctrl Pts',(39.9715519332134,-15.1534306754871,0.));
#19830=CARTESIAN_POINT('Ctrl Pts',(39.9715519332134,-15.1534306754871,18.));
#19831=CARTESIAN_POINT('Ctrl Pts',(40.0729810652204,-15.1394923361537,0.));
#19832=CARTESIAN_POINT('Ctrl Pts',(40.0729810652204,-15.1394923361537,18.));
#19833=CARTESIAN_POINT('Ctrl Pts',(40.1744707357902,-15.1250297462408,0.));
#19834=CARTESIAN_POINT('Ctrl Pts',(40.1744707357902,-15.1250297462408,18.));
#19835=CARTESIAN_POINT('Ctrl Pts',(40.2760187401821,-15.1100457495259,0.));
#19836=CARTESIAN_POINT('Ctrl Pts',(40.2760187401821,-15.1100457495259,18.));
#19837=CARTESIAN_POINT('Ctrl Pts',(40.3776227809037,-15.0945431800724,0.));
#19838=CARTESIAN_POINT('Ctrl Pts',(40.3776227809037,-15.0945431800724,18.));
#19839=CARTESIAN_POINT('Ctrl Pts',(40.4792803645352,-15.0785249502524,0.));
#19840=CARTESIAN_POINT('Ctrl Pts',(40.4792803645352,-15.0785249502524,18.));
#19841=CARTESIAN_POINT('Ctrl Pts',(40.58098877043,-15.0619940893017,0.));
#19842=CARTESIAN_POINT('Ctrl Pts',(40.58098877043,-15.0619940893017,18.));
#19843=CARTESIAN_POINT('Ctrl Pts',(40.6827452453667,-15.0449536183143,0.));
#19844=CARTESIAN_POINT('Ctrl Pts',(40.6827452453667,-15.0449536183143,18.));
#19845=CARTESIAN_POINT('Ctrl Pts',(40.7845471608654,-15.0274064563211,0.));
#19846=CARTESIAN_POINT('Ctrl Pts',(40.7845471608654,-15.0274064563211,18.));
#19847=CARTESIAN_POINT('Ctrl Pts',(40.8863921801,-15.0093553188655,0.));
#19848=CARTESIAN_POINT('Ctrl Pts',(40.8863921801,-15.0093553188655,18.));
#19849=CARTESIAN_POINT('Ctrl Pts',(40.9882784321884,-14.9908026205824,0.));
#19850=CARTESIAN_POINT('Ctrl Pts',(40.9882784321884,-14.9908026205824,18.));
#19851=CARTESIAN_POINT('Ctrl Pts',(41.0902046498729,-14.9717503874227,0.));
#19852=CARTESIAN_POINT('Ctrl Pts',(41.0902046498729,-14.9717503874227,18.));
#19853=CARTESIAN_POINT('Ctrl Pts',(41.1921700381957,-14.9522002356298,0.));
#19854=CARTESIAN_POINT('Ctrl Pts',(41.1921700381957,-14.9522002356298,18.));
#19855=CARTESIAN_POINT('Ctrl Pts',(41.2737733455422,-14.936162723752,0.));
#19856=CARTESIAN_POINT('Ctrl Pts',(41.2737733455422,-14.936162723752,18.));
#19857=CARTESIAN_POINT('Ctrl Pts',(41.3349931861715,-14.9239113834707,0.));
#19858=CARTESIAN_POINT('Ctrl Pts',(41.3349931861715,-14.9239113834707,18.));
#19859=CARTESIAN_POINT('Ctrl Pts',(41.3758141263348,-14.9156446533966,0.));
#19860=CARTESIAN_POINT('Ctrl Pts',(41.3758141263348,-14.9156446533966,18.));
#19861=CARTESIAN_POINT('Ctrl Pts',(41.396226524684,-14.911486495888,0.));
#19862=CARTESIAN_POINT('Ctrl Pts',(41.396226524684,-14.911486495888,18.));
#19863=CARTESIAN_POINT('Ctrl Pts',(34.5082745737944,-14.9001523628048,0.));
#19864=CARTESIAN_POINT('Ctrl Pts',(34.525687510388,-14.9076710061311,0.));
#19865=CARTESIAN_POINT('Ctrl Pts',(34.5606858566713,-14.9222326355678,0.));
#19866=CARTESIAN_POINT('Ctrl Pts',(34.6137007885254,-14.9426481276593,0.));
#19867=CARTESIAN_POINT('Ctrl Pts',(34.6853717911268,-14.9671565602316,0.));
#19868=CARTESIAN_POINT('Ctrl Pts',(34.7763085406486,-14.9940927023322,0.));
#19869=CARTESIAN_POINT('Ctrl Pts',(34.8682205930809,-15.0183713484962,0.));
#19870=CARTESIAN_POINT('Ctrl Pts',(34.9607388363587,-15.041018569143,0.));
#19871=CARTESIAN_POINT('Ctrl Pts',(35.0535882932913,-15.0627878528202,0.));
#19872=CARTESIAN_POINT('Ctrl Pts',(35.1466591020976,-15.08395927165,0.));
#19873=CARTESIAN_POINT('Ctrl Pts',(35.2399506932815,-15.104500806927,0.));
#19874=CARTESIAN_POINT('Ctrl Pts',(35.3335286891314,-15.1241934020682,0.));
#19875=CARTESIAN_POINT('Ctrl Pts',(35.4274792115856,-15.1427632633831,0.));
#19876=CARTESIAN_POINT('Ctrl Pts',(35.5218591529745,-15.1600260710384,0.));
#19877=CARTESIAN_POINT('Ctrl Pts',(35.6166644736253,-15.1759785763051,0.));
#19878=CARTESIAN_POINT('Ctrl Pts',(35.7118553943773,-15.1907243629659,0.));
#19879=CARTESIAN_POINT('Ctrl Pts',(35.8073720252878,-15.2044274601769,0.));
#19880=CARTESIAN_POINT('Ctrl Pts',(35.9031525499277,-15.2172585668056,0.));
#19881=CARTESIAN_POINT('Ctrl Pts',(35.9991531408727,-15.2293360946131,0.));
#19882=CARTESIAN_POINT('Ctrl Pts',(36.095357546697,-15.240697754828,0.));
#19883=CARTESIAN_POINT('Ctrl Pts',(36.1917659216814,-15.2513334565427,0.));
#19884=CARTESIAN_POINT('Ctrl Pts',(36.2883880151607,-15.2612053303774,0.));
#19885=CARTESIAN_POINT('Ctrl Pts',(36.3852352131887,-15.2702711460937,0.));
#19886=CARTESIAN_POINT('Ctrl Pts',(36.4823116513289,-15.2785104654792,0.));
#19887=CARTESIAN_POINT('Ctrl Pts',(36.5796108931244,-15.2859343913094,0.));
#19888=CARTESIAN_POINT('Ctrl Pts',(36.6771206167755,-15.2925717100767,0.));
#19889=CARTESIAN_POINT('Ctrl Pts',(36.7748254044502,-15.2984606286738,0.));
#19890=CARTESIAN_POINT('Ctrl Pts',(36.8727100302512,-15.3036390436952,0.));
#19891=CARTESIAN_POINT('Ctrl Pts',(36.970763176802,-15.3081335446406,0.));
#19892=CARTESIAN_POINT('Ctrl Pts',(37.0689784837457,-15.3119562971444,0.));
#19893=CARTESIAN_POINT('Ctrl Pts',(37.1673525354641,-15.3151109648809,0.));
#19894=CARTESIAN_POINT('Ctrl Pts',(37.2658836214694,-15.3175963510698,0.));
#19895=CARTESIAN_POINT('Ctrl Pts',(37.3645702997848,-15.3194106233802,0.));
#19896=CARTESIAN_POINT('Ctrl Pts',(37.4634097578665,-15.3205561366169,0.));
#19897=CARTESIAN_POINT('Ctrl Pts',(37.562397408596,-15.3210406145546,0.));
#19898=CARTESIAN_POINT('Ctrl Pts',(37.6615277218027,-15.3208746890781,0.));
#19899=CARTESIAN_POINT('Ctrl Pts',(37.7607947318286,-15.320070396385,0.));
#19900=CARTESIAN_POINT('Ctrl Pts',(37.8601926265378,-15.3186394335023,0.));
#19901=CARTESIAN_POINT('Ctrl Pts',(37.959716421934,-15.3165911656268,0.));
#19902=CARTESIAN_POINT('Ctrl Pts',(38.0593621055415,-15.3139321941687,0.));
#19903=CARTESIAN_POINT('Ctrl Pts',(38.1591262705847,-15.310667421514,0.));
#19904=CARTESIAN_POINT('Ctrl Pts',(38.2590058835965,-15.3068007250314,0.));
#19905=CARTESIAN_POINT('Ctrl Pts',(38.3589980188324,-15.3023357307483,0.));
#19906=CARTESIAN_POINT('Ctrl Pts',(38.4590995527814,-15.297276703747,0.));
#19907=CARTESIAN_POINT('Ctrl Pts',(38.5593070891769,-15.2916287700102,0.));
#19908=CARTESIAN_POINT('Ctrl Pts',(38.659617115053,-15.2853974668211,0.));
#19909=CARTESIAN_POINT('Ctrl Pts',(38.7600260961351,-15.2785884727112,0.));
#19910=CARTESIAN_POINT('Ctrl Pts',(38.860530586589,-15.2712072937639,0.));
#19911=CARTESIAN_POINT('Ctrl Pts',(38.9611273555758,-15.2632589109473,0.));
#19912=CARTESIAN_POINT('Ctrl Pts',(39.061813415425,-15.2547476855825,0.));
#19913=CARTESIAN_POINT('Ctrl Pts',(39.1625859371304,-15.2456775636447,0.));
#19914=CARTESIAN_POINT('Ctrl Pts',(39.2634421927888,-15.2360522089072,0.));
#19915=CARTESIAN_POINT('Ctrl Pts',(39.3643794927167,-15.225875156307,0.));
#19916=CARTESIAN_POINT('Ctrl Pts',(39.4653951093947,-15.2151499908149,0.));
#19917=CARTESIAN_POINT('Ctrl Pts',(39.5664862602472,-15.2038804098649,0.));
#19918=CARTESIAN_POINT('Ctrl Pts',(39.6676501731673,-15.1920701163804,0.));
#19919=CARTESIAN_POINT('Ctrl Pts',(39.7688841338802,-15.1797227547562,0.));
#19920=CARTESIAN_POINT('Ctrl Pts',(39.8701855339908,-15.1668418393198,0.));
#19921=CARTESIAN_POINT('Ctrl Pts',(39.9715519332134,-15.1534306754871,0.));
#19922=CARTESIAN_POINT('Ctrl Pts',(40.0729810652204,-15.1394923361537,0.));
#19923=CARTESIAN_POINT('Ctrl Pts',(40.1744707357902,-15.1250297462408,0.));
#19924=CARTESIAN_POINT('Ctrl Pts',(40.2760187401821,-15.1100457495259,0.));
#19925=CARTESIAN_POINT('Ctrl Pts',(40.3776227809037,-15.0945431800724,0.));
#19926=CARTESIAN_POINT('Ctrl Pts',(40.4792803645352,-15.0785249502524,0.));
#19927=CARTESIAN_POINT('Ctrl Pts',(40.58098877043,-15.0619940893017,0.));
#19928=CARTESIAN_POINT('Ctrl Pts',(40.6827452453667,-15.0449536183143,0.));
#19929=CARTESIAN_POINT('Ctrl Pts',(40.7845471608654,-15.0274064563211,0.));
#19930=CARTESIAN_POINT('Ctrl Pts',(40.8863921801,-15.0093553188655,0.));
#19931=CARTESIAN_POINT('Ctrl Pts',(40.9882784321884,-14.9908026205824,0.));
#19932=CARTESIAN_POINT('Ctrl Pts',(41.1105898934098,-14.9679399407908,0.));
#19933=CARTESIAN_POINT('Ctrl Pts',(41.2125650743922,-14.9482653093396,0.));
#19934=CARTESIAN_POINT('Ctrl Pts',(41.2941761025922,-14.9321285285561,0.));
#19935=CARTESIAN_POINT('Ctrl Pts',(41.3554017279611,-14.919802810928,0.));
#19936=CARTESIAN_POINT('Ctrl Pts',(41.396226524684,-14.911486495888,0.));
#19937=CARTESIAN_POINT('Ctrl Pts',(34.5082745737944,-14.9001523628048,15.));
#19938=CARTESIAN_POINT('Ctrl Pts',(34.525687510388,-14.9076710061311,15.));
#19939=CARTESIAN_POINT('Ctrl Pts',(34.5606858566713,-14.9222326355678,15.));
#19940=CARTESIAN_POINT('Ctrl Pts',(34.6137007885254,-14.9426481276593,15.));
#19941=CARTESIAN_POINT('Ctrl Pts',(34.6853717911268,-14.9671565602316,15.));
#19942=CARTESIAN_POINT('Ctrl Pts',(34.7763085406486,-14.9940927023322,15.));
#19943=CARTESIAN_POINT('Ctrl Pts',(34.8682205930809,-15.0183713484962,15.));
#19944=CARTESIAN_POINT('Ctrl Pts',(34.9607388363587,-15.041018569143,15.));
#19945=CARTESIAN_POINT('Ctrl Pts',(35.0535882932913,-15.0627878528202,15.));
#19946=CARTESIAN_POINT('Ctrl Pts',(35.1466591020976,-15.08395927165,15.));
#19947=CARTESIAN_POINT('Ctrl Pts',(35.2399506932815,-15.104500806927,15.));
#19948=CARTESIAN_POINT('Ctrl Pts',(35.3335286891314,-15.1241934020682,15.));
#19949=CARTESIAN_POINT('Ctrl Pts',(35.4274792115856,-15.1427632633831,15.));
#19950=CARTESIAN_POINT('Ctrl Pts',(35.5218591529745,-15.1600260710384,15.));
#19951=CARTESIAN_POINT('Ctrl Pts',(35.6166644736253,-15.1759785763051,15.));
#19952=CARTESIAN_POINT('Ctrl Pts',(35.7118553943773,-15.1907243629659,15.));
#19953=CARTESIAN_POINT('Ctrl Pts',(35.8073720252878,-15.2044274601769,15.));
#19954=CARTESIAN_POINT('Ctrl Pts',(35.9031525499277,-15.2172585668056,15.));
#19955=CARTESIAN_POINT('Ctrl Pts',(35.9991531408727,-15.2293360946131,15.));
#19956=CARTESIAN_POINT('Ctrl Pts',(36.095357546697,-15.240697754828,15.));
#19957=CARTESIAN_POINT('Ctrl Pts',(36.1917659216814,-15.2513334565427,15.));
#19958=CARTESIAN_POINT('Ctrl Pts',(36.2883880151607,-15.2612053303774,15.));
#19959=CARTESIAN_POINT('Ctrl Pts',(36.3852352131887,-15.2702711460937,15.));
#19960=CARTESIAN_POINT('Ctrl Pts',(36.4823116513289,-15.2785104654792,15.));
#19961=CARTESIAN_POINT('Ctrl Pts',(36.5796108931244,-15.2859343913094,15.));
#19962=CARTESIAN_POINT('Ctrl Pts',(36.6771206167755,-15.2925717100767,15.));
#19963=CARTESIAN_POINT('Ctrl Pts',(36.7748254044502,-15.2984606286738,15.));
#19964=CARTESIAN_POINT('Ctrl Pts',(36.8727100302512,-15.3036390436952,15.));
#19965=CARTESIAN_POINT('Ctrl Pts',(36.970763176802,-15.3081335446406,15.));
#19966=CARTESIAN_POINT('Ctrl Pts',(37.0689784837457,-15.3119562971444,15.));
#19967=CARTESIAN_POINT('Ctrl Pts',(37.1673525354641,-15.3151109648809,15.));
#19968=CARTESIAN_POINT('Ctrl Pts',(37.2658836214694,-15.3175963510698,15.));
#19969=CARTESIAN_POINT('Ctrl Pts',(37.3645702997848,-15.3194106233802,15.));
#19970=CARTESIAN_POINT('Ctrl Pts',(37.4634097578665,-15.3205561366169,15.));
#19971=CARTESIAN_POINT('Ctrl Pts',(37.562397408596,-15.3210406145546,15.));
#19972=CARTESIAN_POINT('Ctrl Pts',(37.6615277218027,-15.3208746890781,15.));
#19973=CARTESIAN_POINT('Ctrl Pts',(37.7607947318286,-15.320070396385,15.));
#19974=CARTESIAN_POINT('Ctrl Pts',(37.8601926265378,-15.3186394335023,15.));
#19975=CARTESIAN_POINT('Ctrl Pts',(37.959716421934,-15.3165911656268,15.));
#19976=CARTESIAN_POINT('Ctrl Pts',(38.0593621055415,-15.3139321941687,15.));
#19977=CARTESIAN_POINT('Ctrl Pts',(38.1591262705847,-15.310667421514,15.));
#19978=CARTESIAN_POINT('Ctrl Pts',(38.2590058835965,-15.3068007250314,15.));
#19979=CARTESIAN_POINT('Ctrl Pts',(38.3589980188324,-15.3023357307483,15.));
#19980=CARTESIAN_POINT('Ctrl Pts',(38.4590995527814,-15.297276703747,15.));
#19981=CARTESIAN_POINT('Ctrl Pts',(38.5593070891769,-15.2916287700102,15.));
#19982=CARTESIAN_POINT('Ctrl Pts',(38.659617115053,-15.2853974668211,15.));
#19983=CARTESIAN_POINT('Ctrl Pts',(38.7600260961351,-15.2785884727112,15.));
#19984=CARTESIAN_POINT('Ctrl Pts',(38.860530586589,-15.2712072937639,15.));
#19985=CARTESIAN_POINT('Ctrl Pts',(38.9611273555758,-15.2632589109473,15.));
#19986=CARTESIAN_POINT('Ctrl Pts',(39.061813415425,-15.2547476855825,15.));
#19987=CARTESIAN_POINT('Ctrl Pts',(39.1625859371304,-15.2456775636447,15.));
#19988=CARTESIAN_POINT('Ctrl Pts',(39.2634421927888,-15.2360522089072,15.));
#19989=CARTESIAN_POINT('Ctrl Pts',(39.3643794927167,-15.225875156307,15.));
#19990=CARTESIAN_POINT('Ctrl Pts',(39.4653951093947,-15.2151499908149,15.));
#19991=CARTESIAN_POINT('Ctrl Pts',(39.5664862602472,-15.2038804098649,15.));
#19992=CARTESIAN_POINT('Ctrl Pts',(39.6676501731673,-15.1920701163804,15.));
#19993=CARTESIAN_POINT('Ctrl Pts',(39.7688841338802,-15.1797227547562,15.));
#19994=CARTESIAN_POINT('Ctrl Pts',(39.8701855339908,-15.1668418393198,15.));
#19995=CARTESIAN_POINT('Ctrl Pts',(39.9715519332134,-15.1534306754871,15.));
#19996=CARTESIAN_POINT('Ctrl Pts',(40.0729810652204,-15.1394923361537,15.));
#19997=CARTESIAN_POINT('Ctrl Pts',(40.1744707357902,-15.1250297462408,15.));
#19998=CARTESIAN_POINT('Ctrl Pts',(40.2760187401821,-15.1100457495259,15.));
#19999=CARTESIAN_POINT('Ctrl Pts',(40.3776227809037,-15.0945431800724,15.));
#20000=CARTESIAN_POINT('Ctrl Pts',(40.4792803645352,-15.0785249502524,15.));
#20001=CARTESIAN_POINT('Ctrl Pts',(40.58098877043,-15.0619940893017,15.));
#20002=CARTESIAN_POINT('Ctrl Pts',(40.6827452453667,-15.0449536183143,15.));
#20003=CARTESIAN_POINT('Ctrl Pts',(40.7845471608654,-15.0274064563211,15.));
#20004=CARTESIAN_POINT('Ctrl Pts',(40.8863921801,-15.0093553188655,15.));
#20005=CARTESIAN_POINT('Ctrl Pts',(40.9882784321884,-14.9908026205824,15.));
#20006=CARTESIAN_POINT('Ctrl Pts',(41.1105898934098,-14.9679399407908,15.));
#20007=CARTESIAN_POINT('Ctrl Pts',(41.2125650743922,-14.9482653093396,15.));
#20008=CARTESIAN_POINT('Ctrl Pts',(41.2941761025922,-14.9321285285561,15.));
#20009=CARTESIAN_POINT('Ctrl Pts',(41.3554017279611,-14.919802810928,15.));
#20010=CARTESIAN_POINT('Ctrl Pts',(41.396226524684,-14.911486495888,15.));
#20011=CARTESIAN_POINT('Ctrl Pts',(36.3957374383337,-24.725498909423,0.));
#20012=CARTESIAN_POINT('Ctrl Pts',(36.3957374383337,-24.725498909423,18.));
#20013=CARTESIAN_POINT('Ctrl Pts',(36.3871033517098,-24.7065408286023,0.));
#20014=CARTESIAN_POINT('Ctrl Pts',(36.3871033517098,-24.7065408286023,18.));
#20015=CARTESIAN_POINT('Ctrl Pts',(36.369797330215,-24.6686569322616,0.));
#20016=CARTESIAN_POINT('Ctrl Pts',(36.369797330215,-24.6686569322616,18.));
#20017=CARTESIAN_POINT('Ctrl Pts',(36.3437247532368,-24.6119278836614,0.));
#20018=CARTESIAN_POINT('Ctrl Pts',(36.3437247532368,-24.6119278836614,18.));
#20019=CARTESIAN_POINT('Ctrl Pts',(36.3087341522969,-24.5364828082556,0.));
#20020=CARTESIAN_POINT('Ctrl Pts',(36.3087341522969,-24.5364828082556,18.));
#20021=CARTESIAN_POINT('Ctrl Pts',(36.2646168058395,-24.4424997853605,0.));
#20022=CARTESIAN_POINT('Ctrl Pts',(36.2646168058395,-24.4424997853605,18.));
#20023=CARTESIAN_POINT('Ctrl Pts',(36.2201196586696,-24.3488411214068,0.));
#20024=CARTESIAN_POINT('Ctrl Pts',(36.2201196586696,-24.3488411214068,18.));
#20025=CARTESIAN_POINT('Ctrl Pts',(36.1752418704833,-24.2555084095332,0.));
#20026=CARTESIAN_POINT('Ctrl Pts',(36.1752418704833,-24.2555084095332,18.));
#20027=CARTESIAN_POINT('Ctrl Pts',(36.1299825471271,-24.1625038657964,0.));
#20028=CARTESIAN_POINT('Ctrl Pts',(36.1299825471271,-24.1625038657964,18.));
#20029=CARTESIAN_POINT('Ctrl Pts',(36.0843408347974,-24.0698304230588,0.));
#20030=CARTESIAN_POINT('Ctrl Pts',(36.0843408347974,-24.0698304230588,18.));
#20031=CARTESIAN_POINT('Ctrl Pts',(36.0383159101253,-23.9774915680089,0.));
#20032=CARTESIAN_POINT('Ctrl Pts',(36.0383159101253,-23.9774915680089,18.));
#20033=CARTESIAN_POINT('Ctrl Pts',(35.9919069565469,-23.8854911428947,0.));
#20034=CARTESIAN_POINT('Ctrl Pts',(35.9919069565469,-23.8854911428947,18.));
#20035=CARTESIAN_POINT('Ctrl Pts',(35.9451131482488,-23.7938331508737,0.));
#20036=CARTESIAN_POINT('Ctrl Pts',(35.9451131482488,-23.7938331508737,18.));
#20037=CARTESIAN_POINT('Ctrl Pts',(35.8979336336837,-23.7025215735353,0.));
#20038=CARTESIAN_POINT('Ctrl Pts',(35.8979336336837,-23.7025215735353,18.));
#20039=CARTESIAN_POINT('Ctrl Pts',(35.8503675222884,-23.611560139948,0.));
#20040=CARTESIAN_POINT('Ctrl Pts',(35.8503675222884,-23.611560139948,18.));
#20041=CARTESIAN_POINT('Ctrl Pts',(35.8024138716896,-23.5209523746427,0.));
#20042=CARTESIAN_POINT('Ctrl Pts',(35.8024138716896,-23.5209523746427,18.));
#20043=CARTESIAN_POINT('Ctrl Pts',(35.7540716771372,-23.4307017328227,0.));
#20044=CARTESIAN_POINT('Ctrl Pts',(35.7540716771372,-23.4307017328227,18.));
#20045=CARTESIAN_POINT('Ctrl Pts',(35.7053398620512,-23.3408117088762,0.));
#20046=CARTESIAN_POINT('Ctrl Pts',(35.7053398620512,-23.3408117088762,18.));
#20047=CARTESIAN_POINT('Ctrl Pts',(35.6562172725207,-23.2512859425032,0.));
#20048=CARTESIAN_POINT('Ctrl Pts',(35.6562172725207,-23.2512859425032,18.));
#20049=CARTESIAN_POINT('Ctrl Pts',(35.6067026687722,-23.1621283508111,0.));
#20050=CARTESIAN_POINT('Ctrl Pts',(35.6067026687722,-23.1621283508111,18.));
#20051=CARTESIAN_POINT('Ctrl Pts',(35.5567947408311,-23.0733431097058,0.));
#20052=CARTESIAN_POINT('Ctrl Pts',(35.5567947408311,-23.0733431097058,18.));
#20053=CARTESIAN_POINT('Ctrl Pts',(35.5064921357308,-22.9849345572033,0.));
#20054=CARTESIAN_POINT('Ctrl Pts',(35.5064921357308,-22.9849345572033,18.));
#20055=CARTESIAN_POINT('Ctrl Pts',(35.4557934871468,-22.8969071125089,0.));
#20056=CARTESIAN_POINT('Ctrl Pts',(35.4557934871468,-22.8969071125089,18.));
#20057=CARTESIAN_POINT('Ctrl Pts',(35.4046974393492,-22.8092652000707,0.));
#20058=CARTESIAN_POINT('Ctrl Pts',(35.4046974393492,-22.8092652000707,18.));
#20059=CARTESIAN_POINT('Ctrl Pts',(35.3532026952313,-22.7220131336913,0.));
#20060=CARTESIAN_POINT('Ctrl Pts',(35.3532026952313,-22.7220131336913,18.));
#20061=CARTESIAN_POINT('Ctrl Pts',(35.3013079759252,-22.635155167154,0.));
#20062=CARTESIAN_POINT('Ctrl Pts',(35.3013079759252,-22.635155167154,18.));
#20063=CARTESIAN_POINT('Ctrl Pts',(35.2490119207975,-22.548695660891,0.));
#20064=CARTESIAN_POINT('Ctrl Pts',(35.2490119207975,-22.548695660891,18.));
#20065=CARTESIAN_POINT('Ctrl Pts',(35.1963130003352,-22.4626392230023,0.));
#20066=CARTESIAN_POINT('Ctrl Pts',(35.1963130003352,-22.4626392230023,18.));
#20067=CARTESIAN_POINT('Ctrl Pts',(35.1432094422642,-22.3769908340843,0.));
#20068=CARTESIAN_POINT('Ctrl Pts',(35.1432094422642,-22.3769908340843,18.));
#20069=CARTESIAN_POINT('Ctrl Pts',(35.0896991159359,-22.2917560356803,0.));
#20070=CARTESIAN_POINT('Ctrl Pts',(35.0896991159359,-22.2917560356803,18.));
#20071=CARTESIAN_POINT('Ctrl Pts',(35.0357795922459,-22.2069408519233,0.));
#20072=CARTESIAN_POINT('Ctrl Pts',(35.0357795922459,-22.2069408519233,18.));
#20073=CARTESIAN_POINT('Ctrl Pts',(34.9814483545602,-22.1225514798584,0.));
#20074=CARTESIAN_POINT('Ctrl Pts',(34.9814483545602,-22.1225514798584,18.));
#20075=CARTESIAN_POINT('Ctrl Pts',(34.9267029879922,-22.0385940162683,0.));
#20076=CARTESIAN_POINT('Ctrl Pts',(34.9267029879922,-22.0385940162683,18.));
#20077=CARTESIAN_POINT('Ctrl Pts',(34.8715413418101,-21.9550742217675,0.));
#20078=CARTESIAN_POINT('Ctrl Pts',(34.8715413418101,-21.9550742217675,18.));
#20079=CARTESIAN_POINT('Ctrl Pts',(34.8159618014436,-21.8719971302818,0.));
#20080=CARTESIAN_POINT('Ctrl Pts',(34.8159618014436,-21.8719971302818,18.));
#20081=CARTESIAN_POINT('Ctrl Pts',(34.7599631530844,-21.7893672401137,0.));
#20082=CARTESIAN_POINT('Ctrl Pts',(34.7599631530844,-21.7893672401137,18.));
#20083=CARTESIAN_POINT('Ctrl Pts',(34.7035440429025,-21.7071892844497,0.));
#20084=CARTESIAN_POINT('Ctrl Pts',(34.7035440429025,-21.7071892844497,18.));
#20085=CARTESIAN_POINT('Ctrl Pts',(34.6467025072367,-21.6254689009796,0.));
#20086=CARTESIAN_POINT('Ctrl Pts',(34.6467025072367,-21.6254689009796,18.));
#20087=CARTESIAN_POINT('Ctrl Pts',(34.5894355639082,-21.5442132160757,0.));
#20088=CARTESIAN_POINT('Ctrl Pts',(34.5894355639082,-21.5442132160757,18.));
#20089=CARTESIAN_POINT('Ctrl Pts',(34.5317385658329,-21.4634317666005,0.));
#20090=CARTESIAN_POINT('Ctrl Pts',(34.5317385658329,-21.4634317666005,18.));
#20091=CARTESIAN_POINT('Ctrl Pts',(34.4736054662052,-21.3831361300104,0.));
#20092=CARTESIAN_POINT('Ctrl Pts',(34.4736054662052,-21.3831361300104,18.));
#20093=CARTESIAN_POINT('Ctrl Pts',(34.4150300340623,-21.3033382073239,0.));
#20094=CARTESIAN_POINT('Ctrl Pts',(34.4150300340623,-21.3033382073239,18.));
#20095=CARTESIAN_POINT('Ctrl Pts',(34.3560069185815,-21.2240487218079,0.));
#20096=CARTESIAN_POINT('Ctrl Pts',(34.3560069185815,-21.2240487218079,18.));
#20097=CARTESIAN_POINT('Ctrl Pts',(34.2965325673384,-21.14527592444,0.));
#20098=CARTESIAN_POINT('Ctrl Pts',(34.2965325673384,-21.14527592444,18.));
#20099=CARTESIAN_POINT('Ctrl Pts',(34.2366067284279,-21.0670234747355,0.));
#20100=CARTESIAN_POINT('Ctrl Pts',(34.2366067284279,-21.0670234747355,18.));
#20101=CARTESIAN_POINT('Ctrl Pts',(34.176231731809,-20.9892914622612,0.));
#20102=CARTESIAN_POINT('Ctrl Pts',(34.176231731809,-20.9892914622612,18.));
#20103=CARTESIAN_POINT('Ctrl Pts',(34.1154095510973,-20.9120805673809,0.));
#20104=CARTESIAN_POINT('Ctrl Pts',(34.1154095510973,-20.9120805673809,18.));
#20105=CARTESIAN_POINT('Ctrl Pts',(34.0541392299678,-20.8353957068415,0.));
#20106=CARTESIAN_POINT('Ctrl Pts',(34.0541392299678,-20.8353957068415,18.));
#20107=CARTESIAN_POINT('Ctrl Pts',(33.9924146647395,-20.7592491770603,0.));
#20108=CARTESIAN_POINT('Ctrl Pts',(33.9924146647395,-20.7592491770603,18.));
#20109=CARTESIAN_POINT('Ctrl Pts',(33.9302209962425,-20.683665762903,0.));
#20110=CARTESIAN_POINT('Ctrl Pts',(33.9302209962425,-20.683665762903,18.));
#20111=CARTESIAN_POINT('Ctrl Pts',(33.8675365150454,-20.6086800574386,0.));
#20112=CARTESIAN_POINT('Ctrl Pts',(33.8675365150454,-20.6086800574386,18.));
#20113=CARTESIAN_POINT('Ctrl Pts',(33.8043393734971,-20.5343269914034,0.));
#20114=CARTESIAN_POINT('Ctrl Pts',(33.8043393734971,-20.5343269914034,18.));
#20115=CARTESIAN_POINT('Ctrl Pts',(33.7406135254082,-20.4606334536183,0.));
#20116=CARTESIAN_POINT('Ctrl Pts',(33.7406135254082,-20.4606334536183,18.));
#20117=CARTESIAN_POINT('Ctrl Pts',(33.6763537716992,-20.3876111773341,0.));
#20118=CARTESIAN_POINT('Ctrl Pts',(33.6763537716992,-20.3876111773341,18.));
#20119=CARTESIAN_POINT('Ctrl Pts',(33.6115742164079,-20.3152448035298,0.));
#20120=CARTESIAN_POINT('Ctrl Pts',(33.6115742164079,-20.3152448035298,18.));
#20121=CARTESIAN_POINT('Ctrl Pts',(33.5463023319603,-20.243500298383,0.));
#20122=CARTESIAN_POINT('Ctrl Pts',(33.5463023319603,-20.243500298383,18.));
#20123=CARTESIAN_POINT('Ctrl Pts',(33.480563024813,-20.1723475154533,0.));
#20124=CARTESIAN_POINT('Ctrl Pts',(33.480563024813,-20.1723475154533,18.));
#20125=CARTESIAN_POINT('Ctrl Pts',(33.4143643679979,-20.1017803986381,0.));
#20126=CARTESIAN_POINT('Ctrl Pts',(33.4143643679979,-20.1017803986381,18.));
#20127=CARTESIAN_POINT('Ctrl Pts',(33.3476854048385,-20.0318342617213,0.));
#20128=CARTESIAN_POINT('Ctrl Pts',(33.3476854048385,-20.0318342617213,18.));
#20129=CARTESIAN_POINT('Ctrl Pts',(33.2804560993213,-19.9626141625206,0.));
#20130=CARTESIAN_POINT('Ctrl Pts',(33.2804560993213,-19.9626141625206,18.));
#20131=CARTESIAN_POINT('Ctrl Pts',(33.2125746879471,-19.8942704458546,0.));
#20132=CARTESIAN_POINT('Ctrl Pts',(33.2125746879471,-19.8942704458546,18.));
#20133=CARTESIAN_POINT('Ctrl Pts',(33.1439436707661,-19.8269479776239,0.));
#20134=CARTESIAN_POINT('Ctrl Pts',(33.1439436707661,-19.8269479776239,18.));
#20135=CARTESIAN_POINT('Ctrl Pts',(33.0745026283418,-19.7607398248651,0.));
#20136=CARTESIAN_POINT('Ctrl Pts',(33.0745026283418,-19.7607398248651,18.));
#20137=CARTESIAN_POINT('Ctrl Pts',(33.004256563411,-19.6956473461873,0.));
#20138=CARTESIAN_POINT('Ctrl Pts',(33.004256563411,-19.6956473461873,18.));
#20139=CARTESIAN_POINT('Ctrl Pts',(32.9333211533788,-19.6315161742485,0.));
#20140=CARTESIAN_POINT('Ctrl Pts',(32.9333211533788,-19.6315161742485,18.));
#20141=CARTESIAN_POINT('Ctrl Pts',(32.8618672807884,-19.5681157030437,0.));
#20142=CARTESIAN_POINT('Ctrl Pts',(32.8618672807884,-19.5681157030437,18.));
#20143=CARTESIAN_POINT('Ctrl Pts',(32.7900335943248,-19.5052640847974,0.));
#20144=CARTESIAN_POINT('Ctrl Pts',(32.7900335943248,-19.5052640847974,18.));
#20145=CARTESIAN_POINT('Ctrl Pts',(32.7178463324062,-19.4429429601189,0.));
#20146=CARTESIAN_POINT('Ctrl Pts',(32.7178463324062,-19.4429429601189,18.));
#20147=CARTESIAN_POINT('Ctrl Pts',(32.6451434870609,-19.381405831319,0.));
#20148=CARTESIAN_POINT('Ctrl Pts',(32.6451434870609,-19.381405831319,18.));
#20149=CARTESIAN_POINT('Ctrl Pts',(32.5714771007861,-19.3213180490743,0.));
#20150=CARTESIAN_POINT('Ctrl Pts',(32.5714771007861,-19.3213180490743,18.));
#20151=CARTESIAN_POINT('Ctrl Pts',(32.4962340238036,-19.2635813403783,0.));
#20152=CARTESIAN_POINT('Ctrl Pts',(32.4962340238036,-19.2635813403783,18.));
#20153=CARTESIAN_POINT('Ctrl Pts',(32.4342791270009,-19.2200039764927,0.));
#20154=CARTESIAN_POINT('Ctrl Pts',(32.4342791270009,-19.2200039764927,18.));
#20155=CARTESIAN_POINT('Ctrl Pts',(32.3866012518553,-19.1891139208368,0.));
#20156=CARTESIAN_POINT('Ctrl Pts',(32.3866012518553,-19.1891139208368,18.));
#20157=CARTESIAN_POINT('Ctrl Pts',(32.3542491343753,-19.1693587749508,0.));
#20158=CARTESIAN_POINT('Ctrl Pts',(32.3542491343753,-19.1693587749508,18.));
#20159=CARTESIAN_POINT('Ctrl Pts',(32.3379313568208,-19.1596907609891,0.));
#20160=CARTESIAN_POINT('Ctrl Pts',(32.3379313568208,-19.1596907609891,18.));
#20161=CARTESIAN_POINT('',(36.3957374383337,-24.7254989094229,0.));
#20162=CARTESIAN_POINT('Ctrl Pts',(32.3379313568208,-19.1596907609891,0.));
#20163=CARTESIAN_POINT('Ctrl Pts',(32.3542491343753,-19.1693587749508,0.));
#20164=CARTESIAN_POINT('Ctrl Pts',(32.3866012518553,-19.1891139208368,0.));
#20165=CARTESIAN_POINT('Ctrl Pts',(32.4342791270009,-19.2200039764927,0.));
#20166=CARTESIAN_POINT('Ctrl Pts',(32.4962340238036,-19.2635813403783,0.));
#20167=CARTESIAN_POINT('Ctrl Pts',(32.5714771007861,-19.3213180490743,0.));
#20168=CARTESIAN_POINT('Ctrl Pts',(32.6451434870609,-19.381405831319,0.));
#20169=CARTESIAN_POINT('Ctrl Pts',(32.7178463324062,-19.4429429601189,0.));
#20170=CARTESIAN_POINT('Ctrl Pts',(32.7900335943248,-19.5052640847974,0.));
#20171=CARTESIAN_POINT('Ctrl Pts',(32.8618672807884,-19.5681157030437,0.));
#20172=CARTESIAN_POINT('Ctrl Pts',(32.9333211533788,-19.6315161742485,0.));
#20173=CARTESIAN_POINT('Ctrl Pts',(33.004256563411,-19.6956473461873,0.));
#20174=CARTESIAN_POINT('Ctrl Pts',(33.0745026283418,-19.7607398248651,0.));
#20175=CARTESIAN_POINT('Ctrl Pts',(33.1439436707661,-19.8269479776239,0.));
#20176=CARTESIAN_POINT('Ctrl Pts',(33.2125746879471,-19.8942704458546,0.));
#20177=CARTESIAN_POINT('Ctrl Pts',(33.2804560993213,-19.9626141625206,0.));
#20178=CARTESIAN_POINT('Ctrl Pts',(33.3476854048385,-20.0318342617213,0.));
#20179=CARTESIAN_POINT('Ctrl Pts',(33.4143643679979,-20.1017803986381,0.));
#20180=CARTESIAN_POINT('Ctrl Pts',(33.480563024813,-20.1723475154533,0.));
#20181=CARTESIAN_POINT('Ctrl Pts',(33.5463023319603,-20.243500298383,0.));
#20182=CARTESIAN_POINT('Ctrl Pts',(33.6115742164079,-20.3152448035298,0.));
#20183=CARTESIAN_POINT('Ctrl Pts',(33.6763537716992,-20.3876111773341,0.));
#20184=CARTESIAN_POINT('Ctrl Pts',(33.7406135254082,-20.4606334536183,0.));
#20185=CARTESIAN_POINT('Ctrl Pts',(33.8043393734971,-20.5343269914034,0.));
#20186=CARTESIAN_POINT('Ctrl Pts',(33.8675365150454,-20.6086800574386,0.));
#20187=CARTESIAN_POINT('Ctrl Pts',(33.9302209962425,-20.683665762903,0.));
#20188=CARTESIAN_POINT('Ctrl Pts',(33.9924146647395,-20.7592491770603,0.));
#20189=CARTESIAN_POINT('Ctrl Pts',(34.0541392299678,-20.8353957068415,0.));
#20190=CARTESIAN_POINT('Ctrl Pts',(34.1154095510973,-20.9120805673809,0.));
#20191=CARTESIAN_POINT('Ctrl Pts',(34.176231731809,-20.9892914622612,0.));
#20192=CARTESIAN_POINT('Ctrl Pts',(34.2366067284279,-21.0670234747355,0.));
#20193=CARTESIAN_POINT('Ctrl Pts',(34.2965325673384,-21.14527592444,0.));
#20194=CARTESIAN_POINT('Ctrl Pts',(34.3560069185815,-21.2240487218079,0.));
#20195=CARTESIAN_POINT('Ctrl Pts',(34.4150300340623,-21.3033382073239,0.));
#20196=CARTESIAN_POINT('Ctrl Pts',(34.4736054662052,-21.3831361300104,0.));
#20197=CARTESIAN_POINT('Ctrl Pts',(34.5317385658329,-21.4634317666005,0.));
#20198=CARTESIAN_POINT('Ctrl Pts',(34.5894355639082,-21.5442132160757,0.));
#20199=CARTESIAN_POINT('Ctrl Pts',(34.6467025072367,-21.6254689009796,0.));
#20200=CARTESIAN_POINT('Ctrl Pts',(34.7035440429025,-21.7071892844497,0.));
#20201=CARTESIAN_POINT('Ctrl Pts',(34.7599631530844,-21.7893672401137,0.));
#20202=CARTESIAN_POINT('Ctrl Pts',(34.8159618014436,-21.8719971302818,0.));
#20203=CARTESIAN_POINT('Ctrl Pts',(34.8715413418101,-21.9550742217675,0.));
#20204=CARTESIAN_POINT('Ctrl Pts',(34.9267029879922,-22.0385940162683,0.));
#20205=CARTESIAN_POINT('Ctrl Pts',(34.9814483545602,-22.1225514798584,0.));
#20206=CARTESIAN_POINT('Ctrl Pts',(35.0357795922459,-22.2069408519233,0.));
#20207=CARTESIAN_POINT('Ctrl Pts',(35.0896991159359,-22.2917560356803,0.));
#20208=CARTESIAN_POINT('Ctrl Pts',(35.1432094422642,-22.3769908340843,0.));
#20209=CARTESIAN_POINT('Ctrl Pts',(35.1963130003352,-22.4626392230023,0.));
#20210=CARTESIAN_POINT('Ctrl Pts',(35.2490119207975,-22.548695660891,0.));
#20211=CARTESIAN_POINT('Ctrl Pts',(35.3013079759252,-22.635155167154,0.));
#20212=CARTESIAN_POINT('Ctrl Pts',(35.3532026952313,-22.7220131336913,0.));
#20213=CARTESIAN_POINT('Ctrl Pts',(35.4046974393492,-22.8092652000707,0.));
#20214=CARTESIAN_POINT('Ctrl Pts',(35.4557934871468,-22.8969071125089,0.));
#20215=CARTESIAN_POINT('Ctrl Pts',(35.5064921357308,-22.9849345572033,0.));
#20216=CARTESIAN_POINT('Ctrl Pts',(35.5567947408311,-23.0733431097058,0.));
#20217=CARTESIAN_POINT('Ctrl Pts',(35.6067026687722,-23.1621283508111,0.));
#20218=CARTESIAN_POINT('Ctrl Pts',(35.6562172725207,-23.2512859425032,0.));
#20219=CARTESIAN_POINT('Ctrl Pts',(35.7053398620512,-23.3408117088762,0.));
#20220=CARTESIAN_POINT('Ctrl Pts',(35.7540716771372,-23.4307017328227,0.));
#20221=CARTESIAN_POINT('Ctrl Pts',(35.8024138716896,-23.5209523746427,0.));
#20222=CARTESIAN_POINT('Ctrl Pts',(35.8503675222884,-23.611560139948,0.));
#20223=CARTESIAN_POINT('Ctrl Pts',(35.8979336336837,-23.7025215735353,0.));
#20224=CARTESIAN_POINT('Ctrl Pts',(35.9451131482488,-23.7938331508737,0.));
#20225=CARTESIAN_POINT('Ctrl Pts',(35.9919069565469,-23.8854911428947,0.));
#20226=CARTESIAN_POINT('Ctrl Pts',(36.0383159101253,-23.9774915680089,0.));
#20227=CARTESIAN_POINT('Ctrl Pts',(36.0843408347974,-24.0698304230588,0.));
#20228=CARTESIAN_POINT('Ctrl Pts',(36.1299825471271,-24.1625038657964,0.));
#20229=CARTESIAN_POINT('Ctrl Pts',(36.1752418704833,-24.2555084095332,0.));
#20230=CARTESIAN_POINT('Ctrl Pts',(36.2201196586696,-24.3488411214068,0.));
#20231=CARTESIAN_POINT('Ctrl Pts',(36.2735162352735,-24.4612315181512,0.));
#20232=CARTESIAN_POINT('Ctrl Pts',(36.3175386315528,-24.5552956307817,0.));
#20233=CARTESIAN_POINT('Ctrl Pts',(36.3524534604648,-24.630805301288,0.));
#20234=CARTESIAN_POINT('Ctrl Pts',(36.3784692650901,-24.6875827477484,0.));
#20235=CARTESIAN_POINT('Ctrl Pts',(36.3957374383337,-24.725498909423,0.));
#20236=CARTESIAN_POINT('',(36.3957374383337,-24.7254989094229,15.));
#20237=CARTESIAN_POINT('Ctrl Pts',(36.3957374383337,-24.725498909423,15.));
#20238=CARTESIAN_POINT('Ctrl Pts',(36.3871033517098,-24.7065408286023,15.));
#20239=CARTESIAN_POINT('Ctrl Pts',(36.369797330215,-24.6686569322616,15.));
#20240=CARTESIAN_POINT('Ctrl Pts',(36.3437247532368,-24.6119278836614,15.));
#20241=CARTESIAN_POINT('Ctrl Pts',(36.3087341522969,-24.5364828082556,15.));
#20242=CARTESIAN_POINT('Ctrl Pts',(36.2646168058395,-24.4424997853605,15.));
#20243=CARTESIAN_POINT('Ctrl Pts',(36.2201196586696,-24.3488411214068,15.));
#20244=CARTESIAN_POINT('Ctrl Pts',(36.1752418704833,-24.2555084095332,15.));
#20245=CARTESIAN_POINT('Ctrl Pts',(36.1299825471271,-24.1625038657964,15.));
#20246=CARTESIAN_POINT('Ctrl Pts',(36.0843408347974,-24.0698304230588,15.));
#20247=CARTESIAN_POINT('Ctrl Pts',(36.0383159101253,-23.9774915680089,15.));
#20248=CARTESIAN_POINT('Ctrl Pts',(35.9919069565469,-23.8854911428947,15.));
#20249=CARTESIAN_POINT('Ctrl Pts',(35.9451131482488,-23.7938331508737,15.));
#20250=CARTESIAN_POINT('Ctrl Pts',(35.8979336336837,-23.7025215735353,15.));
#20251=CARTESIAN_POINT('Ctrl Pts',(35.8503675222884,-23.611560139948,15.));
#20252=CARTESIAN_POINT('Ctrl Pts',(35.8024138716896,-23.5209523746427,15.));
#20253=CARTESIAN_POINT('Ctrl Pts',(35.7540716771372,-23.4307017328227,15.));
#20254=CARTESIAN_POINT('Ctrl Pts',(35.7053398620512,-23.3408117088762,15.));
#20255=CARTESIAN_POINT('Ctrl Pts',(35.6562172725207,-23.2512859425032,15.));
#20256=CARTESIAN_POINT('Ctrl Pts',(35.6067026687722,-23.1621283508111,15.));
#20257=CARTESIAN_POINT('Ctrl Pts',(35.5567947408311,-23.0733431097058,15.));
#20258=CARTESIAN_POINT('Ctrl Pts',(35.5064921357308,-22.9849345572033,15.));
#20259=CARTESIAN_POINT('Ctrl Pts',(35.4557934871468,-22.8969071125089,15.));
#20260=CARTESIAN_POINT('Ctrl Pts',(35.4046974393492,-22.8092652000707,15.));
#20261=CARTESIAN_POINT('Ctrl Pts',(35.3532026952313,-22.7220131336913,15.));
#20262=CARTESIAN_POINT('Ctrl Pts',(35.3013079759252,-22.635155167154,15.));
#20263=CARTESIAN_POINT('Ctrl Pts',(35.2490119207975,-22.548695660891,15.));
#20264=CARTESIAN_POINT('Ctrl Pts',(35.1963130003352,-22.4626392230023,15.));
#20265=CARTESIAN_POINT('Ctrl Pts',(35.1432094422642,-22.3769908340843,15.));
#20266=CARTESIAN_POINT('Ctrl Pts',(35.0896991159359,-22.2917560356803,15.));
#20267=CARTESIAN_POINT('Ctrl Pts',(35.0357795922459,-22.2069408519233,15.));
#20268=CARTESIAN_POINT('Ctrl Pts',(34.9814483545602,-22.1225514798584,15.));
#20269=CARTESIAN_POINT('Ctrl Pts',(34.9267029879922,-22.0385940162683,15.));
#20270=CARTESIAN_POINT('Ctrl Pts',(34.8715413418101,-21.9550742217675,15.));
#20271=CARTESIAN_POINT('Ctrl Pts',(34.8159618014436,-21.8719971302818,15.));
#20272=CARTESIAN_POINT('Ctrl Pts',(34.7599631530844,-21.7893672401137,15.));
#20273=CARTESIAN_POINT('Ctrl Pts',(34.7035440429025,-21.7071892844497,15.));
#20274=CARTESIAN_POINT('Ctrl Pts',(34.6467025072367,-21.6254689009796,15.));
#20275=CARTESIAN_POINT('Ctrl Pts',(34.5894355639082,-21.5442132160757,15.));
#20276=CARTESIAN_POINT('Ctrl Pts',(34.5317385658329,-21.4634317666005,15.));
#20277=CARTESIAN_POINT('Ctrl Pts',(34.4736054662052,-21.3831361300104,15.));
#20278=CARTESIAN_POINT('Ctrl Pts',(34.4150300340623,-21.3033382073239,15.));
#20279=CARTESIAN_POINT('Ctrl Pts',(34.3560069185815,-21.2240487218079,15.));
#20280=CARTESIAN_POINT('Ctrl Pts',(34.2965325673384,-21.14527592444,15.));
#20281=CARTESIAN_POINT('Ctrl Pts',(34.2366067284279,-21.0670234747355,15.));
#20282=CARTESIAN_POINT('Ctrl Pts',(34.176231731809,-20.9892914622612,15.));
#20283=CARTESIAN_POINT('Ctrl Pts',(34.1154095510973,-20.9120805673809,15.));
#20284=CARTESIAN_POINT('Ctrl Pts',(34.0541392299678,-20.8353957068415,15.));
#20285=CARTESIAN_POINT('Ctrl Pts',(33.9924146647395,-20.7592491770603,15.));
#20286=CARTESIAN_POINT('Ctrl Pts',(33.9302209962425,-20.683665762903,15.));
#20287=CARTESIAN_POINT('Ctrl Pts',(33.8675365150454,-20.6086800574386,15.));
#20288=CARTESIAN_POINT('Ctrl Pts',(33.8043393734971,-20.5343269914034,15.));
#20289=CARTESIAN_POINT('Ctrl Pts',(33.7406135254082,-20.4606334536183,15.));
#20290=CARTESIAN_POINT('Ctrl Pts',(33.6763537716992,-20.3876111773341,15.));
#20291=CARTESIAN_POINT('Ctrl Pts',(33.6115742164079,-20.3152448035298,15.));
#20292=CARTESIAN_POINT('Ctrl Pts',(33.5463023319603,-20.243500298383,15.));
#20293=CARTESIAN_POINT('Ctrl Pts',(33.480563024813,-20.1723475154533,15.));
#20294=CARTESIAN_POINT('Ctrl Pts',(33.4143643679979,-20.1017803986381,15.));
#20295=CARTESIAN_POINT('Ctrl Pts',(33.3476854048385,-20.0318342617213,15.));
#20296=CARTESIAN_POINT('Ctrl Pts',(33.2804560993213,-19.9626141625206,15.));
#20297=CARTESIAN_POINT('Ctrl Pts',(33.2125746879471,-19.8942704458546,15.));
#20298=CARTESIAN_POINT('Ctrl Pts',(33.1439436707661,-19.8269479776239,15.));
#20299=CARTESIAN_POINT('Ctrl Pts',(33.0745026283418,-19.7607398248651,15.));
#20300=CARTESIAN_POINT('Ctrl Pts',(33.004256563411,-19.6956473461873,15.));
#20301=CARTESIAN_POINT('Ctrl Pts',(32.9333211533788,-19.6315161742485,15.));
#20302=CARTESIAN_POINT('Ctrl Pts',(32.8618672807884,-19.5681157030437,15.));
#20303=CARTESIAN_POINT('Ctrl Pts',(32.7900335943248,-19.5052640847974,15.));
#20304=CARTESIAN_POINT('Ctrl Pts',(32.7178463324062,-19.4429429601189,15.));
#20305=CARTESIAN_POINT('Ctrl Pts',(32.6451434870609,-19.381405831319,15.));
#20306=CARTESIAN_POINT('Ctrl Pts',(32.5714771007861,-19.3213180490743,15.));
#20307=CARTESIAN_POINT('Ctrl Pts',(32.4962340238036,-19.2635813403783,15.));
#20308=CARTESIAN_POINT('Ctrl Pts',(32.4342791270009,-19.2200039764927,15.));
#20309=CARTESIAN_POINT('Ctrl Pts',(32.3866012518553,-19.1891139208368,15.));
#20310=CARTESIAN_POINT('Ctrl Pts',(32.3542491343753,-19.1693587749508,15.));
#20311=CARTESIAN_POINT('Ctrl Pts',(32.3379313568208,-19.1596907609891,15.));
#20312=CARTESIAN_POINT('',(36.3957374383337,-24.7254989094229,0.));
#20313=CARTESIAN_POINT('Origin',(9.16871631793044E-12,-6.66146233219319E-12,
0.));
#20314=CARTESIAN_POINT('',(34.762248247709,-26.9738038986838,0.));
#20315=CARTESIAN_POINT('Origin',(9.16871631793044E-12,-6.66146233219319E-12,
0.));
#20316=CARTESIAN_POINT('',(34.762248247709,-26.9738038986838,15.));
#20317=CARTESIAN_POINT('Origin',(9.16871631793044E-12,-6.66146233219319E-12,
15.));
#20318=CARTESIAN_POINT('',(34.762248247709,-26.9738038986838,0.));
#20319=CARTESIAN_POINT('Ctrl Pts',(28.2149191006268,-24.8345302882955,0.));
#20320=CARTESIAN_POINT('Ctrl Pts',(28.2149191006268,-24.8345302882955,18.));
#20321=CARTESIAN_POINT('Ctrl Pts',(28.2291563988795,-24.8470618363541,0.));
#20322=CARTESIAN_POINT('Ctrl Pts',(28.2291563988795,-24.8470618363541,18.));
#20323=CARTESIAN_POINT('Ctrl Pts',(28.2579420132101,-24.8717258526943,0.));
#20324=CARTESIAN_POINT('Ctrl Pts',(28.2579420132101,-24.8717258526943,18.));
#20325=CARTESIAN_POINT('Ctrl Pts',(28.3020534756061,-24.9075246543798,0.));
#20326=CARTESIAN_POINT('Ctrl Pts',(28.3020534756061,-24.9075246543798,18.));
#20327=CARTESIAN_POINT('Ctrl Pts',(28.3626431274892,-24.9529811166897,0.));
#20328=CARTESIAN_POINT('Ctrl Pts',(28.3626431274892,-24.9529811166897,18.));
#20329=CARTESIAN_POINT('Ctrl Pts',(28.4408053900206,-25.0066999111736,0.));
#20330=CARTESIAN_POINT('Ctrl Pts',(28.4408053900206,-25.0066999111736,18.));
#20331=CARTESIAN_POINT('Ctrl Pts',(28.5207164321473,-25.0581926620043,0.));
#20332=CARTESIAN_POINT('Ctrl Pts',(28.5207164321473,-25.0581926620043,18.));
#20333=CARTESIAN_POINT('Ctrl Pts',(28.6017081342376,-25.108321158239,0.));
#20334=CARTESIAN_POINT('Ctrl Pts',(28.6017081342376,-25.108321158239,18.));
#20335=CARTESIAN_POINT('Ctrl Pts',(28.6832861366762,-25.1577170374459,0.));
#20336=CARTESIAN_POINT('Ctrl Pts',(28.6832861366762,-25.1577170374459,18.));
#20337=CARTESIAN_POINT('Ctrl Pts',(28.7652594076549,-25.2066127148845,0.));
#20338=CARTESIAN_POINT('Ctrl Pts',(28.7652594076549,-25.2066127148845,18.));
#20339=CARTESIAN_POINT('Ctrl Pts',(28.8476372998748,-25.2549775629725,0.));
#20340=CARTESIAN_POINT('Ctrl Pts',(28.8476372998748,-25.2549775629725,18.));
#20341=CARTESIAN_POINT('Ctrl Pts',(28.9305499160476,-25.3026235249214,0.));
#20342=CARTESIAN_POINT('Ctrl Pts',(28.9305499160476,-25.3026235249214,18.));
#20343=CARTESIAN_POINT('Ctrl Pts',(29.0141637699076,-25.3493168206005,0.));
#20344=CARTESIAN_POINT('Ctrl Pts',(29.0141637699076,-25.3493168206005,18.));
#20345=CARTESIAN_POINT('Ctrl Pts',(29.098589927237,-25.3948997321279,0.));
#20346=CARTESIAN_POINT('Ctrl Pts',(29.098589927237,-25.3948997321279,18.));
#20347=CARTESIAN_POINT('Ctrl Pts',(29.183825549991,-25.4393679214513,0.));
#20348=CARTESIAN_POINT('Ctrl Pts',(29.183825549991,-25.4393679214513,18.));
#20349=CARTESIAN_POINT('Ctrl Pts',(29.2698007967907,-25.4828076101654,0.));
#20350=CARTESIAN_POINT('Ctrl Pts',(29.2698007967907,-25.4828076101654,18.));
#20351=CARTESIAN_POINT('Ctrl Pts',(29.356408021119,-25.5253562922582,0.));
#20352=CARTESIAN_POINT('Ctrl Pts',(29.356408021119,-25.5253562922582,18.));
#20353=CARTESIAN_POINT('Ctrl Pts',(29.443535683207,-25.5671572096726,0.));
#20354=CARTESIAN_POINT('Ctrl Pts',(29.443535683207,-25.5671572096726,18.));
#20355=CARTESIAN_POINT('Ctrl Pts',(29.5311055094509,-25.6083094352667,0.));
#20356=CARTESIAN_POINT('Ctrl Pts',(29.5311055094509,-25.6083094352667,18.));
#20357=CARTESIAN_POINT('Ctrl Pts',(29.6190903904157,-25.6488438125835,0.));
#20358=CARTESIAN_POINT('Ctrl Pts',(29.6190903904157,-25.6488438125835,18.));
#20359=CARTESIAN_POINT('Ctrl Pts',(29.7074935910931,-25.6887507922749,0.));
#20360=CARTESIAN_POINT('Ctrl Pts',(29.7074935910931,-25.6887507922749,18.));
#20361=CARTESIAN_POINT('Ctrl Pts',(29.7963360859334,-25.7279973711305,0.));
#20362=CARTESIAN_POINT('Ctrl Pts',(29.7963360859334,-25.7279973711305,18.));
#20363=CARTESIAN_POINT('Ctrl Pts',(29.8856417535786,-25.7665469042913,0.));
#20364=CARTESIAN_POINT('Ctrl Pts',(29.8856417535786,-25.7665469042913,18.));
#20365=CARTESIAN_POINT('Ctrl Pts',(29.9754208429384,-25.8043812318215,0.));
#20366=CARTESIAN_POINT('Ctrl Pts',(29.9754208429384,-25.8043812318215,18.));
#20367=CARTESIAN_POINT('Ctrl Pts',(30.0656638016321,-25.8415089241134,0.));
#20368=CARTESIAN_POINT('Ctrl Pts',(30.0656638016321,-25.8415089241134,18.));
#20369=CARTESIAN_POINT('Ctrl Pts',(30.1563500154165,-25.8779535511028,0.));
#20370=CARTESIAN_POINT('Ctrl Pts',(30.1563500154165,-25.8779535511028,18.));
#20371=CARTESIAN_POINT('Ctrl Pts',(30.2474530144827,-25.9137466853317,0.));
#20372=CARTESIAN_POINT('Ctrl Pts',(30.2474530144827,-25.9137466853317,18.));
#20373=CARTESIAN_POINT('Ctrl Pts',(30.3389466074503,-25.9489196635424,0.));
#20374=CARTESIAN_POINT('Ctrl Pts',(30.3389466074503,-25.9489196635424,18.));
#20375=CARTESIAN_POINT('Ctrl Pts',(30.4308118142473,-25.9834942765902,0.));
#20376=CARTESIAN_POINT('Ctrl Pts',(30.4308118142473,-25.9834942765902,18.));
#20377=CARTESIAN_POINT('Ctrl Pts',(30.5230388264271,-26.0174801292225,0.));
#20378=CARTESIAN_POINT('Ctrl Pts',(30.5230388264271,-26.0174801292225,18.));
#20379=CARTESIAN_POINT('Ctrl Pts',(30.6156232634061,-26.0508796503166,0.));
#20380=CARTESIAN_POINT('Ctrl Pts',(30.6156232634061,-26.0508796503166,18.));
#20381=CARTESIAN_POINT('Ctrl Pts',(30.7085638682391,-26.0836911730968,0.));
#20382=CARTESIAN_POINT('Ctrl Pts',(30.7085638682391,-26.0836911730968,18.));
#20383=CARTESIAN_POINT('Ctrl Pts',(30.8018598357461,-26.1159125093178,0.));
#20384=CARTESIAN_POINT('Ctrl Pts',(30.8018598357461,-26.1159125093178,18.));
#20385=CARTESIAN_POINT('Ctrl Pts',(30.8955077633644,-26.1475450294082,0.));
#20386=CARTESIAN_POINT('Ctrl Pts',(30.8955077633644,-26.1475450294082,18.));
#20387=CARTESIAN_POINT('Ctrl Pts',(30.9895009017072,-26.1785946616165,0.));
#20388=CARTESIAN_POINT('Ctrl Pts',(30.9895009017072,-26.1785946616165,18.));
#20389=CARTESIAN_POINT('Ctrl Pts',(31.0838307058369,-26.2090698085494,0.));
#20390=CARTESIAN_POINT('Ctrl Pts',(31.0838307058369,-26.2090698085494,18.));
#20391=CARTESIAN_POINT('Ctrl Pts',(31.1784877826858,-26.2389800738215,0.));
#20392=CARTESIAN_POINT('Ctrl Pts',(31.1784877826858,-26.2389800738215,18.));
#20393=CARTESIAN_POINT('Ctrl Pts',(31.2734629900041,-26.2683347859175,0.));
#20394=CARTESIAN_POINT('Ctrl Pts',(31.2734629900041,-26.2683347859175,18.));
#20395=CARTESIAN_POINT('Ctrl Pts',(31.3687486937246,-26.2971413115295,0.));
#20396=CARTESIAN_POINT('Ctrl Pts',(31.3687486937246,-26.2971413115295,18.));
#20397=CARTESIAN_POINT('Ctrl Pts',(31.4643390378083,-26.3254046890485,0.));
#20398=CARTESIAN_POINT('Ctrl Pts',(31.4643390378083,-26.3254046890485,18.));
#20399=CARTESIAN_POINT('Ctrl Pts',(31.5602292672984,-26.353128528169,0.));
#20400=CARTESIAN_POINT('Ctrl Pts',(31.5602292672984,-26.353128528169,18.));
#20401=CARTESIAN_POINT('Ctrl Pts',(31.6564152990236,-26.3803155790949,0.));
#20402=CARTESIAN_POINT('Ctrl Pts',(31.6564152990236,-26.3803155790949,18.));
#20403=CARTESIAN_POINT('Ctrl Pts',(31.7528932299312,-26.4069683862785,0.));
#20404=CARTESIAN_POINT('Ctrl Pts',(31.7528932299312,-26.4069683862785,18.));
#20405=CARTESIAN_POINT('Ctrl Pts',(31.849658771403,-26.433090040836,0.));
#20406=CARTESIAN_POINT('Ctrl Pts',(31.849658771403,-26.433090040836,18.));
#20407=CARTESIAN_POINT('Ctrl Pts',(31.9467071093816,-26.4586843683627,0.));
#20408=CARTESIAN_POINT('Ctrl Pts',(31.9467071093816,-26.4586843683627,18.));
#20409=CARTESIAN_POINT('Ctrl Pts',(32.0440331917233,-26.4837555495616,0.));
#20410=CARTESIAN_POINT('Ctrl Pts',(32.0440331917233,-26.4837555495616,18.));
#20411=CARTESIAN_POINT('Ctrl Pts',(32.1416319023705,-26.5083078928862,0.));
#20412=CARTESIAN_POINT('Ctrl Pts',(32.1416319023705,-26.5083078928862,18.));
#20413=CARTESIAN_POINT('Ctrl Pts',(32.2394982626669,-26.5323455701117,0.));
#20414=CARTESIAN_POINT('Ctrl Pts',(32.2394982626669,-26.5323455701117,18.));
#20415=CARTESIAN_POINT('Ctrl Pts',(32.3376276606981,-26.5558723200361,0.));
#20416=CARTESIAN_POINT('Ctrl Pts',(32.3376276606981,-26.5558723200361,18.));
#20417=CARTESIAN_POINT('Ctrl Pts',(32.4360159072985,-26.5788913672813,0.));
#20418=CARTESIAN_POINT('Ctrl Pts',(32.4360159072985,-26.5788913672813,18.));
#20419=CARTESIAN_POINT('Ctrl Pts',(32.5346590925498,-26.6014055904817,0.));
#20420=CARTESIAN_POINT('Ctrl Pts',(32.5346590925498,-26.6014055904817,18.));
#20421=CARTESIAN_POINT('Ctrl Pts',(32.6335534898935,-26.6234176311245,0.));
#20422=CARTESIAN_POINT('Ctrl Pts',(32.6335534898935,-26.6234176311245,18.));
#20423=CARTESIAN_POINT('Ctrl Pts',(32.7326954489334,-26.6449300199764,0.));
#20424=CARTESIAN_POINT('Ctrl Pts',(32.7326954489334,-26.6449300199764,18.));
#20425=CARTESIAN_POINT('Ctrl Pts',(32.8320812678271,-26.6659453236976,0.));
#20426=CARTESIAN_POINT('Ctrl Pts',(32.8320812678271,-26.6659453236976,18.));
#20427=CARTESIAN_POINT('Ctrl Pts',(32.9317071576181,-26.6864661988935,0.));
#20428=CARTESIAN_POINT('Ctrl Pts',(32.9317071576181,-26.6864661988935,18.));
#20429=CARTESIAN_POINT('Ctrl Pts',(33.03156933761,-26.7064953106254,0.));
#20430=CARTESIAN_POINT('Ctrl Pts',(33.03156933761,-26.7064953106254,18.));
#20431=CARTESIAN_POINT('Ctrl Pts',(33.131664100194,-26.7260352861619,0.));
#20432=CARTESIAN_POINT('Ctrl Pts',(33.131664100194,-26.7260352861619,18.));
#20433=CARTESIAN_POINT('Ctrl Pts',(33.2319878786519,-26.7450886617884,0.));
#20434=CARTESIAN_POINT('Ctrl Pts',(33.2319878786519,-26.7450886617884,18.));
#20435=CARTESIAN_POINT('Ctrl Pts',(33.3325373307046,-26.7636578270526,0.));
#20436=CARTESIAN_POINT('Ctrl Pts',(33.3325373307046,-26.7636578270526,18.));
#20437=CARTESIAN_POINT('Ctrl Pts',(33.4333093513694,-26.7817450041181,0.));
#20438=CARTESIAN_POINT('Ctrl Pts',(33.4333093513694,-26.7817450041181,18.));
#20439=CARTESIAN_POINT('Ctrl Pts',(33.5343009499673,-26.7993522966985,0.));
#20440=CARTESIAN_POINT('Ctrl Pts',(33.5343009499673,-26.7993522966985,18.));
#20441=CARTESIAN_POINT('Ctrl Pts',(33.6355091508895,-26.8164817280846,0.));
#20442=CARTESIAN_POINT('Ctrl Pts',(33.6355091508895,-26.8164817280846,18.));
#20443=CARTESIAN_POINT('Ctrl Pts',(33.7369308933173,-26.8331352836667,0.));
#20444=CARTESIAN_POINT('Ctrl Pts',(33.7369308933173,-26.8331352836667,18.));
#20445=CARTESIAN_POINT('Ctrl Pts',(33.838562905895,-26.8493149627661,0.));
#20446=CARTESIAN_POINT('Ctrl Pts',(33.838562905895,-26.8493149627661,18.));
#20447=CARTESIAN_POINT('Ctrl Pts',(33.9404016650487,-26.8650228056313,0.));
#20448=CARTESIAN_POINT('Ctrl Pts',(33.9404016650487,-26.8650228056313,18.));
#20449=CARTESIAN_POINT('Ctrl Pts',(34.0424436187397,-26.880260834701,0.));
#20450=CARTESIAN_POINT('Ctrl Pts',(34.0424436187397,-26.880260834701,18.));
#20451=CARTESIAN_POINT('Ctrl Pts',(34.1446853651051,-26.895031013894,0.));
#20452=CARTESIAN_POINT('Ctrl Pts',(34.1446853651051,-26.895031013894,18.));
#20453=CARTESIAN_POINT('Ctrl Pts',(34.2471238425419,-26.9093352037262,0.));
#20454=CARTESIAN_POINT('Ctrl Pts',(34.2471238425419,-26.9093352037262,18.));
#20455=CARTESIAN_POINT('Ctrl Pts',(34.3497565255724,-26.9231751225177,0.));
#20456=CARTESIAN_POINT('Ctrl Pts',(34.3497565255724,-26.9231751225177,18.));
#20457=CARTESIAN_POINT('Ctrl Pts',(34.4525815829097,-26.9365523054581,0.));
#20458=CARTESIAN_POINT('Ctrl Pts',(34.4525815829097,-26.9365523054581,18.));
#20459=CARTESIAN_POINT('Ctrl Pts',(34.5555977590573,-26.9494680440307,0.));
#20460=CARTESIAN_POINT('Ctrl Pts',(34.5555977590573,-26.9494680440307,18.));
#20461=CARTESIAN_POINT('Ctrl Pts',(34.6381629799782,-26.9594322726214,0.));
#20462=CARTESIAN_POINT('Ctrl Pts',(34.6381629799782,-26.9594322726214,18.));
#20463=CARTESIAN_POINT('Ctrl Pts',(34.700172380686,-26.9666985267609,0.));
#20464=CARTESIAN_POINT('Ctrl Pts',(34.700172380686,-26.9666985267609,18.));
#20465=CARTESIAN_POINT('Ctrl Pts',(34.7415499619104,-26.9714507634923,0.));
#20466=CARTESIAN_POINT('Ctrl Pts',(34.7415499619104,-26.9714507634923,18.));
#20467=CARTESIAN_POINT('Ctrl Pts',(34.7622482477091,-26.9738038986838,0.));
#20468=CARTESIAN_POINT('Ctrl Pts',(34.7622482477091,-26.9738038986838,18.));
#20469=CARTESIAN_POINT('Ctrl Pts',(28.2149191006268,-24.8345302882955,0.));
#20470=CARTESIAN_POINT('Ctrl Pts',(28.2291563988795,-24.8470618363541,0.));
#20471=CARTESIAN_POINT('Ctrl Pts',(28.2579420132101,-24.8717258526943,0.));
#20472=CARTESIAN_POINT('Ctrl Pts',(28.3020534756061,-24.9075246543798,0.));
#20473=CARTESIAN_POINT('Ctrl Pts',(28.3626431274892,-24.9529811166897,0.));
#20474=CARTESIAN_POINT('Ctrl Pts',(28.4408053900206,-25.0066999111736,0.));
#20475=CARTESIAN_POINT('Ctrl Pts',(28.5207164321473,-25.0581926620043,0.));
#20476=CARTESIAN_POINT('Ctrl Pts',(28.6017081342376,-25.108321158239,0.));
#20477=CARTESIAN_POINT('Ctrl Pts',(28.6832861366762,-25.1577170374459,0.));
#20478=CARTESIAN_POINT('Ctrl Pts',(28.7652594076549,-25.2066127148845,0.));
#20479=CARTESIAN_POINT('Ctrl Pts',(28.8476372998748,-25.2549775629725,0.));
#20480=CARTESIAN_POINT('Ctrl Pts',(28.9305499160476,-25.3026235249214,0.));
#20481=CARTESIAN_POINT('Ctrl Pts',(29.0141637699076,-25.3493168206005,0.));
#20482=CARTESIAN_POINT('Ctrl Pts',(29.098589927237,-25.3948997321279,0.));
#20483=CARTESIAN_POINT('Ctrl Pts',(29.183825549991,-25.4393679214513,0.));
#20484=CARTESIAN_POINT('Ctrl Pts',(29.2698007967907,-25.4828076101654,0.));
#20485=CARTESIAN_POINT('Ctrl Pts',(29.356408021119,-25.5253562922582,0.));
#20486=CARTESIAN_POINT('Ctrl Pts',(29.443535683207,-25.5671572096726,0.));
#20487=CARTESIAN_POINT('Ctrl Pts',(29.5311055094509,-25.6083094352667,0.));
#20488=CARTESIAN_POINT('Ctrl Pts',(29.6190903904157,-25.6488438125835,0.));
#20489=CARTESIAN_POINT('Ctrl Pts',(29.7074935910931,-25.6887507922749,0.));
#20490=CARTESIAN_POINT('Ctrl Pts',(29.7963360859334,-25.7279973711305,0.));
#20491=CARTESIAN_POINT('Ctrl Pts',(29.8856417535786,-25.7665469042913,0.));
#20492=CARTESIAN_POINT('Ctrl Pts',(29.9754208429384,-25.8043812318215,0.));
#20493=CARTESIAN_POINT('Ctrl Pts',(30.0656638016321,-25.8415089241134,0.));
#20494=CARTESIAN_POINT('Ctrl Pts',(30.1563500154165,-25.8779535511028,0.));
#20495=CARTESIAN_POINT('Ctrl Pts',(30.2474530144827,-25.9137466853317,0.));
#20496=CARTESIAN_POINT('Ctrl Pts',(30.3389466074503,-25.9489196635424,0.));
#20497=CARTESIAN_POINT('Ctrl Pts',(30.4308118142473,-25.9834942765902,0.));
#20498=CARTESIAN_POINT('Ctrl Pts',(30.5230388264271,-26.0174801292225,0.));
#20499=CARTESIAN_POINT('Ctrl Pts',(30.6156232634061,-26.0508796503166,0.));
#20500=CARTESIAN_POINT('Ctrl Pts',(30.7085638682391,-26.0836911730968,0.));
#20501=CARTESIAN_POINT('Ctrl Pts',(30.8018598357461,-26.1159125093178,0.));
#20502=CARTESIAN_POINT('Ctrl Pts',(30.8955077633644,-26.1475450294082,0.));
#20503=CARTESIAN_POINT('Ctrl Pts',(30.9895009017072,-26.1785946616165,0.));
#20504=CARTESIAN_POINT('Ctrl Pts',(31.0838307058369,-26.2090698085494,0.));
#20505=CARTESIAN_POINT('Ctrl Pts',(31.1784877826858,-26.2389800738215,0.));
#20506=CARTESIAN_POINT('Ctrl Pts',(31.2734629900041,-26.2683347859175,0.));
#20507=CARTESIAN_POINT('Ctrl Pts',(31.3687486937246,-26.2971413115295,0.));
#20508=CARTESIAN_POINT('Ctrl Pts',(31.4643390378083,-26.3254046890485,0.));
#20509=CARTESIAN_POINT('Ctrl Pts',(31.5602292672984,-26.353128528169,0.));
#20510=CARTESIAN_POINT('Ctrl Pts',(31.6564152990236,-26.3803155790949,0.));
#20511=CARTESIAN_POINT('Ctrl Pts',(31.7528932299312,-26.4069683862785,0.));
#20512=CARTESIAN_POINT('Ctrl Pts',(31.849658771403,-26.433090040836,0.));
#20513=CARTESIAN_POINT('Ctrl Pts',(31.9467071093816,-26.4586843683627,0.));
#20514=CARTESIAN_POINT('Ctrl Pts',(32.0440331917233,-26.4837555495616,0.));
#20515=CARTESIAN_POINT('Ctrl Pts',(32.1416319023705,-26.5083078928862,0.));
#20516=CARTESIAN_POINT('Ctrl Pts',(32.2394982626669,-26.5323455701117,0.));
#20517=CARTESIAN_POINT('Ctrl Pts',(32.3376276606981,-26.5558723200361,0.));
#20518=CARTESIAN_POINT('Ctrl Pts',(32.4360159072985,-26.5788913672813,0.));
#20519=CARTESIAN_POINT('Ctrl Pts',(32.5346590925498,-26.6014055904817,0.));
#20520=CARTESIAN_POINT('Ctrl Pts',(32.6335534898935,-26.6234176311245,0.));
#20521=CARTESIAN_POINT('Ctrl Pts',(32.7326954489334,-26.6449300199764,0.));
#20522=CARTESIAN_POINT('Ctrl Pts',(32.8320812678271,-26.6659453236976,0.));
#20523=CARTESIAN_POINT('Ctrl Pts',(32.9317071576181,-26.6864661988935,0.));
#20524=CARTESIAN_POINT('Ctrl Pts',(33.03156933761,-26.7064953106254,0.));
#20525=CARTESIAN_POINT('Ctrl Pts',(33.131664100194,-26.7260352861619,0.));
#20526=CARTESIAN_POINT('Ctrl Pts',(33.2319878786519,-26.7450886617884,0.));
#20527=CARTESIAN_POINT('Ctrl Pts',(33.3325373307046,-26.7636578270526,0.));
#20528=CARTESIAN_POINT('Ctrl Pts',(33.4333093513694,-26.7817450041181,0.));
#20529=CARTESIAN_POINT('Ctrl Pts',(33.5343009499673,-26.7993522966985,0.));
#20530=CARTESIAN_POINT('Ctrl Pts',(33.6355091508895,-26.8164817280846,0.));
#20531=CARTESIAN_POINT('Ctrl Pts',(33.7369308933173,-26.8331352836667,0.));
#20532=CARTESIAN_POINT('Ctrl Pts',(33.838562905895,-26.8493149627661,0.));
#20533=CARTESIAN_POINT('Ctrl Pts',(33.9404016650487,-26.8650228056313,0.));
#20534=CARTESIAN_POINT('Ctrl Pts',(34.0424436187397,-26.880260834701,0.));
#20535=CARTESIAN_POINT('Ctrl Pts',(34.1446853651051,-26.895031013894,0.));
#20536=CARTESIAN_POINT('Ctrl Pts',(34.2471238425419,-26.9093352037262,0.));
#20537=CARTESIAN_POINT('Ctrl Pts',(34.3497565255724,-26.9231751225177,0.));
#20538=CARTESIAN_POINT('Ctrl Pts',(34.4731465943772,-26.9392277420462,0.));
#20539=CARTESIAN_POINT('Ctrl Pts',(34.5762105502273,-26.9520281195268,0.));
#20540=CARTESIAN_POINT('Ctrl Pts',(34.6588137898952,-26.9619003236529,0.));
#20541=CARTESIAN_POINT('Ctrl Pts',(34.7208516760814,-26.9690976283149,0.));
#20542=CARTESIAN_POINT('Ctrl Pts',(34.7622482477091,-26.9738038986838,0.));
#20543=CARTESIAN_POINT('Ctrl Pts',(28.2149191006268,-24.8345302882955,15.));
#20544=CARTESIAN_POINT('Ctrl Pts',(28.2291563988795,-24.8470618363541,15.));
#20545=CARTESIAN_POINT('Ctrl Pts',(28.2579420132101,-24.8717258526943,15.));
#20546=CARTESIAN_POINT('Ctrl Pts',(28.3020534756061,-24.9075246543798,15.));
#20547=CARTESIAN_POINT('Ctrl Pts',(28.3626431274892,-24.9529811166897,15.));
#20548=CARTESIAN_POINT('Ctrl Pts',(28.4408053900206,-25.0066999111736,15.));
#20549=CARTESIAN_POINT('Ctrl Pts',(28.5207164321473,-25.0581926620043,15.));
#20550=CARTESIAN_POINT('Ctrl Pts',(28.6017081342376,-25.108321158239,15.));
#20551=CARTESIAN_POINT('Ctrl Pts',(28.6832861366762,-25.1577170374459,15.));
#20552=CARTESIAN_POINT('Ctrl Pts',(28.7652594076549,-25.2066127148845,15.));
#20553=CARTESIAN_POINT('Ctrl Pts',(28.8476372998748,-25.2549775629725,15.));
#20554=CARTESIAN_POINT('Ctrl Pts',(28.9305499160476,-25.3026235249214,15.));
#20555=CARTESIAN_POINT('Ctrl Pts',(29.0141637699076,-25.3493168206005,15.));
#20556=CARTESIAN_POINT('Ctrl Pts',(29.098589927237,-25.3948997321279,15.));
#20557=CARTESIAN_POINT('Ctrl Pts',(29.183825549991,-25.4393679214513,15.));
#20558=CARTESIAN_POINT('Ctrl Pts',(29.2698007967907,-25.4828076101654,15.));
#20559=CARTESIAN_POINT('Ctrl Pts',(29.356408021119,-25.5253562922582,15.));
#20560=CARTESIAN_POINT('Ctrl Pts',(29.443535683207,-25.5671572096726,15.));
#20561=CARTESIAN_POINT('Ctrl Pts',(29.5311055094509,-25.6083094352667,15.));
#20562=CARTESIAN_POINT('Ctrl Pts',(29.6190903904157,-25.6488438125835,15.));
#20563=CARTESIAN_POINT('Ctrl Pts',(29.7074935910931,-25.6887507922749,15.));
#20564=CARTESIAN_POINT('Ctrl Pts',(29.7963360859334,-25.7279973711305,15.));
#20565=CARTESIAN_POINT('Ctrl Pts',(29.8856417535786,-25.7665469042913,15.));
#20566=CARTESIAN_POINT('Ctrl Pts',(29.9754208429384,-25.8043812318215,15.));
#20567=CARTESIAN_POINT('Ctrl Pts',(30.0656638016321,-25.8415089241134,15.));
#20568=CARTESIAN_POINT('Ctrl Pts',(30.1563500154165,-25.8779535511028,15.));
#20569=CARTESIAN_POINT('Ctrl Pts',(30.2474530144827,-25.9137466853317,15.));
#20570=CARTESIAN_POINT('Ctrl Pts',(30.3389466074503,-25.9489196635424,15.));
#20571=CARTESIAN_POINT('Ctrl Pts',(30.4308118142473,-25.9834942765902,15.));
#20572=CARTESIAN_POINT('Ctrl Pts',(30.5230388264271,-26.0174801292225,15.));
#20573=CARTESIAN_POINT('Ctrl Pts',(30.6156232634061,-26.0508796503166,15.));
#20574=CARTESIAN_POINT('Ctrl Pts',(30.7085638682391,-26.0836911730968,15.));
#20575=CARTESIAN_POINT('Ctrl Pts',(30.8018598357461,-26.1159125093178,15.));
#20576=CARTESIAN_POINT('Ctrl Pts',(30.8955077633644,-26.1475450294082,15.));
#20577=CARTESIAN_POINT('Ctrl Pts',(30.9895009017072,-26.1785946616165,15.));
#20578=CARTESIAN_POINT('Ctrl Pts',(31.0838307058369,-26.2090698085494,15.));
#20579=CARTESIAN_POINT('Ctrl Pts',(31.1784877826858,-26.2389800738215,15.));
#20580=CARTESIAN_POINT('Ctrl Pts',(31.2734629900041,-26.2683347859175,15.));
#20581=CARTESIAN_POINT('Ctrl Pts',(31.3687486937246,-26.2971413115295,15.));
#20582=CARTESIAN_POINT('Ctrl Pts',(31.4643390378083,-26.3254046890485,15.));
#20583=CARTESIAN_POINT('Ctrl Pts',(31.5602292672984,-26.353128528169,15.));
#20584=CARTESIAN_POINT('Ctrl Pts',(31.6564152990236,-26.3803155790949,15.));
#20585=CARTESIAN_POINT('Ctrl Pts',(31.7528932299312,-26.4069683862785,15.));
#20586=CARTESIAN_POINT('Ctrl Pts',(31.849658771403,-26.433090040836,15.));
#20587=CARTESIAN_POINT('Ctrl Pts',(31.9467071093816,-26.4586843683627,15.));
#20588=CARTESIAN_POINT('Ctrl Pts',(32.0440331917233,-26.4837555495616,15.));
#20589=CARTESIAN_POINT('Ctrl Pts',(32.1416319023705,-26.5083078928862,15.));
#20590=CARTESIAN_POINT('Ctrl Pts',(32.2394982626669,-26.5323455701117,15.));
#20591=CARTESIAN_POINT('Ctrl Pts',(32.3376276606981,-26.5558723200361,15.));
#20592=CARTESIAN_POINT('Ctrl Pts',(32.4360159072985,-26.5788913672813,15.));
#20593=CARTESIAN_POINT('Ctrl Pts',(32.5346590925498,-26.6014055904817,15.));
#20594=CARTESIAN_POINT('Ctrl Pts',(32.6335534898935,-26.6234176311245,15.));
#20595=CARTESIAN_POINT('Ctrl Pts',(32.7326954489334,-26.6449300199764,15.));
#20596=CARTESIAN_POINT('Ctrl Pts',(32.8320812678271,-26.6659453236976,15.));
#20597=CARTESIAN_POINT('Ctrl Pts',(32.9317071576181,-26.6864661988935,15.));
#20598=CARTESIAN_POINT('Ctrl Pts',(33.03156933761,-26.7064953106254,15.));
#20599=CARTESIAN_POINT('Ctrl Pts',(33.131664100194,-26.7260352861619,15.));
#20600=CARTESIAN_POINT('Ctrl Pts',(33.2319878786519,-26.7450886617884,15.));
#20601=CARTESIAN_POINT('Ctrl Pts',(33.3325373307046,-26.7636578270526,15.));
#20602=CARTESIAN_POINT('Ctrl Pts',(33.4333093513694,-26.7817450041181,15.));
#20603=CARTESIAN_POINT('Ctrl Pts',(33.5343009499673,-26.7993522966985,15.));
#20604=CARTESIAN_POINT('Ctrl Pts',(33.6355091508895,-26.8164817280846,15.));
#20605=CARTESIAN_POINT('Ctrl Pts',(33.7369308933173,-26.8331352836667,15.));
#20606=CARTESIAN_POINT('Ctrl Pts',(33.838562905895,-26.8493149627661,15.));
#20607=CARTESIAN_POINT('Ctrl Pts',(33.9404016650487,-26.8650228056313,15.));
#20608=CARTESIAN_POINT('Ctrl Pts',(34.0424436187397,-26.880260834701,15.));
#20609=CARTESIAN_POINT('Ctrl Pts',(34.1446853651051,-26.895031013894,15.));
#20610=CARTESIAN_POINT('Ctrl Pts',(34.2471238425419,-26.9093352037262,15.));
#20611=CARTESIAN_POINT('Ctrl Pts',(34.3497565255724,-26.9231751225177,15.));
#20612=CARTESIAN_POINT('Ctrl Pts',(34.4731465943772,-26.9392277420462,15.));
#20613=CARTESIAN_POINT('Ctrl Pts',(34.5762105502273,-26.9520281195268,15.));
#20614=CARTESIAN_POINT('Ctrl Pts',(34.6588137898952,-26.9619003236529,15.));
#20615=CARTESIAN_POINT('Ctrl Pts',(34.7208516760814,-26.9690976283149,15.));
#20616=CARTESIAN_POINT('Ctrl Pts',(34.7622482477091,-26.9738038986838,15.));
#20617=CARTESIAN_POINT('Ctrl Pts',(26.9738038986838,-34.7622482477091,0.));
#20618=CARTESIAN_POINT('Ctrl Pts',(26.9738038986838,-34.7622482477091,18.));
#20619=CARTESIAN_POINT('Ctrl Pts',(26.9714507634922,-34.7415499619104,0.));
#20620=CARTESIAN_POINT('Ctrl Pts',(26.9714507634922,-34.7415499619104,18.));
#20621=CARTESIAN_POINT('Ctrl Pts',(26.9666985267608,-34.700172380686,0.));
#20622=CARTESIAN_POINT('Ctrl Pts',(26.9666985267608,-34.700172380686,18.));
#20623=CARTESIAN_POINT('Ctrl Pts',(26.9594322726214,-34.6381629799782,0.));
#20624=CARTESIAN_POINT('Ctrl Pts',(26.9594322726214,-34.6381629799782,18.));
#20625=CARTESIAN_POINT('Ctrl Pts',(26.9494680440307,-34.5555977590573,0.));
#20626=CARTESIAN_POINT('Ctrl Pts',(26.9494680440307,-34.5555977590573,18.));
#20627=CARTESIAN_POINT('Ctrl Pts',(26.936552305458,-34.4525815829097,0.));
#20628=CARTESIAN_POINT('Ctrl Pts',(26.936552305458,-34.4525815829097,18.));
#20629=CARTESIAN_POINT('Ctrl Pts',(26.9231751225177,-34.3497565255724,0.));
#20630=CARTESIAN_POINT('Ctrl Pts',(26.9231751225177,-34.3497565255724,18.));
#20631=CARTESIAN_POINT('Ctrl Pts',(26.9093352037262,-34.2471238425419,0.));
#20632=CARTESIAN_POINT('Ctrl Pts',(26.9093352037262,-34.2471238425419,18.));
#20633=CARTESIAN_POINT('Ctrl Pts',(26.8950310138939,-34.1446853651051,0.));
#20634=CARTESIAN_POINT('Ctrl Pts',(26.8950310138939,-34.1446853651051,18.));
#20635=CARTESIAN_POINT('Ctrl Pts',(26.880260834701,-34.0424436187397,0.));
#20636=CARTESIAN_POINT('Ctrl Pts',(26.880260834701,-34.0424436187397,18.));
#20637=CARTESIAN_POINT('Ctrl Pts',(26.8650228056313,-33.9404016650487,0.));
#20638=CARTESIAN_POINT('Ctrl Pts',(26.8650228056313,-33.9404016650487,18.));
#20639=CARTESIAN_POINT('Ctrl Pts',(26.8493149627661,-33.838562905895,0.));
#20640=CARTESIAN_POINT('Ctrl Pts',(26.8493149627661,-33.838562905895,18.));
#20641=CARTESIAN_POINT('Ctrl Pts',(26.8331352836666,-33.7369308933173,0.));
#20642=CARTESIAN_POINT('Ctrl Pts',(26.8331352836666,-33.7369308933173,18.));
#20643=CARTESIAN_POINT('Ctrl Pts',(26.8164817280846,-33.6355091508895,0.));
#20644=CARTESIAN_POINT('Ctrl Pts',(26.8164817280846,-33.6355091508895,18.));
#20645=CARTESIAN_POINT('Ctrl Pts',(26.7993522966985,-33.5343009499673,0.));
#20646=CARTESIAN_POINT('Ctrl Pts',(26.7993522966985,-33.5343009499673,18.));
#20647=CARTESIAN_POINT('Ctrl Pts',(26.7817450041181,-33.4333093513694,0.));
#20648=CARTESIAN_POINT('Ctrl Pts',(26.7817450041181,-33.4333093513694,18.));
#20649=CARTESIAN_POINT('Ctrl Pts',(26.7636578270526,-33.3325373307046,0.));
#20650=CARTESIAN_POINT('Ctrl Pts',(26.7636578270526,-33.3325373307046,18.));
#20651=CARTESIAN_POINT('Ctrl Pts',(26.7450886617884,-33.231987878652,0.));
#20652=CARTESIAN_POINT('Ctrl Pts',(26.7450886617884,-33.231987878652,18.));
#20653=CARTESIAN_POINT('Ctrl Pts',(26.7260352861618,-33.131664100194,0.));
#20654=CARTESIAN_POINT('Ctrl Pts',(26.7260352861618,-33.131664100194,18.));
#20655=CARTESIAN_POINT('Ctrl Pts',(26.7064953106254,-33.03156933761,0.));
#20656=CARTESIAN_POINT('Ctrl Pts',(26.7064953106254,-33.03156933761,18.));
#20657=CARTESIAN_POINT('Ctrl Pts',(26.6864661988934,-32.9317071576181,0.));
#20658=CARTESIAN_POINT('Ctrl Pts',(26.6864661988934,-32.9317071576181,18.));
#20659=CARTESIAN_POINT('Ctrl Pts',(26.6659453236976,-32.8320812678271,0.));
#20660=CARTESIAN_POINT('Ctrl Pts',(26.6659453236976,-32.8320812678271,18.));
#20661=CARTESIAN_POINT('Ctrl Pts',(26.6449300199763,-32.7326954489334,0.));
#20662=CARTESIAN_POINT('Ctrl Pts',(26.6449300199763,-32.7326954489334,18.));
#20663=CARTESIAN_POINT('Ctrl Pts',(26.6234176311244,-32.6335534898936,0.));
#20664=CARTESIAN_POINT('Ctrl Pts',(26.6234176311244,-32.6335534898936,18.));
#20665=CARTESIAN_POINT('Ctrl Pts',(26.6014055904817,-32.5346590925498,0.));
#20666=CARTESIAN_POINT('Ctrl Pts',(26.6014055904817,-32.5346590925498,18.));
#20667=CARTESIAN_POINT('Ctrl Pts',(26.5788913672813,-32.4360159072985,0.));
#20668=CARTESIAN_POINT('Ctrl Pts',(26.5788913672813,-32.4360159072985,18.));
#20669=CARTESIAN_POINT('Ctrl Pts',(26.555872320036,-32.3376276606981,0.));
#20670=CARTESIAN_POINT('Ctrl Pts',(26.555872320036,-32.3376276606981,18.));
#20671=CARTESIAN_POINT('Ctrl Pts',(26.5323455701117,-32.2394982626669,0.));
#20672=CARTESIAN_POINT('Ctrl Pts',(26.5323455701117,-32.2394982626669,18.));
#20673=CARTESIAN_POINT('Ctrl Pts',(26.5083078928862,-32.1416319023705,0.));
#20674=CARTESIAN_POINT('Ctrl Pts',(26.5083078928862,-32.1416319023705,18.));
#20675=CARTESIAN_POINT('Ctrl Pts',(26.4837555495616,-32.0440331917233,0.));
#20676=CARTESIAN_POINT('Ctrl Pts',(26.4837555495616,-32.0440331917233,18.));
#20677=CARTESIAN_POINT('Ctrl Pts',(26.4586843683627,-31.9467071093816,0.));
#20678=CARTESIAN_POINT('Ctrl Pts',(26.4586843683627,-31.9467071093816,18.));
#20679=CARTESIAN_POINT('Ctrl Pts',(26.433090040836,-31.849658771403,0.));
#20680=CARTESIAN_POINT('Ctrl Pts',(26.433090040836,-31.849658771403,18.));
#20681=CARTESIAN_POINT('Ctrl Pts',(26.4069683862784,-31.7528932299312,0.));
#20682=CARTESIAN_POINT('Ctrl Pts',(26.4069683862784,-31.7528932299312,18.));
#20683=CARTESIAN_POINT('Ctrl Pts',(26.3803155790949,-31.6564152990236,0.));
#20684=CARTESIAN_POINT('Ctrl Pts',(26.3803155790949,-31.6564152990236,18.));
#20685=CARTESIAN_POINT('Ctrl Pts',(26.353128528169,-31.5602292672984,0.));
#20686=CARTESIAN_POINT('Ctrl Pts',(26.353128528169,-31.5602292672984,18.));
#20687=CARTESIAN_POINT('Ctrl Pts',(26.3254046890485,-31.4643390378084,0.));
#20688=CARTESIAN_POINT('Ctrl Pts',(26.3254046890485,-31.4643390378084,18.));
#20689=CARTESIAN_POINT('Ctrl Pts',(26.2971413115295,-31.3687486937246,0.));
#20690=CARTESIAN_POINT('Ctrl Pts',(26.2971413115295,-31.3687486937246,18.));
#20691=CARTESIAN_POINT('Ctrl Pts',(26.2683347859175,-31.2734629900041,0.));
#20692=CARTESIAN_POINT('Ctrl Pts',(26.2683347859175,-31.2734629900041,18.));
#20693=CARTESIAN_POINT('Ctrl Pts',(26.2389800738214,-31.1784877826858,0.));
#20694=CARTESIAN_POINT('Ctrl Pts',(26.2389800738214,-31.1784877826858,18.));
#20695=CARTESIAN_POINT('Ctrl Pts',(26.2090698085494,-31.0838307058369,0.));
#20696=CARTESIAN_POINT('Ctrl Pts',(26.2090698085494,-31.0838307058369,18.));
#20697=CARTESIAN_POINT('Ctrl Pts',(26.1785946616165,-30.9895009017073,0.));
#20698=CARTESIAN_POINT('Ctrl Pts',(26.1785946616165,-30.9895009017073,18.));
#20699=CARTESIAN_POINT('Ctrl Pts',(26.1475450294082,-30.8955077633644,0.));
#20700=CARTESIAN_POINT('Ctrl Pts',(26.1475450294082,-30.8955077633644,18.));
#20701=CARTESIAN_POINT('Ctrl Pts',(26.1159125093178,-30.8018598357461,0.));
#20702=CARTESIAN_POINT('Ctrl Pts',(26.1159125093178,-30.8018598357461,18.));
#20703=CARTESIAN_POINT('Ctrl Pts',(26.0836911730968,-30.7085638682391,0.));
#20704=CARTESIAN_POINT('Ctrl Pts',(26.0836911730968,-30.7085638682391,18.));
#20705=CARTESIAN_POINT('Ctrl Pts',(26.0508796503166,-30.6156232634061,0.));
#20706=CARTESIAN_POINT('Ctrl Pts',(26.0508796503166,-30.6156232634061,18.));
#20707=CARTESIAN_POINT('Ctrl Pts',(26.0174801292225,-30.5230388264271,0.));
#20708=CARTESIAN_POINT('Ctrl Pts',(26.0174801292225,-30.5230388264271,18.));
#20709=CARTESIAN_POINT('Ctrl Pts',(25.9834942765902,-30.4308118142473,0.));
#20710=CARTESIAN_POINT('Ctrl Pts',(25.9834942765902,-30.4308118142473,18.));
#20711=CARTESIAN_POINT('Ctrl Pts',(25.9489196635424,-30.3389466074503,0.));
#20712=CARTESIAN_POINT('Ctrl Pts',(25.9489196635424,-30.3389466074503,18.));
#20713=CARTESIAN_POINT('Ctrl Pts',(25.9137466853317,-30.2474530144827,0.));
#20714=CARTESIAN_POINT('Ctrl Pts',(25.9137466853317,-30.2474530144827,18.));
#20715=CARTESIAN_POINT('Ctrl Pts',(25.8779535511027,-30.1563500154165,0.));
#20716=CARTESIAN_POINT('Ctrl Pts',(25.8779535511027,-30.1563500154165,18.));
#20717=CARTESIAN_POINT('Ctrl Pts',(25.8415089241134,-30.0656638016321,0.));
#20718=CARTESIAN_POINT('Ctrl Pts',(25.8415089241134,-30.0656638016321,18.));
#20719=CARTESIAN_POINT('Ctrl Pts',(25.8043812318214,-29.9754208429384,0.));
#20720=CARTESIAN_POINT('Ctrl Pts',(25.8043812318214,-29.9754208429384,18.));
#20721=CARTESIAN_POINT('Ctrl Pts',(25.7665469042913,-29.8856417535786,0.));
#20722=CARTESIAN_POINT('Ctrl Pts',(25.7665469042913,-29.8856417535786,18.));
#20723=CARTESIAN_POINT('Ctrl Pts',(25.7279973711305,-29.7963360859334,0.));
#20724=CARTESIAN_POINT('Ctrl Pts',(25.7279973711305,-29.7963360859334,18.));
#20725=CARTESIAN_POINT('Ctrl Pts',(25.6887507922748,-29.7074935910931,0.));
#20726=CARTESIAN_POINT('Ctrl Pts',(25.6887507922748,-29.7074935910931,18.));
#20727=CARTESIAN_POINT('Ctrl Pts',(25.6488438125835,-29.6190903904157,0.));
#20728=CARTESIAN_POINT('Ctrl Pts',(25.6488438125835,-29.6190903904157,18.));
#20729=CARTESIAN_POINT('Ctrl Pts',(25.6083094352667,-29.5311055094509,0.));
#20730=CARTESIAN_POINT('Ctrl Pts',(25.6083094352667,-29.5311055094509,18.));
#20731=CARTESIAN_POINT('Ctrl Pts',(25.5671572096726,-29.443535683207,0.));
#20732=CARTESIAN_POINT('Ctrl Pts',(25.5671572096726,-29.443535683207,18.));
#20733=CARTESIAN_POINT('Ctrl Pts',(25.5253562922582,-29.356408021119,0.));
#20734=CARTESIAN_POINT('Ctrl Pts',(25.5253562922582,-29.356408021119,18.));
#20735=CARTESIAN_POINT('Ctrl Pts',(25.4828076101654,-29.2698007967907,0.));
#20736=CARTESIAN_POINT('Ctrl Pts',(25.4828076101654,-29.2698007967907,18.));
#20737=CARTESIAN_POINT('Ctrl Pts',(25.4393679214513,-29.183825549991,0.));
#20738=CARTESIAN_POINT('Ctrl Pts',(25.4393679214513,-29.183825549991,18.));
#20739=CARTESIAN_POINT('Ctrl Pts',(25.3948997321278,-29.098589927237,0.));
#20740=CARTESIAN_POINT('Ctrl Pts',(25.3948997321278,-29.098589927237,18.));
#20741=CARTESIAN_POINT('Ctrl Pts',(25.3493168206005,-29.0141637699076,0.));
#20742=CARTESIAN_POINT('Ctrl Pts',(25.3493168206005,-29.0141637699076,18.));
#20743=CARTESIAN_POINT('Ctrl Pts',(25.3026235249214,-28.9305499160476,0.));
#20744=CARTESIAN_POINT('Ctrl Pts',(25.3026235249214,-28.9305499160476,18.));
#20745=CARTESIAN_POINT('Ctrl Pts',(25.2549775629725,-28.8476372998748,0.));
#20746=CARTESIAN_POINT('Ctrl Pts',(25.2549775629725,-28.8476372998748,18.));
#20747=CARTESIAN_POINT('Ctrl Pts',(25.2066127148845,-28.7652594076549,0.));
#20748=CARTESIAN_POINT('Ctrl Pts',(25.2066127148845,-28.7652594076549,18.));
#20749=CARTESIAN_POINT('Ctrl Pts',(25.1577170374459,-28.6832861366762,0.));
#20750=CARTESIAN_POINT('Ctrl Pts',(25.1577170374459,-28.6832861366762,18.));
#20751=CARTESIAN_POINT('Ctrl Pts',(25.1083211582389,-28.6017081342376,0.));
#20752=CARTESIAN_POINT('Ctrl Pts',(25.1083211582389,-28.6017081342376,18.));
#20753=CARTESIAN_POINT('Ctrl Pts',(25.0581926620043,-28.5207164321473,0.));
#20754=CARTESIAN_POINT('Ctrl Pts',(25.0581926620043,-28.5207164321473,18.));
#20755=CARTESIAN_POINT('Ctrl Pts',(25.0066999111736,-28.4408053900206,0.));
#20756=CARTESIAN_POINT('Ctrl Pts',(25.0066999111736,-28.4408053900206,18.));
#20757=CARTESIAN_POINT('Ctrl Pts',(24.9529811166897,-28.3626431274892,0.));
#20758=CARTESIAN_POINT('Ctrl Pts',(24.9529811166897,-28.3626431274892,18.));
#20759=CARTESIAN_POINT('Ctrl Pts',(24.9075246543798,-28.3020534756061,0.));
#20760=CARTESIAN_POINT('Ctrl Pts',(24.9075246543798,-28.3020534756061,18.));
#20761=CARTESIAN_POINT('Ctrl Pts',(24.8717258526943,-28.2579420132101,0.));
#20762=CARTESIAN_POINT('Ctrl Pts',(24.8717258526943,-28.2579420132101,18.));
#20763=CARTESIAN_POINT('Ctrl Pts',(24.8470618363541,-28.2291563988796,0.));
#20764=CARTESIAN_POINT('Ctrl Pts',(24.8470618363541,-28.2291563988796,18.));
#20765=CARTESIAN_POINT('Ctrl Pts',(24.8345302882955,-28.2149191006269,0.));
#20766=CARTESIAN_POINT('Ctrl Pts',(24.8345302882955,-28.2149191006269,18.));
#20767=CARTESIAN_POINT('',(26.9738038986839,-34.762248247709,0.));
#20768=CARTESIAN_POINT('Ctrl Pts',(24.8345302882955,-28.2149191006269,0.));
#20769=CARTESIAN_POINT('Ctrl Pts',(24.8470618363541,-28.2291563988796,0.));
#20770=CARTESIAN_POINT('Ctrl Pts',(24.8717258526943,-28.2579420132101,0.));
#20771=CARTESIAN_POINT('Ctrl Pts',(24.9075246543798,-28.3020534756061,0.));
#20772=CARTESIAN_POINT('Ctrl Pts',(24.9529811166897,-28.3626431274892,0.));
#20773=CARTESIAN_POINT('Ctrl Pts',(25.0066999111736,-28.4408053900206,0.));
#20774=CARTESIAN_POINT('Ctrl Pts',(25.0581926620043,-28.5207164321473,0.));
#20775=CARTESIAN_POINT('Ctrl Pts',(25.1083211582389,-28.6017081342376,0.));
#20776=CARTESIAN_POINT('Ctrl Pts',(25.1577170374459,-28.6832861366762,0.));
#20777=CARTESIAN_POINT('Ctrl Pts',(25.2066127148845,-28.7652594076549,0.));
#20778=CARTESIAN_POINT('Ctrl Pts',(25.2549775629725,-28.8476372998748,0.));
#20779=CARTESIAN_POINT('Ctrl Pts',(25.3026235249214,-28.9305499160476,0.));
#20780=CARTESIAN_POINT('Ctrl Pts',(25.3493168206005,-29.0141637699076,0.));
#20781=CARTESIAN_POINT('Ctrl Pts',(25.3948997321278,-29.098589927237,0.));
#20782=CARTESIAN_POINT('Ctrl Pts',(25.4393679214513,-29.183825549991,0.));
#20783=CARTESIAN_POINT('Ctrl Pts',(25.4828076101654,-29.2698007967907,0.));
#20784=CARTESIAN_POINT('Ctrl Pts',(25.5253562922582,-29.356408021119,0.));
#20785=CARTESIAN_POINT('Ctrl Pts',(25.5671572096726,-29.443535683207,0.));
#20786=CARTESIAN_POINT('Ctrl Pts',(25.6083094352667,-29.5311055094509,0.));
#20787=CARTESIAN_POINT('Ctrl Pts',(25.6488438125835,-29.6190903904157,0.));
#20788=CARTESIAN_POINT('Ctrl Pts',(25.6887507922748,-29.7074935910931,0.));
#20789=CARTESIAN_POINT('Ctrl Pts',(25.7279973711305,-29.7963360859334,0.));
#20790=CARTESIAN_POINT('Ctrl Pts',(25.7665469042913,-29.8856417535786,0.));
#20791=CARTESIAN_POINT('Ctrl Pts',(25.8043812318214,-29.9754208429384,0.));
#20792=CARTESIAN_POINT('Ctrl Pts',(25.8415089241134,-30.0656638016321,0.));
#20793=CARTESIAN_POINT('Ctrl Pts',(25.8779535511027,-30.1563500154165,0.));
#20794=CARTESIAN_POINT('Ctrl Pts',(25.9137466853317,-30.2474530144827,0.));
#20795=CARTESIAN_POINT('Ctrl Pts',(25.9489196635424,-30.3389466074503,0.));
#20796=CARTESIAN_POINT('Ctrl Pts',(25.9834942765902,-30.4308118142473,0.));
#20797=CARTESIAN_POINT('Ctrl Pts',(26.0174801292225,-30.5230388264271,0.));
#20798=CARTESIAN_POINT('Ctrl Pts',(26.0508796503166,-30.6156232634061,0.));
#20799=CARTESIAN_POINT('Ctrl Pts',(26.0836911730968,-30.7085638682391,0.));
#20800=CARTESIAN_POINT('Ctrl Pts',(26.1159125093178,-30.8018598357461,0.));
#20801=CARTESIAN_POINT('Ctrl Pts',(26.1475450294082,-30.8955077633644,0.));
#20802=CARTESIAN_POINT('Ctrl Pts',(26.1785946616165,-30.9895009017073,0.));
#20803=CARTESIAN_POINT('Ctrl Pts',(26.2090698085494,-31.0838307058369,0.));
#20804=CARTESIAN_POINT('Ctrl Pts',(26.2389800738214,-31.1784877826858,0.));
#20805=CARTESIAN_POINT('Ctrl Pts',(26.2683347859175,-31.2734629900041,0.));
#20806=CARTESIAN_POINT('Ctrl Pts',(26.2971413115295,-31.3687486937246,0.));
#20807=CARTESIAN_POINT('Ctrl Pts',(26.3254046890485,-31.4643390378084,0.));
#20808=CARTESIAN_POINT('Ctrl Pts',(26.353128528169,-31.5602292672984,0.));
#20809=CARTESIAN_POINT('Ctrl Pts',(26.3803155790949,-31.6564152990236,0.));
#20810=CARTESIAN_POINT('Ctrl Pts',(26.4069683862784,-31.7528932299312,0.));
#20811=CARTESIAN_POINT('Ctrl Pts',(26.433090040836,-31.849658771403,0.));
#20812=CARTESIAN_POINT('Ctrl Pts',(26.4586843683627,-31.9467071093816,0.));
#20813=CARTESIAN_POINT('Ctrl Pts',(26.4837555495616,-32.0440331917233,0.));
#20814=CARTESIAN_POINT('Ctrl Pts',(26.5083078928862,-32.1416319023705,0.));
#20815=CARTESIAN_POINT('Ctrl Pts',(26.5323455701117,-32.2394982626669,0.));
#20816=CARTESIAN_POINT('Ctrl Pts',(26.555872320036,-32.3376276606981,0.));
#20817=CARTESIAN_POINT('Ctrl Pts',(26.5788913672813,-32.4360159072985,0.));
#20818=CARTESIAN_POINT('Ctrl Pts',(26.6014055904817,-32.5346590925498,0.));
#20819=CARTESIAN_POINT('Ctrl Pts',(26.6234176311244,-32.6335534898936,0.));
#20820=CARTESIAN_POINT('Ctrl Pts',(26.6449300199763,-32.7326954489334,0.));
#20821=CARTESIAN_POINT('Ctrl Pts',(26.6659453236976,-32.8320812678271,0.));
#20822=CARTESIAN_POINT('Ctrl Pts',(26.6864661988934,-32.9317071576181,0.));
#20823=CARTESIAN_POINT('Ctrl Pts',(26.7064953106254,-33.03156933761,0.));
#20824=CARTESIAN_POINT('Ctrl Pts',(26.7260352861618,-33.131664100194,0.));
#20825=CARTESIAN_POINT('Ctrl Pts',(26.7450886617884,-33.231987878652,0.));
#20826=CARTESIAN_POINT('Ctrl Pts',(26.7636578270526,-33.3325373307046,0.));
#20827=CARTESIAN_POINT('Ctrl Pts',(26.7817450041181,-33.4333093513694,0.));
#20828=CARTESIAN_POINT('Ctrl Pts',(26.7993522966985,-33.5343009499673,0.));
#20829=CARTESIAN_POINT('Ctrl Pts',(26.8164817280846,-33.6355091508895,0.));
#20830=CARTESIAN_POINT('Ctrl Pts',(26.8331352836666,-33.7369308933173,0.));
#20831=CARTESIAN_POINT('Ctrl Pts',(26.8493149627661,-33.838562905895,0.));
#20832=CARTESIAN_POINT('Ctrl Pts',(26.8650228056313,-33.9404016650487,0.));
#20833=CARTESIAN_POINT('Ctrl Pts',(26.880260834701,-34.0424436187397,0.));
#20834=CARTESIAN_POINT('Ctrl Pts',(26.8950310138939,-34.1446853651051,0.));
#20835=CARTESIAN_POINT('Ctrl Pts',(26.9093352037262,-34.2471238425419,0.));
#20836=CARTESIAN_POINT('Ctrl Pts',(26.9231751225177,-34.3497565255724,0.));
#20837=CARTESIAN_POINT('Ctrl Pts',(26.9392277420461,-34.4731465943772,0.));
#20838=CARTESIAN_POINT('Ctrl Pts',(26.9520281195269,-34.5762105502273,0.));
#20839=CARTESIAN_POINT('Ctrl Pts',(26.9619003236529,-34.6588137898952,0.));
#20840=CARTESIAN_POINT('Ctrl Pts',(26.9690976283147,-34.7208516760814,0.));
#20841=CARTESIAN_POINT('Ctrl Pts',(26.9738038986838,-34.7622482477091,0.));
#20842=CARTESIAN_POINT('',(26.9738038986839,-34.762248247709,15.));
#20843=CARTESIAN_POINT('Ctrl Pts',(26.9738038986838,-34.7622482477091,15.));
#20844=CARTESIAN_POINT('Ctrl Pts',(26.9714507634922,-34.7415499619104,15.));
#20845=CARTESIAN_POINT('Ctrl Pts',(26.9666985267608,-34.700172380686,15.));
#20846=CARTESIAN_POINT('Ctrl Pts',(26.9594322726214,-34.6381629799782,15.));
#20847=CARTESIAN_POINT('Ctrl Pts',(26.9494680440307,-34.5555977590573,15.));
#20848=CARTESIAN_POINT('Ctrl Pts',(26.936552305458,-34.4525815829097,15.));
#20849=CARTESIAN_POINT('Ctrl Pts',(26.9231751225177,-34.3497565255724,15.));
#20850=CARTESIAN_POINT('Ctrl Pts',(26.9093352037262,-34.2471238425419,15.));
#20851=CARTESIAN_POINT('Ctrl Pts',(26.8950310138939,-34.1446853651051,15.));
#20852=CARTESIAN_POINT('Ctrl Pts',(26.880260834701,-34.0424436187397,15.));
#20853=CARTESIAN_POINT('Ctrl Pts',(26.8650228056313,-33.9404016650487,15.));
#20854=CARTESIAN_POINT('Ctrl Pts',(26.8493149627661,-33.838562905895,15.));
#20855=CARTESIAN_POINT('Ctrl Pts',(26.8331352836666,-33.7369308933173,15.));
#20856=CARTESIAN_POINT('Ctrl Pts',(26.8164817280846,-33.6355091508895,15.));
#20857=CARTESIAN_POINT('Ctrl Pts',(26.7993522966985,-33.5343009499673,15.));
#20858=CARTESIAN_POINT('Ctrl Pts',(26.7817450041181,-33.4333093513694,15.));
#20859=CARTESIAN_POINT('Ctrl Pts',(26.7636578270526,-33.3325373307046,15.));
#20860=CARTESIAN_POINT('Ctrl Pts',(26.7450886617884,-33.231987878652,15.));
#20861=CARTESIAN_POINT('Ctrl Pts',(26.7260352861618,-33.131664100194,15.));
#20862=CARTESIAN_POINT('Ctrl Pts',(26.7064953106254,-33.03156933761,15.));
#20863=CARTESIAN_POINT('Ctrl Pts',(26.6864661988934,-32.9317071576181,15.));
#20864=CARTESIAN_POINT('Ctrl Pts',(26.6659453236976,-32.8320812678271,15.));
#20865=CARTESIAN_POINT('Ctrl Pts',(26.6449300199763,-32.7326954489334,15.));
#20866=CARTESIAN_POINT('Ctrl Pts',(26.6234176311244,-32.6335534898936,15.));
#20867=CARTESIAN_POINT('Ctrl Pts',(26.6014055904817,-32.5346590925498,15.));
#20868=CARTESIAN_POINT('Ctrl Pts',(26.5788913672813,-32.4360159072985,15.));
#20869=CARTESIAN_POINT('Ctrl Pts',(26.555872320036,-32.3376276606981,15.));
#20870=CARTESIAN_POINT('Ctrl Pts',(26.5323455701117,-32.2394982626669,15.));
#20871=CARTESIAN_POINT('Ctrl Pts',(26.5083078928862,-32.1416319023705,15.));
#20872=CARTESIAN_POINT('Ctrl Pts',(26.4837555495616,-32.0440331917233,15.));
#20873=CARTESIAN_POINT('Ctrl Pts',(26.4586843683627,-31.9467071093816,15.));
#20874=CARTESIAN_POINT('Ctrl Pts',(26.433090040836,-31.849658771403,15.));
#20875=CARTESIAN_POINT('Ctrl Pts',(26.4069683862784,-31.7528932299312,15.));
#20876=CARTESIAN_POINT('Ctrl Pts',(26.3803155790949,-31.6564152990236,15.));
#20877=CARTESIAN_POINT('Ctrl Pts',(26.353128528169,-31.5602292672984,15.));
#20878=CARTESIAN_POINT('Ctrl Pts',(26.3254046890485,-31.4643390378084,15.));
#20879=CARTESIAN_POINT('Ctrl Pts',(26.2971413115295,-31.3687486937246,15.));
#20880=CARTESIAN_POINT('Ctrl Pts',(26.2683347859175,-31.2734629900041,15.));
#20881=CARTESIAN_POINT('Ctrl Pts',(26.2389800738214,-31.1784877826858,15.));
#20882=CARTESIAN_POINT('Ctrl Pts',(26.2090698085494,-31.0838307058369,15.));
#20883=CARTESIAN_POINT('Ctrl Pts',(26.1785946616165,-30.9895009017073,15.));
#20884=CARTESIAN_POINT('Ctrl Pts',(26.1475450294082,-30.8955077633644,15.));
#20885=CARTESIAN_POINT('Ctrl Pts',(26.1159125093178,-30.8018598357461,15.));
#20886=CARTESIAN_POINT('Ctrl Pts',(26.0836911730968,-30.7085638682391,15.));
#20887=CARTESIAN_POINT('Ctrl Pts',(26.0508796503166,-30.6156232634061,15.));
#20888=CARTESIAN_POINT('Ctrl Pts',(26.0174801292225,-30.5230388264271,15.));
#20889=CARTESIAN_POINT('Ctrl Pts',(25.9834942765902,-30.4308118142473,15.));
#20890=CARTESIAN_POINT('Ctrl Pts',(25.9489196635424,-30.3389466074503,15.));
#20891=CARTESIAN_POINT('Ctrl Pts',(25.9137466853317,-30.2474530144827,15.));
#20892=CARTESIAN_POINT('Ctrl Pts',(25.8779535511027,-30.1563500154165,15.));
#20893=CARTESIAN_POINT('Ctrl Pts',(25.8415089241134,-30.0656638016321,15.));
#20894=CARTESIAN_POINT('Ctrl Pts',(25.8043812318214,-29.9754208429384,15.));
#20895=CARTESIAN_POINT('Ctrl Pts',(25.7665469042913,-29.8856417535786,15.));
#20896=CARTESIAN_POINT('Ctrl Pts',(25.7279973711305,-29.7963360859334,15.));
#20897=CARTESIAN_POINT('Ctrl Pts',(25.6887507922748,-29.7074935910931,15.));
#20898=CARTESIAN_POINT('Ctrl Pts',(25.6488438125835,-29.6190903904157,15.));
#20899=CARTESIAN_POINT('Ctrl Pts',(25.6083094352667,-29.5311055094509,15.));
#20900=CARTESIAN_POINT('Ctrl Pts',(25.5671572096726,-29.443535683207,15.));
#20901=CARTESIAN_POINT('Ctrl Pts',(25.5253562922582,-29.356408021119,15.));
#20902=CARTESIAN_POINT('Ctrl Pts',(25.4828076101654,-29.2698007967907,15.));
#20903=CARTESIAN_POINT('Ctrl Pts',(25.4393679214513,-29.183825549991,15.));
#20904=CARTESIAN_POINT('Ctrl Pts',(25.3948997321278,-29.098589927237,15.));
#20905=CARTESIAN_POINT('Ctrl Pts',(25.3493168206005,-29.0141637699076,15.));
#20906=CARTESIAN_POINT('Ctrl Pts',(25.3026235249214,-28.9305499160476,15.));
#20907=CARTESIAN_POINT('Ctrl Pts',(25.2549775629725,-28.8476372998748,15.));
#20908=CARTESIAN_POINT('Ctrl Pts',(25.2066127148845,-28.7652594076549,15.));
#20909=CARTESIAN_POINT('Ctrl Pts',(25.1577170374459,-28.6832861366762,15.));
#20910=CARTESIAN_POINT('Ctrl Pts',(25.1083211582389,-28.6017081342376,15.));
#20911=CARTESIAN_POINT('Ctrl Pts',(25.0581926620043,-28.5207164321473,15.));
#20912=CARTESIAN_POINT('Ctrl Pts',(25.0066999111736,-28.4408053900206,15.));
#20913=CARTESIAN_POINT('Ctrl Pts',(24.9529811166897,-28.3626431274892,15.));
#20914=CARTESIAN_POINT('Ctrl Pts',(24.9075246543798,-28.3020534756061,15.));
#20915=CARTESIAN_POINT('Ctrl Pts',(24.8717258526943,-28.2579420132101,15.));
#20916=CARTESIAN_POINT('Ctrl Pts',(24.8470618363541,-28.2291563988796,15.));
#20917=CARTESIAN_POINT('Ctrl Pts',(24.8345302882955,-28.2149191006269,15.));
#20918=CARTESIAN_POINT('',(26.9738038986839,-34.762248247709,0.));
#20919=CARTESIAN_POINT('Origin',(6.66146233219318E-12,-9.16871631793044E-12,
0.));
#20920=CARTESIAN_POINT('',(24.725498909423,-36.3957374383337,0.));
#20921=CARTESIAN_POINT('Origin',(6.66146233219318E-12,-9.16871631793044E-12,
0.));
#20922=CARTESIAN_POINT('',(24.725498909423,-36.3957374383337,15.));
#20923=CARTESIAN_POINT('Origin',(6.66146233219318E-12,-9.16871631793044E-12,
15.));
#20924=CARTESIAN_POINT('',(24.725498909423,-36.3957374383337,0.));
#20925=CARTESIAN_POINT('Ctrl Pts',(19.1596907609891,-32.3379313568208,0.));
#20926=CARTESIAN_POINT('Ctrl Pts',(19.1596907609891,-32.3379313568208,18.));
#20927=CARTESIAN_POINT('Ctrl Pts',(19.1693587749508,-32.3542491343753,0.));
#20928=CARTESIAN_POINT('Ctrl Pts',(19.1693587749508,-32.3542491343753,18.));
#20929=CARTESIAN_POINT('Ctrl Pts',(19.1891139208368,-32.3866012518553,0.));
#20930=CARTESIAN_POINT('Ctrl Pts',(19.1891139208368,-32.3866012518553,18.));
#20931=CARTESIAN_POINT('Ctrl Pts',(19.2200039764927,-32.4342791270009,0.));
#20932=CARTESIAN_POINT('Ctrl Pts',(19.2200039764927,-32.4342791270009,18.));
#20933=CARTESIAN_POINT('Ctrl Pts',(19.2635813403783,-32.4962340238036,0.));
#20934=CARTESIAN_POINT('Ctrl Pts',(19.2635813403783,-32.4962340238036,18.));
#20935=CARTESIAN_POINT('Ctrl Pts',(19.3213180490743,-32.5714771007861,0.));
#20936=CARTESIAN_POINT('Ctrl Pts',(19.3213180490743,-32.5714771007861,18.));
#20937=CARTESIAN_POINT('Ctrl Pts',(19.381405831319,-32.6451434870609,0.));
#20938=CARTESIAN_POINT('Ctrl Pts',(19.381405831319,-32.6451434870609,18.));
#20939=CARTESIAN_POINT('Ctrl Pts',(19.4429429601189,-32.7178463324062,0.));
#20940=CARTESIAN_POINT('Ctrl Pts',(19.4429429601189,-32.7178463324062,18.));
#20941=CARTESIAN_POINT('Ctrl Pts',(19.5052640847974,-32.7900335943248,0.));
#20942=CARTESIAN_POINT('Ctrl Pts',(19.5052640847974,-32.7900335943248,18.));
#20943=CARTESIAN_POINT('Ctrl Pts',(19.5681157030437,-32.8618672807884,0.));
#20944=CARTESIAN_POINT('Ctrl Pts',(19.5681157030437,-32.8618672807884,18.));
#20945=CARTESIAN_POINT('Ctrl Pts',(19.6315161742485,-32.9333211533788,0.));
#20946=CARTESIAN_POINT('Ctrl Pts',(19.6315161742485,-32.9333211533788,18.));
#20947=CARTESIAN_POINT('Ctrl Pts',(19.6956473461873,-33.004256563411,0.));
#20948=CARTESIAN_POINT('Ctrl Pts',(19.6956473461873,-33.004256563411,18.));
#20949=CARTESIAN_POINT('Ctrl Pts',(19.7607398248651,-33.0745026283418,0.));
#20950=CARTESIAN_POINT('Ctrl Pts',(19.7607398248651,-33.0745026283418,18.));
#20951=CARTESIAN_POINT('Ctrl Pts',(19.8269479776239,-33.1439436707661,0.));
#20952=CARTESIAN_POINT('Ctrl Pts',(19.8269479776239,-33.1439436707661,18.));
#20953=CARTESIAN_POINT('Ctrl Pts',(19.8942704458546,-33.2125746879471,0.));
#20954=CARTESIAN_POINT('Ctrl Pts',(19.8942704458546,-33.2125746879471,18.));
#20955=CARTESIAN_POINT('Ctrl Pts',(19.9626141625205,-33.2804560993213,0.));
#20956=CARTESIAN_POINT('Ctrl Pts',(19.9626141625205,-33.2804560993213,18.));
#20957=CARTESIAN_POINT('Ctrl Pts',(20.0318342617212,-33.3476854048385,0.));
#20958=CARTESIAN_POINT('Ctrl Pts',(20.0318342617212,-33.3476854048385,18.));
#20959=CARTESIAN_POINT('Ctrl Pts',(20.1017803986381,-33.4143643679979,0.));
#20960=CARTESIAN_POINT('Ctrl Pts',(20.1017803986381,-33.4143643679979,18.));
#20961=CARTESIAN_POINT('Ctrl Pts',(20.1723475154533,-33.480563024813,0.));
#20962=CARTESIAN_POINT('Ctrl Pts',(20.1723475154533,-33.480563024813,18.));
#20963=CARTESIAN_POINT('Ctrl Pts',(20.243500298383,-33.5463023319603,0.));
#20964=CARTESIAN_POINT('Ctrl Pts',(20.243500298383,-33.5463023319603,18.));
#20965=CARTESIAN_POINT('Ctrl Pts',(20.3152448035297,-33.6115742164079,0.));
#20966=CARTESIAN_POINT('Ctrl Pts',(20.3152448035297,-33.6115742164079,18.));
#20967=CARTESIAN_POINT('Ctrl Pts',(20.3876111773341,-33.6763537716992,0.));
#20968=CARTESIAN_POINT('Ctrl Pts',(20.3876111773341,-33.6763537716992,18.));
#20969=CARTESIAN_POINT('Ctrl Pts',(20.4606334536183,-33.7406135254082,0.));
#20970=CARTESIAN_POINT('Ctrl Pts',(20.4606334536183,-33.7406135254082,18.));
#20971=CARTESIAN_POINT('Ctrl Pts',(20.5343269914034,-33.8043393734971,0.));
#20972=CARTESIAN_POINT('Ctrl Pts',(20.5343269914034,-33.8043393734971,18.));
#20973=CARTESIAN_POINT('Ctrl Pts',(20.6086800574386,-33.8675365150454,0.));
#20974=CARTESIAN_POINT('Ctrl Pts',(20.6086800574386,-33.8675365150454,18.));
#20975=CARTESIAN_POINT('Ctrl Pts',(20.683665762903,-33.9302209962425,0.));
#20976=CARTESIAN_POINT('Ctrl Pts',(20.683665762903,-33.9302209962425,18.));
#20977=CARTESIAN_POINT('Ctrl Pts',(20.7592491770603,-33.9924146647395,0.));
#20978=CARTESIAN_POINT('Ctrl Pts',(20.7592491770603,-33.9924146647395,18.));
#20979=CARTESIAN_POINT('Ctrl Pts',(20.8353957068415,-34.0541392299678,0.));
#20980=CARTESIAN_POINT('Ctrl Pts',(20.8353957068415,-34.0541392299678,18.));
#20981=CARTESIAN_POINT('Ctrl Pts',(20.9120805673809,-34.1154095510973,0.));
#20982=CARTESIAN_POINT('Ctrl Pts',(20.9120805673809,-34.1154095510973,18.));
#20983=CARTESIAN_POINT('Ctrl Pts',(20.9892914622612,-34.176231731809,0.));
#20984=CARTESIAN_POINT('Ctrl Pts',(20.9892914622612,-34.176231731809,18.));
#20985=CARTESIAN_POINT('Ctrl Pts',(21.0670234747355,-34.2366067284279,0.));
#20986=CARTESIAN_POINT('Ctrl Pts',(21.0670234747355,-34.2366067284279,18.));
#20987=CARTESIAN_POINT('Ctrl Pts',(21.1452759244399,-34.2965325673384,0.));
#20988=CARTESIAN_POINT('Ctrl Pts',(21.1452759244399,-34.2965325673384,18.));
#20989=CARTESIAN_POINT('Ctrl Pts',(21.2240487218078,-34.3560069185815,0.));
#20990=CARTESIAN_POINT('Ctrl Pts',(21.2240487218078,-34.3560069185815,18.));
#20991=CARTESIAN_POINT('Ctrl Pts',(21.3033382073239,-34.4150300340623,0.));
#20992=CARTESIAN_POINT('Ctrl Pts',(21.3033382073239,-34.4150300340623,18.));
#20993=CARTESIAN_POINT('Ctrl Pts',(21.3831361300104,-34.4736054662052,0.));
#20994=CARTESIAN_POINT('Ctrl Pts',(21.3831361300104,-34.4736054662052,18.));
#20995=CARTESIAN_POINT('Ctrl Pts',(21.4634317666004,-34.5317385658329,0.));
#20996=CARTESIAN_POINT('Ctrl Pts',(21.4634317666004,-34.5317385658329,18.));
#20997=CARTESIAN_POINT('Ctrl Pts',(21.5442132160757,-34.5894355639082,0.));
#20998=CARTESIAN_POINT('Ctrl Pts',(21.5442132160757,-34.5894355639082,18.));
#20999=CARTESIAN_POINT('Ctrl Pts',(21.6254689009796,-34.6467025072367,0.));
#21000=CARTESIAN_POINT('Ctrl Pts',(21.6254689009796,-34.6467025072367,18.));
#21001=CARTESIAN_POINT('Ctrl Pts',(21.7071892844497,-34.7035440429025,0.));
#21002=CARTESIAN_POINT('Ctrl Pts',(21.7071892844497,-34.7035440429025,18.));
#21003=CARTESIAN_POINT('Ctrl Pts',(21.7893672401137,-34.7599631530844,0.));
#21004=CARTESIAN_POINT('Ctrl Pts',(21.7893672401137,-34.7599631530844,18.));
#21005=CARTESIAN_POINT('Ctrl Pts',(21.8719971302817,-34.8159618014436,0.));
#21006=CARTESIAN_POINT('Ctrl Pts',(21.8719971302817,-34.8159618014436,18.));
#21007=CARTESIAN_POINT('Ctrl Pts',(21.9550742217675,-34.8715413418101,0.));
#21008=CARTESIAN_POINT('Ctrl Pts',(21.9550742217675,-34.8715413418101,18.));
#21009=CARTESIAN_POINT('Ctrl Pts',(22.0385940162683,-34.9267029879922,0.));
#21010=CARTESIAN_POINT('Ctrl Pts',(22.0385940162683,-34.9267029879922,18.));
#21011=CARTESIAN_POINT('Ctrl Pts',(22.1225514798584,-34.9814483545602,0.));
#21012=CARTESIAN_POINT('Ctrl Pts',(22.1225514798584,-34.9814483545602,18.));
#21013=CARTESIAN_POINT('Ctrl Pts',(22.2069408519232,-35.0357795922459,0.));
#21014=CARTESIAN_POINT('Ctrl Pts',(22.2069408519232,-35.0357795922459,18.));
#21015=CARTESIAN_POINT('Ctrl Pts',(22.2917560356802,-35.0896991159359,0.));
#21016=CARTESIAN_POINT('Ctrl Pts',(22.2917560356802,-35.0896991159359,18.));
#21017=CARTESIAN_POINT('Ctrl Pts',(22.3769908340843,-35.1432094422642,0.));
#21018=CARTESIAN_POINT('Ctrl Pts',(22.3769908340843,-35.1432094422642,18.));
#21019=CARTESIAN_POINT('Ctrl Pts',(22.4626392230023,-35.1963130003353,0.));
#21020=CARTESIAN_POINT('Ctrl Pts',(22.4626392230023,-35.1963130003353,18.));
#21021=CARTESIAN_POINT('Ctrl Pts',(22.5486956608909,-35.2490119207975,0.));
#21022=CARTESIAN_POINT('Ctrl Pts',(22.5486956608909,-35.2490119207975,18.));
#21023=CARTESIAN_POINT('Ctrl Pts',(22.635155167154,-35.3013079759253,0.));
#21024=CARTESIAN_POINT('Ctrl Pts',(22.635155167154,-35.3013079759253,18.));
#21025=CARTESIAN_POINT('Ctrl Pts',(22.7220131336912,-35.3532026952313,0.));
#21026=CARTESIAN_POINT('Ctrl Pts',(22.7220131336912,-35.3532026952313,18.));
#21027=CARTESIAN_POINT('Ctrl Pts',(22.8092652000706,-35.4046974393492,0.));
#21028=CARTESIAN_POINT('Ctrl Pts',(22.8092652000706,-35.4046974393492,18.));
#21029=CARTESIAN_POINT('Ctrl Pts',(22.8969071125089,-35.4557934871468,0.));
#21030=CARTESIAN_POINT('Ctrl Pts',(22.8969071125089,-35.4557934871468,18.));
#21031=CARTESIAN_POINT('Ctrl Pts',(22.9849345572033,-35.5064921357308,0.));
#21032=CARTESIAN_POINT('Ctrl Pts',(22.9849345572033,-35.5064921357308,18.));
#21033=CARTESIAN_POINT('Ctrl Pts',(23.0733431097058,-35.5567947408311,0.));
#21034=CARTESIAN_POINT('Ctrl Pts',(23.0733431097058,-35.5567947408311,18.));
#21035=CARTESIAN_POINT('Ctrl Pts',(23.1621283508111,-35.6067026687722,0.));
#21036=CARTESIAN_POINT('Ctrl Pts',(23.1621283508111,-35.6067026687722,18.));
#21037=CARTESIAN_POINT('Ctrl Pts',(23.2512859425032,-35.6562172725207,0.));
#21038=CARTESIAN_POINT('Ctrl Pts',(23.2512859425032,-35.6562172725207,18.));
#21039=CARTESIAN_POINT('Ctrl Pts',(23.3408117088761,-35.7053398620512,0.));
#21040=CARTESIAN_POINT('Ctrl Pts',(23.3408117088761,-35.7053398620512,18.));
#21041=CARTESIAN_POINT('Ctrl Pts',(23.4307017328227,-35.7540716771372,0.));
#21042=CARTESIAN_POINT('Ctrl Pts',(23.4307017328227,-35.7540716771372,18.));
#21043=CARTESIAN_POINT('Ctrl Pts',(23.5209523746427,-35.8024138716897,0.));
#21044=CARTESIAN_POINT('Ctrl Pts',(23.5209523746427,-35.8024138716897,18.));
#21045=CARTESIAN_POINT('Ctrl Pts',(23.611560139948,-35.8503675222884,0.));
#21046=CARTESIAN_POINT('Ctrl Pts',(23.611560139948,-35.8503675222884,18.));
#21047=CARTESIAN_POINT('Ctrl Pts',(23.7025215735353,-35.8979336336837,0.));
#21048=CARTESIAN_POINT('Ctrl Pts',(23.7025215735353,-35.8979336336837,18.));
#21049=CARTESIAN_POINT('Ctrl Pts',(23.7938331508737,-35.9451131482488,0.));
#21050=CARTESIAN_POINT('Ctrl Pts',(23.7938331508737,-35.9451131482488,18.));
#21051=CARTESIAN_POINT('Ctrl Pts',(23.8854911428946,-35.991906956547,0.));
#21052=CARTESIAN_POINT('Ctrl Pts',(23.8854911428946,-35.991906956547,18.));
#21053=CARTESIAN_POINT('Ctrl Pts',(23.9774915680089,-36.0383159101253,0.));
#21054=CARTESIAN_POINT('Ctrl Pts',(23.9774915680089,-36.0383159101253,18.));
#21055=CARTESIAN_POINT('Ctrl Pts',(24.0698304230588,-36.0843408347974,0.));
#21056=CARTESIAN_POINT('Ctrl Pts',(24.0698304230588,-36.0843408347974,18.));
#21057=CARTESIAN_POINT('Ctrl Pts',(24.1625038657964,-36.1299825471271,0.));
#21058=CARTESIAN_POINT('Ctrl Pts',(24.1625038657964,-36.1299825471271,18.));
#21059=CARTESIAN_POINT('Ctrl Pts',(24.2555084095331,-36.1752418704833,0.));
#21060=CARTESIAN_POINT('Ctrl Pts',(24.2555084095331,-36.1752418704833,18.));
#21061=CARTESIAN_POINT('Ctrl Pts',(24.3488411214068,-36.2201196586696,0.));
#21062=CARTESIAN_POINT('Ctrl Pts',(24.3488411214068,-36.2201196586696,18.));
#21063=CARTESIAN_POINT('Ctrl Pts',(24.4424997853604,-36.2646168058395,0.));
#21064=CARTESIAN_POINT('Ctrl Pts',(24.4424997853604,-36.2646168058395,18.));
#21065=CARTESIAN_POINT('Ctrl Pts',(24.5364828082556,-36.308734152297,0.));
#21066=CARTESIAN_POINT('Ctrl Pts',(24.5364828082556,-36.308734152297,18.));
#21067=CARTESIAN_POINT('Ctrl Pts',(24.6119278836614,-36.3437247532369,0.));
#21068=CARTESIAN_POINT('Ctrl Pts',(24.6119278836614,-36.3437247532369,18.));
#21069=CARTESIAN_POINT('Ctrl Pts',(24.6686569322615,-36.369797330215,0.));
#21070=CARTESIAN_POINT('Ctrl Pts',(24.6686569322615,-36.369797330215,18.));
#21071=CARTESIAN_POINT('Ctrl Pts',(24.7065408286023,-36.3871033517098,0.));
#21072=CARTESIAN_POINT('Ctrl Pts',(24.7065408286023,-36.3871033517098,18.));
#21073=CARTESIAN_POINT('Ctrl Pts',(24.725498909423,-36.3957374383337,0.));
#21074=CARTESIAN_POINT('Ctrl Pts',(24.725498909423,-36.3957374383337,18.));
#21075=CARTESIAN_POINT('Ctrl Pts',(19.1596907609891,-32.3379313568208,0.));
#21076=CARTESIAN_POINT('Ctrl Pts',(19.1693587749508,-32.3542491343753,0.));
#21077=CARTESIAN_POINT('Ctrl Pts',(19.1891139208368,-32.3866012518553,0.));
#21078=CARTESIAN_POINT('Ctrl Pts',(19.2200039764927,-32.4342791270009,0.));
#21079=CARTESIAN_POINT('Ctrl Pts',(19.2635813403783,-32.4962340238036,0.));
#21080=CARTESIAN_POINT('Ctrl Pts',(19.3213180490743,-32.5714771007861,0.));
#21081=CARTESIAN_POINT('Ctrl Pts',(19.381405831319,-32.6451434870609,0.));
#21082=CARTESIAN_POINT('Ctrl Pts',(19.4429429601189,-32.7178463324062,0.));
#21083=CARTESIAN_POINT('Ctrl Pts',(19.5052640847974,-32.7900335943248,0.));
#21084=CARTESIAN_POINT('Ctrl Pts',(19.5681157030437,-32.8618672807884,0.));
#21085=CARTESIAN_POINT('Ctrl Pts',(19.6315161742485,-32.9333211533788,0.));
#21086=CARTESIAN_POINT('Ctrl Pts',(19.6956473461873,-33.004256563411,0.));
#21087=CARTESIAN_POINT('Ctrl Pts',(19.7607398248651,-33.0745026283418,0.));
#21088=CARTESIAN_POINT('Ctrl Pts',(19.8269479776239,-33.1439436707661,0.));
#21089=CARTESIAN_POINT('Ctrl Pts',(19.8942704458546,-33.2125746879471,0.));
#21090=CARTESIAN_POINT('Ctrl Pts',(19.9626141625205,-33.2804560993213,0.));
#21091=CARTESIAN_POINT('Ctrl Pts',(20.0318342617212,-33.3476854048385,0.));
#21092=CARTESIAN_POINT('Ctrl Pts',(20.1017803986381,-33.4143643679979,0.));
#21093=CARTESIAN_POINT('Ctrl Pts',(20.1723475154533,-33.480563024813,0.));
#21094=CARTESIAN_POINT('Ctrl Pts',(20.243500298383,-33.5463023319603,0.));
#21095=CARTESIAN_POINT('Ctrl Pts',(20.3152448035297,-33.6115742164079,0.));
#21096=CARTESIAN_POINT('Ctrl Pts',(20.3876111773341,-33.6763537716992,0.));
#21097=CARTESIAN_POINT('Ctrl Pts',(20.4606334536183,-33.7406135254082,0.));
#21098=CARTESIAN_POINT('Ctrl Pts',(20.5343269914034,-33.8043393734971,0.));
#21099=CARTESIAN_POINT('Ctrl Pts',(20.6086800574386,-33.8675365150454,0.));
#21100=CARTESIAN_POINT('Ctrl Pts',(20.683665762903,-33.9302209962425,0.));
#21101=CARTESIAN_POINT('Ctrl Pts',(20.7592491770603,-33.9924146647395,0.));
#21102=CARTESIAN_POINT('Ctrl Pts',(20.8353957068415,-34.0541392299678,0.));
#21103=CARTESIAN_POINT('Ctrl Pts',(20.9120805673809,-34.1154095510973,0.));
#21104=CARTESIAN_POINT('Ctrl Pts',(20.9892914622612,-34.176231731809,0.));
#21105=CARTESIAN_POINT('Ctrl Pts',(21.0670234747355,-34.2366067284279,0.));
#21106=CARTESIAN_POINT('Ctrl Pts',(21.1452759244399,-34.2965325673384,0.));
#21107=CARTESIAN_POINT('Ctrl Pts',(21.2240487218078,-34.3560069185815,0.));
#21108=CARTESIAN_POINT('Ctrl Pts',(21.3033382073239,-34.4150300340623,0.));
#21109=CARTESIAN_POINT('Ctrl Pts',(21.3831361300104,-34.4736054662052,0.));
#21110=CARTESIAN_POINT('Ctrl Pts',(21.4634317666004,-34.5317385658329,0.));
#21111=CARTESIAN_POINT('Ctrl Pts',(21.5442132160757,-34.5894355639082,0.));
#21112=CARTESIAN_POINT('Ctrl Pts',(21.6254689009796,-34.6467025072367,0.));
#21113=CARTESIAN_POINT('Ctrl Pts',(21.7071892844497,-34.7035440429025,0.));
#21114=CARTESIAN_POINT('Ctrl Pts',(21.7893672401137,-34.7599631530844,0.));
#21115=CARTESIAN_POINT('Ctrl Pts',(21.8719971302817,-34.8159618014436,0.));
#21116=CARTESIAN_POINT('Ctrl Pts',(21.9550742217675,-34.8715413418101,0.));
#21117=CARTESIAN_POINT('Ctrl Pts',(22.0385940162683,-34.9267029879922,0.));
#21118=CARTESIAN_POINT('Ctrl Pts',(22.1225514798584,-34.9814483545602,0.));
#21119=CARTESIAN_POINT('Ctrl Pts',(22.2069408519232,-35.0357795922459,0.));
#21120=CARTESIAN_POINT('Ctrl Pts',(22.2917560356802,-35.0896991159359,0.));
#21121=CARTESIAN_POINT('Ctrl Pts',(22.3769908340843,-35.1432094422642,0.));
#21122=CARTESIAN_POINT('Ctrl Pts',(22.4626392230023,-35.1963130003353,0.));
#21123=CARTESIAN_POINT('Ctrl Pts',(22.5486956608909,-35.2490119207975,0.));
#21124=CARTESIAN_POINT('Ctrl Pts',(22.635155167154,-35.3013079759253,0.));
#21125=CARTESIAN_POINT('Ctrl Pts',(22.7220131336912,-35.3532026952313,0.));
#21126=CARTESIAN_POINT('Ctrl Pts',(22.8092652000706,-35.4046974393492,0.));
#21127=CARTESIAN_POINT('Ctrl Pts',(22.8969071125089,-35.4557934871468,0.));
#21128=CARTESIAN_POINT('Ctrl Pts',(22.9849345572033,-35.5064921357308,0.));
#21129=CARTESIAN_POINT('Ctrl Pts',(23.0733431097058,-35.5567947408311,0.));
#21130=CARTESIAN_POINT('Ctrl Pts',(23.1621283508111,-35.6067026687722,0.));
#21131=CARTESIAN_POINT('Ctrl Pts',(23.2512859425032,-35.6562172725207,0.));
#21132=CARTESIAN_POINT('Ctrl Pts',(23.3408117088761,-35.7053398620512,0.));
#21133=CARTESIAN_POINT('Ctrl Pts',(23.4307017328227,-35.7540716771372,0.));
#21134=CARTESIAN_POINT('Ctrl Pts',(23.5209523746427,-35.8024138716897,0.));
#21135=CARTESIAN_POINT('Ctrl Pts',(23.611560139948,-35.8503675222884,0.));
#21136=CARTESIAN_POINT('Ctrl Pts',(23.7025215735353,-35.8979336336837,0.));
#21137=CARTESIAN_POINT('Ctrl Pts',(23.7938331508737,-35.9451131482488,0.));
#21138=CARTESIAN_POINT('Ctrl Pts',(23.8854911428946,-35.991906956547,0.));
#21139=CARTESIAN_POINT('Ctrl Pts',(23.9774915680089,-36.0383159101253,0.));
#21140=CARTESIAN_POINT('Ctrl Pts',(24.0698304230588,-36.0843408347974,0.));
#21141=CARTESIAN_POINT('Ctrl Pts',(24.1625038657964,-36.1299825471271,0.));
#21142=CARTESIAN_POINT('Ctrl Pts',(24.2555084095331,-36.1752418704833,0.));
#21143=CARTESIAN_POINT('Ctrl Pts',(24.3488411214068,-36.2201196586696,0.));
#21144=CARTESIAN_POINT('Ctrl Pts',(24.4612315181511,-36.2735162352735,0.));
#21145=CARTESIAN_POINT('Ctrl Pts',(24.5552956307817,-36.3175386315529,0.));
#21146=CARTESIAN_POINT('Ctrl Pts',(24.630805301288,-36.3524534604649,0.));
#21147=CARTESIAN_POINT('Ctrl Pts',(24.6875827477483,-36.37846926509,0.));
#21148=CARTESIAN_POINT('Ctrl Pts',(24.725498909423,-36.3957374383337,0.));
#21149=CARTESIAN_POINT('Ctrl Pts',(19.1596907609891,-32.3379313568208,15.));
#21150=CARTESIAN_POINT('Ctrl Pts',(19.1693587749508,-32.3542491343753,15.));
#21151=CARTESIAN_POINT('Ctrl Pts',(19.1891139208368,-32.3866012518553,15.));
#21152=CARTESIAN_POINT('Ctrl Pts',(19.2200039764927,-32.4342791270009,15.));
#21153=CARTESIAN_POINT('Ctrl Pts',(19.2635813403783,-32.4962340238036,15.));
#21154=CARTESIAN_POINT('Ctrl Pts',(19.3213180490743,-32.5714771007861,15.));
#21155=CARTESIAN_POINT('Ctrl Pts',(19.381405831319,-32.6451434870609,15.));
#21156=CARTESIAN_POINT('Ctrl Pts',(19.4429429601189,-32.7178463324062,15.));
#21157=CARTESIAN_POINT('Ctrl Pts',(19.5052640847974,-32.7900335943248,15.));
#21158=CARTESIAN_POINT('Ctrl Pts',(19.5681157030437,-32.8618672807884,15.));
#21159=CARTESIAN_POINT('Ctrl Pts',(19.6315161742485,-32.9333211533788,15.));
#21160=CARTESIAN_POINT('Ctrl Pts',(19.6956473461873,-33.004256563411,15.));
#21161=CARTESIAN_POINT('Ctrl Pts',(19.7607398248651,-33.0745026283418,15.));
#21162=CARTESIAN_POINT('Ctrl Pts',(19.8269479776239,-33.1439436707661,15.));
#21163=CARTESIAN_POINT('Ctrl Pts',(19.8942704458546,-33.2125746879471,15.));
#21164=CARTESIAN_POINT('Ctrl Pts',(19.9626141625205,-33.2804560993213,15.));
#21165=CARTESIAN_POINT('Ctrl Pts',(20.0318342617212,-33.3476854048385,15.));
#21166=CARTESIAN_POINT('Ctrl Pts',(20.1017803986381,-33.4143643679979,15.));
#21167=CARTESIAN_POINT('Ctrl Pts',(20.1723475154533,-33.480563024813,15.));
#21168=CARTESIAN_POINT('Ctrl Pts',(20.243500298383,-33.5463023319603,15.));
#21169=CARTESIAN_POINT('Ctrl Pts',(20.3152448035297,-33.6115742164079,15.));
#21170=CARTESIAN_POINT('Ctrl Pts',(20.3876111773341,-33.6763537716992,15.));
#21171=CARTESIAN_POINT('Ctrl Pts',(20.4606334536183,-33.7406135254082,15.));
#21172=CARTESIAN_POINT('Ctrl Pts',(20.5343269914034,-33.8043393734971,15.));
#21173=CARTESIAN_POINT('Ctrl Pts',(20.6086800574386,-33.8675365150454,15.));
#21174=CARTESIAN_POINT('Ctrl Pts',(20.683665762903,-33.9302209962425,15.));
#21175=CARTESIAN_POINT('Ctrl Pts',(20.7592491770603,-33.9924146647395,15.));
#21176=CARTESIAN_POINT('Ctrl Pts',(20.8353957068415,-34.0541392299678,15.));
#21177=CARTESIAN_POINT('Ctrl Pts',(20.9120805673809,-34.1154095510973,15.));
#21178=CARTESIAN_POINT('Ctrl Pts',(20.9892914622612,-34.176231731809,15.));
#21179=CARTESIAN_POINT('Ctrl Pts',(21.0670234747355,-34.2366067284279,15.));
#21180=CARTESIAN_POINT('Ctrl Pts',(21.1452759244399,-34.2965325673384,15.));
#21181=CARTESIAN_POINT('Ctrl Pts',(21.2240487218078,-34.3560069185815,15.));
#21182=CARTESIAN_POINT('Ctrl Pts',(21.3033382073239,-34.4150300340623,15.));
#21183=CARTESIAN_POINT('Ctrl Pts',(21.3831361300104,-34.4736054662052,15.));
#21184=CARTESIAN_POINT('Ctrl Pts',(21.4634317666004,-34.5317385658329,15.));
#21185=CARTESIAN_POINT('Ctrl Pts',(21.5442132160757,-34.5894355639082,15.));
#21186=CARTESIAN_POINT('Ctrl Pts',(21.6254689009796,-34.6467025072367,15.));
#21187=CARTESIAN_POINT('Ctrl Pts',(21.7071892844497,-34.7035440429025,15.));
#21188=CARTESIAN_POINT('Ctrl Pts',(21.7893672401137,-34.7599631530844,15.));
#21189=CARTESIAN_POINT('Ctrl Pts',(21.8719971302817,-34.8159618014436,15.));
#21190=CARTESIAN_POINT('Ctrl Pts',(21.9550742217675,-34.8715413418101,15.));
#21191=CARTESIAN_POINT('Ctrl Pts',(22.0385940162683,-34.9267029879922,15.));
#21192=CARTESIAN_POINT('Ctrl Pts',(22.1225514798584,-34.9814483545602,15.));
#21193=CARTESIAN_POINT('Ctrl Pts',(22.2069408519232,-35.0357795922459,15.));
#21194=CARTESIAN_POINT('Ctrl Pts',(22.2917560356802,-35.0896991159359,15.));
#21195=CARTESIAN_POINT('Ctrl Pts',(22.3769908340843,-35.1432094422642,15.));
#21196=CARTESIAN_POINT('Ctrl Pts',(22.4626392230023,-35.1963130003353,15.));
#21197=CARTESIAN_POINT('Ctrl Pts',(22.5486956608909,-35.2490119207975,15.));
#21198=CARTESIAN_POINT('Ctrl Pts',(22.635155167154,-35.3013079759253,15.));
#21199=CARTESIAN_POINT('Ctrl Pts',(22.7220131336912,-35.3532026952313,15.));
#21200=CARTESIAN_POINT('Ctrl Pts',(22.8092652000706,-35.4046974393492,15.));
#21201=CARTESIAN_POINT('Ctrl Pts',(22.8969071125089,-35.4557934871468,15.));
#21202=CARTESIAN_POINT('Ctrl Pts',(22.9849345572033,-35.5064921357308,15.));
#21203=CARTESIAN_POINT('Ctrl Pts',(23.0733431097058,-35.5567947408311,15.));
#21204=CARTESIAN_POINT('Ctrl Pts',(23.1621283508111,-35.6067026687722,15.));
#21205=CARTESIAN_POINT('Ctrl Pts',(23.2512859425032,-35.6562172725207,15.));
#21206=CARTESIAN_POINT('Ctrl Pts',(23.3408117088761,-35.7053398620512,15.));
#21207=CARTESIAN_POINT('Ctrl Pts',(23.4307017328227,-35.7540716771372,15.));
#21208=CARTESIAN_POINT('Ctrl Pts',(23.5209523746427,-35.8024138716897,15.));
#21209=CARTESIAN_POINT('Ctrl Pts',(23.611560139948,-35.8503675222884,15.));
#21210=CARTESIAN_POINT('Ctrl Pts',(23.7025215735353,-35.8979336336837,15.));
#21211=CARTESIAN_POINT('Ctrl Pts',(23.7938331508737,-35.9451131482488,15.));
#21212=CARTESIAN_POINT('Ctrl Pts',(23.8854911428946,-35.991906956547,15.));
#21213=CARTESIAN_POINT('Ctrl Pts',(23.9774915680089,-36.0383159101253,15.));
#21214=CARTESIAN_POINT('Ctrl Pts',(24.0698304230588,-36.0843408347974,15.));
#21215=CARTESIAN_POINT('Ctrl Pts',(24.1625038657964,-36.1299825471271,15.));
#21216=CARTESIAN_POINT('Ctrl Pts',(24.2555084095331,-36.1752418704833,15.));
#21217=CARTESIAN_POINT('Ctrl Pts',(24.3488411214068,-36.2201196586696,15.));
#21218=CARTESIAN_POINT('Ctrl Pts',(24.4612315181511,-36.2735162352735,15.));
#21219=CARTESIAN_POINT('Ctrl Pts',(24.5552956307817,-36.3175386315529,15.));
#21220=CARTESIAN_POINT('Ctrl Pts',(24.630805301288,-36.3524534604649,15.));
#21221=CARTESIAN_POINT('Ctrl Pts',(24.6875827477483,-36.37846926509,15.));
#21222=CARTESIAN_POINT('Ctrl Pts',(24.725498909423,-36.3957374383337,15.));
#21223=CARTESIAN_POINT('Ctrl Pts',(14.911486495888,-41.396226524684,0.));
#21224=CARTESIAN_POINT('Ctrl Pts',(14.911486495888,-41.396226524684,18.));
#21225=CARTESIAN_POINT('Ctrl Pts',(14.9156446533966,-41.3758141263348,0.));
#21226=CARTESIAN_POINT('Ctrl Pts',(14.9156446533966,-41.3758141263348,18.));
#21227=CARTESIAN_POINT('Ctrl Pts',(14.9239113834707,-41.3349931861715,0.));
#21228=CARTESIAN_POINT('Ctrl Pts',(14.9239113834707,-41.3349931861715,18.));
#21229=CARTESIAN_POINT('Ctrl Pts',(14.936162723752,-41.2737733455422,0.));
#21230=CARTESIAN_POINT('Ctrl Pts',(14.936162723752,-41.2737733455422,18.));
#21231=CARTESIAN_POINT('Ctrl Pts',(14.9522002356298,-41.1921700381957,0.));
#21232=CARTESIAN_POINT('Ctrl Pts',(14.9522002356298,-41.1921700381957,18.));
#21233=CARTESIAN_POINT('Ctrl Pts',(14.9717503874227,-41.0902046498729,0.));
#21234=CARTESIAN_POINT('Ctrl Pts',(14.9717503874227,-41.0902046498729,18.));
#21235=CARTESIAN_POINT('Ctrl Pts',(14.9908026205824,-40.9882784321884,0.));
#21236=CARTESIAN_POINT('Ctrl Pts',(14.9908026205824,-40.9882784321884,18.));
#21237=CARTESIAN_POINT('Ctrl Pts',(15.0093553188655,-40.8863921801,0.));
#21238=CARTESIAN_POINT('Ctrl Pts',(15.0093553188655,-40.8863921801,18.));
#21239=CARTESIAN_POINT('Ctrl Pts',(15.0274064563211,-40.7845471608654,0.));
#21240=CARTESIAN_POINT('Ctrl Pts',(15.0274064563211,-40.7845471608654,18.));
#21241=CARTESIAN_POINT('Ctrl Pts',(15.0449536183143,-40.6827452453667,0.));
#21242=CARTESIAN_POINT('Ctrl Pts',(15.0449536183143,-40.6827452453667,18.));
#21243=CARTESIAN_POINT('Ctrl Pts',(15.0619940893017,-40.58098877043,0.));
#21244=CARTESIAN_POINT('Ctrl Pts',(15.0619940893017,-40.58098877043,18.));
#21245=CARTESIAN_POINT('Ctrl Pts',(15.0785249502524,-40.4792803645352,0.));
#21246=CARTESIAN_POINT('Ctrl Pts',(15.0785249502524,-40.4792803645352,18.));
#21247=CARTESIAN_POINT('Ctrl Pts',(15.0945431800723,-40.3776227809037,0.));
#21248=CARTESIAN_POINT('Ctrl Pts',(15.0945431800723,-40.3776227809037,18.));
#21249=CARTESIAN_POINT('Ctrl Pts',(15.1100457495259,-40.2760187401822,0.));
#21250=CARTESIAN_POINT('Ctrl Pts',(15.1100457495259,-40.2760187401822,18.));
#21251=CARTESIAN_POINT('Ctrl Pts',(15.1250297462408,-40.1744707357902,0.));
#21252=CARTESIAN_POINT('Ctrl Pts',(15.1250297462408,-40.1744707357902,18.));
#21253=CARTESIAN_POINT('Ctrl Pts',(15.1394923361537,-40.0729810652204,0.));
#21254=CARTESIAN_POINT('Ctrl Pts',(15.1394923361537,-40.0729810652204,18.));
#21255=CARTESIAN_POINT('Ctrl Pts',(15.1534306754871,-39.9715519332134,0.));
#21256=CARTESIAN_POINT('Ctrl Pts',(15.1534306754871,-39.9715519332134,18.));
#21257=CARTESIAN_POINT('Ctrl Pts',(15.1668418393198,-39.8701855339908,0.));
#21258=CARTESIAN_POINT('Ctrl Pts',(15.1668418393198,-39.8701855339908,18.));
#21259=CARTESIAN_POINT('Ctrl Pts',(15.1797227547561,-39.7688841338802,0.));
#21260=CARTESIAN_POINT('Ctrl Pts',(15.1797227547561,-39.7688841338802,18.));
#21261=CARTESIAN_POINT('Ctrl Pts',(15.1920701163803,-39.6676501731673,0.));
#21262=CARTESIAN_POINT('Ctrl Pts',(15.1920701163803,-39.6676501731673,18.));
#21263=CARTESIAN_POINT('Ctrl Pts',(15.2038804098649,-39.5664862602472,0.));
#21264=CARTESIAN_POINT('Ctrl Pts',(15.2038804098649,-39.5664862602472,18.));
#21265=CARTESIAN_POINT('Ctrl Pts',(15.2151499908149,-39.4653951093947,0.));
#21266=CARTESIAN_POINT('Ctrl Pts',(15.2151499908149,-39.4653951093947,18.));
#21267=CARTESIAN_POINT('Ctrl Pts',(15.2258751563069,-39.3643794927167,0.));
#21268=CARTESIAN_POINT('Ctrl Pts',(15.2258751563069,-39.3643794927167,18.));
#21269=CARTESIAN_POINT('Ctrl Pts',(15.2360522089072,-39.2634421927888,0.));
#21270=CARTESIAN_POINT('Ctrl Pts',(15.2360522089072,-39.2634421927888,18.));
#21271=CARTESIAN_POINT('Ctrl Pts',(15.2456775636447,-39.1625859371304,0.));
#21272=CARTESIAN_POINT('Ctrl Pts',(15.2456775636447,-39.1625859371304,18.));
#21273=CARTESIAN_POINT('Ctrl Pts',(15.2547476855825,-39.061813415425,0.));
#21274=CARTESIAN_POINT('Ctrl Pts',(15.2547476855825,-39.061813415425,18.));
#21275=CARTESIAN_POINT('Ctrl Pts',(15.2632589109473,-38.9611273555758,0.));
#21276=CARTESIAN_POINT('Ctrl Pts',(15.2632589109473,-38.9611273555758,18.));
#21277=CARTESIAN_POINT('Ctrl Pts',(15.2712072937639,-38.860530586589,0.));
#21278=CARTESIAN_POINT('Ctrl Pts',(15.2712072937639,-38.860530586589,18.));
#21279=CARTESIAN_POINT('Ctrl Pts',(15.2785884727112,-38.7600260961351,0.));
#21280=CARTESIAN_POINT('Ctrl Pts',(15.2785884727112,-38.7600260961351,18.));
#21281=CARTESIAN_POINT('Ctrl Pts',(15.2853974668211,-38.659617115053,0.));
#21282=CARTESIAN_POINT('Ctrl Pts',(15.2853974668211,-38.659617115053,18.));
#21283=CARTESIAN_POINT('Ctrl Pts',(15.2916287700102,-38.5593070891769,0.));
#21284=CARTESIAN_POINT('Ctrl Pts',(15.2916287700102,-38.5593070891769,18.));
#21285=CARTESIAN_POINT('Ctrl Pts',(15.2972767037469,-38.4590995527814,0.));
#21286=CARTESIAN_POINT('Ctrl Pts',(15.2972767037469,-38.4590995527814,18.));
#21287=CARTESIAN_POINT('Ctrl Pts',(15.3023357307483,-38.3589980188324,0.));
#21288=CARTESIAN_POINT('Ctrl Pts',(15.3023357307483,-38.3589980188324,18.));
#21289=CARTESIAN_POINT('Ctrl Pts',(15.3068007250314,-38.2590058835965,0.));
#21290=CARTESIAN_POINT('Ctrl Pts',(15.3068007250314,-38.2590058835965,18.));
#21291=CARTESIAN_POINT('Ctrl Pts',(15.310667421514,-38.1591262705847,0.));
#21292=CARTESIAN_POINT('Ctrl Pts',(15.310667421514,-38.1591262705847,18.));
#21293=CARTESIAN_POINT('Ctrl Pts',(15.3139321941687,-38.0593621055415,0.));
#21294=CARTESIAN_POINT('Ctrl Pts',(15.3139321941687,-38.0593621055415,18.));
#21295=CARTESIAN_POINT('Ctrl Pts',(15.3165911656268,-37.959716421934,0.));
#21296=CARTESIAN_POINT('Ctrl Pts',(15.3165911656268,-37.959716421934,18.));
#21297=CARTESIAN_POINT('Ctrl Pts',(15.3186394335023,-37.8601926265378,0.));
#21298=CARTESIAN_POINT('Ctrl Pts',(15.3186394335023,-37.8601926265378,18.));
#21299=CARTESIAN_POINT('Ctrl Pts',(15.320070396385,-37.7607947318286,0.));
#21300=CARTESIAN_POINT('Ctrl Pts',(15.320070396385,-37.7607947318286,18.));
#21301=CARTESIAN_POINT('Ctrl Pts',(15.320874689078,-37.6615277218027,0.));
#21302=CARTESIAN_POINT('Ctrl Pts',(15.320874689078,-37.6615277218027,18.));
#21303=CARTESIAN_POINT('Ctrl Pts',(15.3210406145546,-37.562397408596,0.));
#21304=CARTESIAN_POINT('Ctrl Pts',(15.3210406145546,-37.562397408596,18.));
#21305=CARTESIAN_POINT('Ctrl Pts',(15.3205561366169,-37.4634097578665,0.));
#21306=CARTESIAN_POINT('Ctrl Pts',(15.3205561366169,-37.4634097578665,18.));
#21307=CARTESIAN_POINT('Ctrl Pts',(15.3194106233801,-37.3645702997848,0.));
#21308=CARTESIAN_POINT('Ctrl Pts',(15.3194106233801,-37.3645702997848,18.));
#21309=CARTESIAN_POINT('Ctrl Pts',(15.3175963510697,-37.2658836214694,0.));
#21310=CARTESIAN_POINT('Ctrl Pts',(15.3175963510697,-37.2658836214694,18.));
#21311=CARTESIAN_POINT('Ctrl Pts',(15.3151109648809,-37.1673525354642,0.));
#21312=CARTESIAN_POINT('Ctrl Pts',(15.3151109648809,-37.1673525354642,18.));
#21313=CARTESIAN_POINT('Ctrl Pts',(15.3119562971444,-37.0689784837457,0.));
#21314=CARTESIAN_POINT('Ctrl Pts',(15.3119562971444,-37.0689784837457,18.));
#21315=CARTESIAN_POINT('Ctrl Pts',(15.3081335446406,-36.970763176802,0.));
#21316=CARTESIAN_POINT('Ctrl Pts',(15.3081335446406,-36.970763176802,18.));
#21317=CARTESIAN_POINT('Ctrl Pts',(15.3036390436952,-36.8727100302512,0.));
#21318=CARTESIAN_POINT('Ctrl Pts',(15.3036390436952,-36.8727100302512,18.));
#21319=CARTESIAN_POINT('Ctrl Pts',(15.2984606286737,-36.7748254044502,0.));
#21320=CARTESIAN_POINT('Ctrl Pts',(15.2984606286737,-36.7748254044502,18.));
#21321=CARTESIAN_POINT('Ctrl Pts',(15.2925717100767,-36.6771206167756,0.));
#21322=CARTESIAN_POINT('Ctrl Pts',(15.2925717100767,-36.6771206167756,18.));
#21323=CARTESIAN_POINT('Ctrl Pts',(15.2859343913094,-36.5796108931244,0.));
#21324=CARTESIAN_POINT('Ctrl Pts',(15.2859343913094,-36.5796108931244,18.));
#21325=CARTESIAN_POINT('Ctrl Pts',(15.2785104654792,-36.4823116513289,0.));
#21326=CARTESIAN_POINT('Ctrl Pts',(15.2785104654792,-36.4823116513289,18.));
#21327=CARTESIAN_POINT('Ctrl Pts',(15.2702711460936,-36.3852352131887,0.));
#21328=CARTESIAN_POINT('Ctrl Pts',(15.2702711460936,-36.3852352131887,18.));
#21329=CARTESIAN_POINT('Ctrl Pts',(15.2612053303773,-36.2883880151607,0.));
#21330=CARTESIAN_POINT('Ctrl Pts',(15.2612053303773,-36.2883880151607,18.));
#21331=CARTESIAN_POINT('Ctrl Pts',(15.2513334565427,-36.1917659216814,0.));
#21332=CARTESIAN_POINT('Ctrl Pts',(15.2513334565427,-36.1917659216814,18.));
#21333=CARTESIAN_POINT('Ctrl Pts',(15.240697754828,-36.095357546697,0.));
#21334=CARTESIAN_POINT('Ctrl Pts',(15.240697754828,-36.095357546697,18.));
#21335=CARTESIAN_POINT('Ctrl Pts',(15.2293360946131,-35.9991531408727,0.));
#21336=CARTESIAN_POINT('Ctrl Pts',(15.2293360946131,-35.9991531408727,18.));
#21337=CARTESIAN_POINT('Ctrl Pts',(15.2172585668056,-35.9031525499277,0.));
#21338=CARTESIAN_POINT('Ctrl Pts',(15.2172585668056,-35.9031525499277,18.));
#21339=CARTESIAN_POINT('Ctrl Pts',(15.2044274601769,-35.8073720252878,0.));
#21340=CARTESIAN_POINT('Ctrl Pts',(15.2044274601769,-35.8073720252878,18.));
#21341=CARTESIAN_POINT('Ctrl Pts',(15.1907243629658,-35.7118553943773,0.));
#21342=CARTESIAN_POINT('Ctrl Pts',(15.1907243629658,-35.7118553943773,18.));
#21343=CARTESIAN_POINT('Ctrl Pts',(15.1759785763051,-35.6166644736253,0.));
#21344=CARTESIAN_POINT('Ctrl Pts',(15.1759785763051,-35.6166644736253,18.));
#21345=CARTESIAN_POINT('Ctrl Pts',(15.1600260710383,-35.5218591529746,0.));
#21346=CARTESIAN_POINT('Ctrl Pts',(15.1600260710383,-35.5218591529746,18.));
#21347=CARTESIAN_POINT('Ctrl Pts',(15.1427632633831,-35.4274792115856,0.));
#21348=CARTESIAN_POINT('Ctrl Pts',(15.1427632633831,-35.4274792115856,18.));
#21349=CARTESIAN_POINT('Ctrl Pts',(15.1241934020681,-35.3335286891314,0.));
#21350=CARTESIAN_POINT('Ctrl Pts',(15.1241934020681,-35.3335286891314,18.));
#21351=CARTESIAN_POINT('Ctrl Pts',(15.104500806927,-35.2399506932815,0.));
#21352=CARTESIAN_POINT('Ctrl Pts',(15.104500806927,-35.2399506932815,18.));
#21353=CARTESIAN_POINT('Ctrl Pts',(15.08395927165,-35.1466591020976,0.));
#21354=CARTESIAN_POINT('Ctrl Pts',(15.08395927165,-35.1466591020976,18.));
#21355=CARTESIAN_POINT('Ctrl Pts',(15.0627878528202,-35.0535882932913,0.));
#21356=CARTESIAN_POINT('Ctrl Pts',(15.0627878528202,-35.0535882932913,18.));
#21357=CARTESIAN_POINT('Ctrl Pts',(15.041018569143,-34.9607388363587,0.));
#21358=CARTESIAN_POINT('Ctrl Pts',(15.041018569143,-34.9607388363587,18.));
#21359=CARTESIAN_POINT('Ctrl Pts',(15.0183713484962,-34.8682205930809,0.));
#21360=CARTESIAN_POINT('Ctrl Pts',(15.0183713484962,-34.8682205930809,18.));
#21361=CARTESIAN_POINT('Ctrl Pts',(14.9940927023321,-34.7763085406486,0.));
#21362=CARTESIAN_POINT('Ctrl Pts',(14.9940927023321,-34.7763085406486,18.));
#21363=CARTESIAN_POINT('Ctrl Pts',(14.9671565602316,-34.6853717911268,0.));
#21364=CARTESIAN_POINT('Ctrl Pts',(14.9671565602316,-34.6853717911268,18.));
#21365=CARTESIAN_POINT('Ctrl Pts',(14.9426481276593,-34.6137007885254,0.));
#21366=CARTESIAN_POINT('Ctrl Pts',(14.9426481276593,-34.6137007885254,18.));
#21367=CARTESIAN_POINT('Ctrl Pts',(14.9222326355678,-34.5606858566713,0.));
#21368=CARTESIAN_POINT('Ctrl Pts',(14.9222326355678,-34.5606858566713,18.));
#21369=CARTESIAN_POINT('Ctrl Pts',(14.9076710061311,-34.525687510388,0.));
#21370=CARTESIAN_POINT('Ctrl Pts',(14.9076710061311,-34.525687510388,18.));
#21371=CARTESIAN_POINT('Ctrl Pts',(14.9001523628048,-34.5082745737944,0.));
#21372=CARTESIAN_POINT('Ctrl Pts',(14.9001523628048,-34.5082745737944,18.));
#21373=CARTESIAN_POINT('',(14.9114864958881,-41.3962265246839,0.));
#21374=CARTESIAN_POINT('Ctrl Pts',(14.9001523628048,-34.5082745737944,0.));
#21375=CARTESIAN_POINT('Ctrl Pts',(14.9076710061311,-34.525687510388,0.));
#21376=CARTESIAN_POINT('Ctrl Pts',(14.9222326355678,-34.5606858566713,0.));
#21377=CARTESIAN_POINT('Ctrl Pts',(14.9426481276593,-34.6137007885254,0.));
#21378=CARTESIAN_POINT('Ctrl Pts',(14.9671565602316,-34.6853717911268,0.));
#21379=CARTESIAN_POINT('Ctrl Pts',(14.9940927023321,-34.7763085406486,0.));
#21380=CARTESIAN_POINT('Ctrl Pts',(15.0183713484962,-34.8682205930809,0.));
#21381=CARTESIAN_POINT('Ctrl Pts',(15.041018569143,-34.9607388363587,0.));
#21382=CARTESIAN_POINT('Ctrl Pts',(15.0627878528202,-35.0535882932913,0.));
#21383=CARTESIAN_POINT('Ctrl Pts',(15.08395927165,-35.1466591020976,0.));
#21384=CARTESIAN_POINT('Ctrl Pts',(15.104500806927,-35.2399506932815,0.));
#21385=CARTESIAN_POINT('Ctrl Pts',(15.1241934020681,-35.3335286891314,0.));
#21386=CARTESIAN_POINT('Ctrl Pts',(15.1427632633831,-35.4274792115856,0.));
#21387=CARTESIAN_POINT('Ctrl Pts',(15.1600260710383,-35.5218591529746,0.));
#21388=CARTESIAN_POINT('Ctrl Pts',(15.1759785763051,-35.6166644736253,0.));
#21389=CARTESIAN_POINT('Ctrl Pts',(15.1907243629658,-35.7118553943773,0.));
#21390=CARTESIAN_POINT('Ctrl Pts',(15.2044274601769,-35.8073720252878,0.));
#21391=CARTESIAN_POINT('Ctrl Pts',(15.2172585668056,-35.9031525499277,0.));
#21392=CARTESIAN_POINT('Ctrl Pts',(15.2293360946131,-35.9991531408727,0.));
#21393=CARTESIAN_POINT('Ctrl Pts',(15.240697754828,-36.095357546697,0.));
#21394=CARTESIAN_POINT('Ctrl Pts',(15.2513334565427,-36.1917659216814,0.));
#21395=CARTESIAN_POINT('Ctrl Pts',(15.2612053303773,-36.2883880151607,0.));
#21396=CARTESIAN_POINT('Ctrl Pts',(15.2702711460936,-36.3852352131887,0.));
#21397=CARTESIAN_POINT('Ctrl Pts',(15.2785104654792,-36.4823116513289,0.));
#21398=CARTESIAN_POINT('Ctrl Pts',(15.2859343913094,-36.5796108931244,0.));
#21399=CARTESIAN_POINT('Ctrl Pts',(15.2925717100767,-36.6771206167756,0.));
#21400=CARTESIAN_POINT('Ctrl Pts',(15.2984606286737,-36.7748254044502,0.));
#21401=CARTESIAN_POINT('Ctrl Pts',(15.3036390436952,-36.8727100302512,0.));
#21402=CARTESIAN_POINT('Ctrl Pts',(15.3081335446406,-36.970763176802,0.));
#21403=CARTESIAN_POINT('Ctrl Pts',(15.3119562971444,-37.0689784837457,0.));
#21404=CARTESIAN_POINT('Ctrl Pts',(15.3151109648809,-37.1673525354642,0.));
#21405=CARTESIAN_POINT('Ctrl Pts',(15.3175963510697,-37.2658836214694,0.));
#21406=CARTESIAN_POINT('Ctrl Pts',(15.3194106233801,-37.3645702997848,0.));
#21407=CARTESIAN_POINT('Ctrl Pts',(15.3205561366169,-37.4634097578665,0.));
#21408=CARTESIAN_POINT('Ctrl Pts',(15.3210406145546,-37.562397408596,0.));
#21409=CARTESIAN_POINT('Ctrl Pts',(15.320874689078,-37.6615277218027,0.));
#21410=CARTESIAN_POINT('Ctrl Pts',(15.320070396385,-37.7607947318286,0.));
#21411=CARTESIAN_POINT('Ctrl Pts',(15.3186394335023,-37.8601926265378,0.));
#21412=CARTESIAN_POINT('Ctrl Pts',(15.3165911656268,-37.959716421934,0.));
#21413=CARTESIAN_POINT('Ctrl Pts',(15.3139321941687,-38.0593621055415,0.));
#21414=CARTESIAN_POINT('Ctrl Pts',(15.310667421514,-38.1591262705847,0.));
#21415=CARTESIAN_POINT('Ctrl Pts',(15.3068007250314,-38.2590058835965,0.));
#21416=CARTESIAN_POINT('Ctrl Pts',(15.3023357307483,-38.3589980188324,0.));
#21417=CARTESIAN_POINT('Ctrl Pts',(15.2972767037469,-38.4590995527814,0.));
#21418=CARTESIAN_POINT('Ctrl Pts',(15.2916287700102,-38.5593070891769,0.));
#21419=CARTESIAN_POINT('Ctrl Pts',(15.2853974668211,-38.659617115053,0.));
#21420=CARTESIAN_POINT('Ctrl Pts',(15.2785884727112,-38.7600260961351,0.));
#21421=CARTESIAN_POINT('Ctrl Pts',(15.2712072937639,-38.860530586589,0.));
#21422=CARTESIAN_POINT('Ctrl Pts',(15.2632589109473,-38.9611273555758,0.));
#21423=CARTESIAN_POINT('Ctrl Pts',(15.2547476855825,-39.061813415425,0.));
#21424=CARTESIAN_POINT('Ctrl Pts',(15.2456775636447,-39.1625859371304,0.));
#21425=CARTESIAN_POINT('Ctrl Pts',(15.2360522089072,-39.2634421927888,0.));
#21426=CARTESIAN_POINT('Ctrl Pts',(15.2258751563069,-39.3643794927167,0.));
#21427=CARTESIAN_POINT('Ctrl Pts',(15.2151499908149,-39.4653951093947,0.));
#21428=CARTESIAN_POINT('Ctrl Pts',(15.2038804098649,-39.5664862602472,0.));
#21429=CARTESIAN_POINT('Ctrl Pts',(15.1920701163803,-39.6676501731673,0.));
#21430=CARTESIAN_POINT('Ctrl Pts',(15.1797227547561,-39.7688841338802,0.));
#21431=CARTESIAN_POINT('Ctrl Pts',(15.1668418393198,-39.8701855339908,0.));
#21432=CARTESIAN_POINT('Ctrl Pts',(15.1534306754871,-39.9715519332134,0.));
#21433=CARTESIAN_POINT('Ctrl Pts',(15.1394923361537,-40.0729810652204,0.));
#21434=CARTESIAN_POINT('Ctrl Pts',(15.1250297462408,-40.1744707357902,0.));
#21435=CARTESIAN_POINT('Ctrl Pts',(15.1100457495259,-40.2760187401822,0.));
#21436=CARTESIAN_POINT('Ctrl Pts',(15.0945431800723,-40.3776227809037,0.));
#21437=CARTESIAN_POINT('Ctrl Pts',(15.0785249502524,-40.4792803645352,0.));
#21438=CARTESIAN_POINT('Ctrl Pts',(15.0619940893017,-40.58098877043,0.));
#21439=CARTESIAN_POINT('Ctrl Pts',(15.0449536183143,-40.6827452453667,0.));
#21440=CARTESIAN_POINT('Ctrl Pts',(15.0274064563211,-40.7845471608654,0.));
#21441=CARTESIAN_POINT('Ctrl Pts',(15.0093553188655,-40.8863921801,0.));
#21442=CARTESIAN_POINT('Ctrl Pts',(14.9908026205824,-40.9882784321884,0.));
#21443=CARTESIAN_POINT('Ctrl Pts',(14.9679399407908,-41.1105898934098,0.));
#21444=CARTESIAN_POINT('Ctrl Pts',(14.9482653093396,-41.2125650743922,0.));
#21445=CARTESIAN_POINT('Ctrl Pts',(14.9321285285561,-41.2941761025922,0.));
#21446=CARTESIAN_POINT('Ctrl Pts',(14.919802810928,-41.3554017279611,0.));
#21447=CARTESIAN_POINT('Ctrl Pts',(14.911486495888,-41.396226524684,0.));
#21448=CARTESIAN_POINT('',(14.9114864958881,-41.3962265246839,15.));
#21449=CARTESIAN_POINT('Ctrl Pts',(14.911486495888,-41.396226524684,15.));
#21450=CARTESIAN_POINT('Ctrl Pts',(14.9156446533966,-41.3758141263348,15.));
#21451=CARTESIAN_POINT('Ctrl Pts',(14.9239113834707,-41.3349931861715,15.));
#21452=CARTESIAN_POINT('Ctrl Pts',(14.936162723752,-41.2737733455422,15.));
#21453=CARTESIAN_POINT('Ctrl Pts',(14.9522002356298,-41.1921700381957,15.));
#21454=CARTESIAN_POINT('Ctrl Pts',(14.9717503874227,-41.0902046498729,15.));
#21455=CARTESIAN_POINT('Ctrl Pts',(14.9908026205824,-40.9882784321884,15.));
#21456=CARTESIAN_POINT('Ctrl Pts',(15.0093553188655,-40.8863921801,15.));
#21457=CARTESIAN_POINT('Ctrl Pts',(15.0274064563211,-40.7845471608654,15.));
#21458=CARTESIAN_POINT('Ctrl Pts',(15.0449536183143,-40.6827452453667,15.));
#21459=CARTESIAN_POINT('Ctrl Pts',(15.0619940893017,-40.58098877043,15.));
#21460=CARTESIAN_POINT('Ctrl Pts',(15.0785249502524,-40.4792803645352,15.));
#21461=CARTESIAN_POINT('Ctrl Pts',(15.0945431800723,-40.3776227809037,15.));
#21462=CARTESIAN_POINT('Ctrl Pts',(15.1100457495259,-40.2760187401822,15.));
#21463=CARTESIAN_POINT('Ctrl Pts',(15.1250297462408,-40.1744707357902,15.));
#21464=CARTESIAN_POINT('Ctrl Pts',(15.1394923361537,-40.0729810652204,15.));
#21465=CARTESIAN_POINT('Ctrl Pts',(15.1534306754871,-39.9715519332134,15.));
#21466=CARTESIAN_POINT('Ctrl Pts',(15.1668418393198,-39.8701855339908,15.));
#21467=CARTESIAN_POINT('Ctrl Pts',(15.1797227547561,-39.7688841338802,15.));
#21468=CARTESIAN_POINT('Ctrl Pts',(15.1920701163803,-39.6676501731673,15.));
#21469=CARTESIAN_POINT('Ctrl Pts',(15.2038804098649,-39.5664862602472,15.));
#21470=CARTESIAN_POINT('Ctrl Pts',(15.2151499908149,-39.4653951093947,15.));
#21471=CARTESIAN_POINT('Ctrl Pts',(15.2258751563069,-39.3643794927167,15.));
#21472=CARTESIAN_POINT('Ctrl Pts',(15.2360522089072,-39.2634421927888,15.));
#21473=CARTESIAN_POINT('Ctrl Pts',(15.2456775636447,-39.1625859371304,15.));
#21474=CARTESIAN_POINT('Ctrl Pts',(15.2547476855825,-39.061813415425,15.));
#21475=CARTESIAN_POINT('Ctrl Pts',(15.2632589109473,-38.9611273555758,15.));
#21476=CARTESIAN_POINT('Ctrl Pts',(15.2712072937639,-38.860530586589,15.));
#21477=CARTESIAN_POINT('Ctrl Pts',(15.2785884727112,-38.7600260961351,15.));
#21478=CARTESIAN_POINT('Ctrl Pts',(15.2853974668211,-38.659617115053,15.));
#21479=CARTESIAN_POINT('Ctrl Pts',(15.2916287700102,-38.5593070891769,15.));
#21480=CARTESIAN_POINT('Ctrl Pts',(15.2972767037469,-38.4590995527814,15.));
#21481=CARTESIAN_POINT('Ctrl Pts',(15.3023357307483,-38.3589980188324,15.));
#21482=CARTESIAN_POINT('Ctrl Pts',(15.3068007250314,-38.2590058835965,15.));
#21483=CARTESIAN_POINT('Ctrl Pts',(15.310667421514,-38.1591262705847,15.));
#21484=CARTESIAN_POINT('Ctrl Pts',(15.3139321941687,-38.0593621055415,15.));
#21485=CARTESIAN_POINT('Ctrl Pts',(15.3165911656268,-37.959716421934,15.));
#21486=CARTESIAN_POINT('Ctrl Pts',(15.3186394335023,-37.8601926265378,15.));
#21487=CARTESIAN_POINT('Ctrl Pts',(15.320070396385,-37.7607947318286,15.));
#21488=CARTESIAN_POINT('Ctrl Pts',(15.320874689078,-37.6615277218027,15.));
#21489=CARTESIAN_POINT('Ctrl Pts',(15.3210406145546,-37.562397408596,15.));
#21490=CARTESIAN_POINT('Ctrl Pts',(15.3205561366169,-37.4634097578665,15.));
#21491=CARTESIAN_POINT('Ctrl Pts',(15.3194106233801,-37.3645702997848,15.));
#21492=CARTESIAN_POINT('Ctrl Pts',(15.3175963510697,-37.2658836214694,15.));
#21493=CARTESIAN_POINT('Ctrl Pts',(15.3151109648809,-37.1673525354642,15.));
#21494=CARTESIAN_POINT('Ctrl Pts',(15.3119562971444,-37.0689784837457,15.));
#21495=CARTESIAN_POINT('Ctrl Pts',(15.3081335446406,-36.970763176802,15.));
#21496=CARTESIAN_POINT('Ctrl Pts',(15.3036390436952,-36.8727100302512,15.));
#21497=CARTESIAN_POINT('Ctrl Pts',(15.2984606286737,-36.7748254044502,15.));
#21498=CARTESIAN_POINT('Ctrl Pts',(15.2925717100767,-36.6771206167756,15.));
#21499=CARTESIAN_POINT('Ctrl Pts',(15.2859343913094,-36.5796108931244,15.));
#21500=CARTESIAN_POINT('Ctrl Pts',(15.2785104654792,-36.4823116513289,15.));
#21501=CARTESIAN_POINT('Ctrl Pts',(15.2702711460936,-36.3852352131887,15.));
#21502=CARTESIAN_POINT('Ctrl Pts',(15.2612053303773,-36.2883880151607,15.));
#21503=CARTESIAN_POINT('Ctrl Pts',(15.2513334565427,-36.1917659216814,15.));
#21504=CARTESIAN_POINT('Ctrl Pts',(15.240697754828,-36.095357546697,15.));
#21505=CARTESIAN_POINT('Ctrl Pts',(15.2293360946131,-35.9991531408727,15.));
#21506=CARTESIAN_POINT('Ctrl Pts',(15.2172585668056,-35.9031525499277,15.));
#21507=CARTESIAN_POINT('Ctrl Pts',(15.2044274601769,-35.8073720252878,15.));
#21508=CARTESIAN_POINT('Ctrl Pts',(15.1907243629658,-35.7118553943773,15.));
#21509=CARTESIAN_POINT('Ctrl Pts',(15.1759785763051,-35.6166644736253,15.));
#21510=CARTESIAN_POINT('Ctrl Pts',(15.1600260710383,-35.5218591529746,15.));
#21511=CARTESIAN_POINT('Ctrl Pts',(15.1427632633831,-35.4274792115856,15.));
#21512=CARTESIAN_POINT('Ctrl Pts',(15.1241934020681,-35.3335286891314,15.));
#21513=CARTESIAN_POINT('Ctrl Pts',(15.104500806927,-35.2399506932815,15.));
#21514=CARTESIAN_POINT('Ctrl Pts',(15.08395927165,-35.1466591020976,15.));
#21515=CARTESIAN_POINT('Ctrl Pts',(15.0627878528202,-35.0535882932913,15.));
#21516=CARTESIAN_POINT('Ctrl Pts',(15.041018569143,-34.9607388363587,15.));
#21517=CARTESIAN_POINT('Ctrl Pts',(15.0183713484962,-34.8682205930809,15.));
#21518=CARTESIAN_POINT('Ctrl Pts',(14.9940927023321,-34.7763085406486,15.));
#21519=CARTESIAN_POINT('Ctrl Pts',(14.9671565602316,-34.6853717911268,15.));
#21520=CARTESIAN_POINT('Ctrl Pts',(14.9426481276593,-34.6137007885254,15.));
#21521=CARTESIAN_POINT('Ctrl Pts',(14.9222326355678,-34.5606858566713,15.));
#21522=CARTESIAN_POINT('Ctrl Pts',(14.9076710061311,-34.525687510388,15.));
#21523=CARTESIAN_POINT('Ctrl Pts',(14.9001523628048,-34.5082745737944,15.));
#21524=CARTESIAN_POINT('',(14.9114864958881,-41.3962265246839,0.));
#21525=CARTESIAN_POINT('Origin',(3.50213800024364E-12,-1.07784724682657E-11,
0.));
#21526=CARTESIAN_POINT('',(12.2684454652018,-42.2550026135057,0.));
#21527=CARTESIAN_POINT('Origin',(3.50213800024364E-12,-1.07784724682657E-11,
0.));
#21528=CARTESIAN_POINT('',(12.2684454652018,-42.2550026135057,15.));
#21529=CARTESIAN_POINT('Origin',(3.50213800024364E-12,-1.07784724682657E-11,
15.));
#21530=CARTESIAN_POINT('',(12.2684454652018,-42.2550026135057,0.));
#21531=CARTESIAN_POINT('Ctrl Pts',(8.2289783962506,-36.6758703925241,0.));
#21532=CARTESIAN_POINT('Ctrl Pts',(8.2289783962506,-36.6758703925241,18.));
#21533=CARTESIAN_POINT('Ctrl Pts',(8.23313075335376,-36.6943771018148,0.));
#21534=CARTESIAN_POINT('Ctrl Pts',(8.23313075335376,-36.6943771018148,18.));
#21535=CARTESIAN_POINT('Ctrl Pts',(8.24192165947366,-36.7312504697652,0.));
#21536=CARTESIAN_POINT('Ctrl Pts',(8.24192165947366,-36.7312504697652,18.));
#21537=CARTESIAN_POINT('Ctrl Pts',(8.2565665745182,-36.7861403757604,0.));
#21538=CARTESIAN_POINT('Ctrl Pts',(8.2565665745182,-36.7861403757604,18.));
#21539=CARTESIAN_POINT('Ctrl Pts',(8.27886599440784,-36.8585291300917,0.));
#21540=CARTESIAN_POINT('Ctrl Pts',(8.27886599440784,-36.8585291300917,18.));
#21541=CARTESIAN_POINT('Ctrl Pts',(8.3105254779459,-36.9479311729484,0.));
#21542=CARTESIAN_POINT('Ctrl Pts',(8.3105254779459,-36.9479311729484,18.));
#21543=CARTESIAN_POINT('Ctrl Pts',(8.34490818952639,-37.0365602155148,0.));
#21544=CARTESIAN_POINT('Ctrl Pts',(8.34490818952639,-37.0365602155148,18.));
#21545=CARTESIAN_POINT('Ctrl Pts',(8.38096706211447,-37.1247207489179,0.));
#21546=CARTESIAN_POINT('Ctrl Pts',(8.38096706211447,-37.1247207489179,18.));
#21547=CARTESIAN_POINT('Ctrl Pts',(8.41793088313259,-37.2126332013933,0.));
#21548=CARTESIAN_POINT('Ctrl Pts',(8.41793088313259,-37.2126332013933,18.));
#21549=CARTESIAN_POINT('Ctrl Pts',(8.45550849433959,-37.3003733151561,0.));
#21550=CARTESIAN_POINT('Ctrl Pts',(8.45550849433959,-37.3003733151561,18.));
#21551=CARTESIAN_POINT('Ctrl Pts',(8.49372546467075,-37.3879218093514,0.));
#21552=CARTESIAN_POINT('Ctrl Pts',(8.49372546467075,-37.3879218093514,18.));
#21553=CARTESIAN_POINT('Ctrl Pts',(8.53279758643783,-37.4752030152968,0.));
#21554=CARTESIAN_POINT('Ctrl Pts',(8.53279758643783,-37.4752030152968,18.));
#21555=CARTESIAN_POINT('Ctrl Pts',(8.57299698459465,-37.5621256752108,0.));
#21556=CARTESIAN_POINT('Ctrl Pts',(8.57299698459465,-37.5621256752108,18.));
#21557=CARTESIAN_POINT('Ctrl Pts',(8.61450621749154,-37.6486274754754,0.));
#21558=CARTESIAN_POINT('Ctrl Pts',(8.61450621749154,-37.6486274754754,18.));
#21559=CARTESIAN_POINT('Ctrl Pts',(8.65732553894524,-37.7347032383719,0.));
#21560=CARTESIAN_POINT('Ctrl Pts',(8.65732553894524,-37.7347032383719,18.));
#21561=CARTESIAN_POINT('Ctrl Pts',(8.70134776631143,-37.8203816669031,0.));
#21562=CARTESIAN_POINT('Ctrl Pts',(8.70134776631143,-37.8203816669031,18.));
#21563=CARTESIAN_POINT('Ctrl Pts',(8.74640499479001,-37.9057107230066,0.));
#21564=CARTESIAN_POINT('Ctrl Pts',(8.74640499479001,-37.9057107230066,18.));
#21565=CARTESIAN_POINT('Ctrl Pts',(8.79232279131091,-37.9907407304174,0.));
#21566=CARTESIAN_POINT('Ctrl Pts',(8.79232279131091,-37.9907407304174,18.));
#21567=CARTESIAN_POINT('Ctrl Pts',(8.83897959763348,-38.0755058326913,0.));
#21568=CARTESIAN_POINT('Ctrl Pts',(8.83897959763348,-38.0755058326913,18.));
#21569=CARTESIAN_POINT('Ctrl Pts',(8.88633535238434,-38.1600150482528,0.));
#21570=CARTESIAN_POINT('Ctrl Pts',(8.88633535238434,-38.1600150482528,18.));
#21571=CARTESIAN_POINT('Ctrl Pts',(8.93439830996338,-38.2442625706309,0.));
#21572=CARTESIAN_POINT('Ctrl Pts',(8.93439830996338,-38.2442625706309,18.));
#21573=CARTESIAN_POINT('Ctrl Pts',(8.98320483785759,-38.3282340281403,0.));
#21574=CARTESIAN_POINT('Ctrl Pts',(8.98320483785759,-38.3282340281403,18.));
#21575=CARTESIAN_POINT('Ctrl Pts',(9.0327957936019,-38.4119138099805,0.));
#21576=CARTESIAN_POINT('Ctrl Pts',(9.0327957936019,-38.4119138099805,18.));
#21577=CARTESIAN_POINT('Ctrl Pts',(9.08319014288085,-38.4952932486131,0.));
#21578=CARTESIAN_POINT('Ctrl Pts',(9.08319014288085,-38.4952932486131,18.));
#21579=CARTESIAN_POINT('Ctrl Pts',(9.13437512010585,-38.5783736628826,0.));
#21580=CARTESIAN_POINT('Ctrl Pts',(9.13437512010585,-38.5783736628826,18.));
#21581=CARTESIAN_POINT('Ctrl Pts',(9.18632019394329,-38.6611620045193,0.));
#21582=CARTESIAN_POINT('Ctrl Pts',(9.18632019394329,-38.6611620045193,18.));
#21583=CARTESIAN_POINT('Ctrl Pts',(9.2389853919933,-38.7436682576832,0.));
#21584=CARTESIAN_POINT('Ctrl Pts',(9.2389853919933,-38.7436682576832,18.));
#21585=CARTESIAN_POINT('Ctrl Pts',(9.29233110570902,-38.8259023794241,0.));
#21586=CARTESIAN_POINT('Ctrl Pts',(9.29233110570902,-38.8259023794241,18.));
#21587=CARTESIAN_POINT('Ctrl Pts',(9.34632917154636,-38.9078708427078,0.));
#21588=CARTESIAN_POINT('Ctrl Pts',(9.34632917154636,-38.9078708427078,18.));
#21589=CARTESIAN_POINT('Ctrl Pts',(9.40096600877643,-38.9895756526779,0.));
#21590=CARTESIAN_POINT('Ctrl Pts',(9.40096600877643,-38.9895756526779,18.));
#21591=CARTESIAN_POINT('Ctrl Pts',(9.45623664577431,-39.0710161994951,0.));
#21592=CARTESIAN_POINT('Ctrl Pts',(9.45623664577431,-39.0710161994951,18.));
#21593=CARTESIAN_POINT('Ctrl Pts',(9.5121410453562,-39.1521903958955,0.));
#21594=CARTESIAN_POINT('Ctrl Pts',(9.5121410453562,-39.1521903958955,18.));
#21595=CARTESIAN_POINT('Ctrl Pts',(9.56867984233622,-39.2330959982788,0.));
#21596=CARTESIAN_POINT('Ctrl Pts',(9.56867984233622,-39.2330959982788,18.));
#21597=CARTESIAN_POINT('Ctrl Pts',(9.62584947846542,-39.3137321153686,0.));
#21598=CARTESIAN_POINT('Ctrl Pts',(9.62584947846542,-39.3137321153686,18.));
#21599=CARTESIAN_POINT('Ctrl Pts',(9.68364100883825,-39.3940995760289,0.));
#21600=CARTESIAN_POINT('Ctrl Pts',(9.68364100883825,-39.3940995760289,18.));
#21601=CARTESIAN_POINT('Ctrl Pts',(9.74204258152662,-39.4742001555227,0.));
#21602=CARTESIAN_POINT('Ctrl Pts',(9.74204258152662,-39.4742001555227,18.));
#21603=CARTESIAN_POINT('Ctrl Pts',(9.80104095251613,-39.5540361022309,0.));
#21604=CARTESIAN_POINT('Ctrl Pts',(9.80104095251613,-39.5540361022309,18.));
#21605=CARTESIAN_POINT('Ctrl Pts',(9.86062324242559,-39.6336095893767,0.));
#21606=CARTESIAN_POINT('Ctrl Pts',(9.86062324242559,-39.6336095893767,18.));
#21607=CARTESIAN_POINT('Ctrl Pts',(9.92077894513191,-39.712922089547,0.));
#21608=CARTESIAN_POINT('Ctrl Pts',(9.92077894513191,-39.712922089547,18.));
#21609=CARTESIAN_POINT('Ctrl Pts',(9.98150036150822,-39.7919742367922,0.));
#21610=CARTESIAN_POINT('Ctrl Pts',(9.98150036150822,-39.7919742367922,18.));
#21611=CARTESIAN_POINT('Ctrl Pts',(10.0427815229883,-39.8707661565233,0.));
#21612=CARTESIAN_POINT('Ctrl Pts',(10.0427815229883,-39.8707661565233,18.));
#21613=CARTESIAN_POINT('Ctrl Pts',(10.1046175096878,-39.9492976736738,0.));
#21614=CARTESIAN_POINT('Ctrl Pts',(10.1046175096878,-39.9492976736738,18.));
#21615=CARTESIAN_POINT('Ctrl Pts',(10.1670036683795,-40.0275685525923,0.));
#21616=CARTESIAN_POINT('Ctrl Pts',(10.1670036683795,-40.0275685525923,18.));
#21617=CARTESIAN_POINT('Ctrl Pts',(10.2299347125857,-40.1055787732578,0.));
#21618=CARTESIAN_POINT('Ctrl Pts',(10.2299347125857,-40.1055787732578,18.));
#21619=CARTESIAN_POINT('Ctrl Pts',(10.2934044990237,-40.1833286010098,0.));
#21620=CARTESIAN_POINT('Ctrl Pts',(10.2934044990237,-40.1833286010098,18.));
#21621=CARTESIAN_POINT('Ctrl Pts',(10.3574064830678,-40.2608184485326,0.));
#21622=CARTESIAN_POINT('Ctrl Pts',(10.3574064830678,-40.2608184485326,18.));
#21623=CARTESIAN_POINT('Ctrl Pts',(10.421933993295,-40.3380487942952,0.));
#21624=CARTESIAN_POINT('Ctrl Pts',(10.421933993295,-40.3380487942952,18.));
#21625=CARTESIAN_POINT('Ctrl Pts',(10.48698054978,-40.4150200869536,0.));
#21626=CARTESIAN_POINT('Ctrl Pts',(10.48698054978,-40.4150200869536,18.));
#21627=CARTESIAN_POINT('Ctrl Pts',(10.552540223795,-40.4917326404439,0.));
#21628=CARTESIAN_POINT('Ctrl Pts',(10.552540223795,-40.4917326404439,18.));
#21629=CARTESIAN_POINT('Ctrl Pts',(10.618607730849,-40.5681866012103,0.));
#21630=CARTESIAN_POINT('Ctrl Pts',(10.618607730849,-40.5681866012103,18.));
#21631=CARTESIAN_POINT('Ctrl Pts',(10.6851782157325,-40.6443819999244,0.));
#21632=CARTESIAN_POINT('Ctrl Pts',(10.6851782157325,-40.6443819999244,18.));
#21633=CARTESIAN_POINT('Ctrl Pts',(10.7522471109694,-40.7203187831783,0.));
#21634=CARTESIAN_POINT('Ctrl Pts',(10.7522471109694,-40.7203187831783,18.));
#21635=CARTESIAN_POINT('Ctrl Pts',(10.8198099757795,-40.7959968527561,0.));
#21636=CARTESIAN_POINT('Ctrl Pts',(10.8198099757795,-40.7959968527561,18.));
#21637=CARTESIAN_POINT('Ctrl Pts',(10.8878623066646,-40.8714161092412,0.));
#21638=CARTESIAN_POINT('Ctrl Pts',(10.8878623066646,-40.8714161092412,18.));
#21639=CARTESIAN_POINT('Ctrl Pts',(10.956399476781,-40.9465764747798,0.));
#21640=CARTESIAN_POINT('Ctrl Pts',(10.956399476781,-40.9465764747798,18.));
#21641=CARTESIAN_POINT('Ctrl Pts',(11.0254168609972,-41.0214778832142,0.));
#21642=CARTESIAN_POINT('Ctrl Pts',(11.0254168609972,-41.0214778832142,18.));
#21643=CARTESIAN_POINT('Ctrl Pts',(11.0949099155251,-41.0961202807715,0.));
#21644=CARTESIAN_POINT('Ctrl Pts',(11.0949099155251,-41.0961202807715,18.));
#21645=CARTESIAN_POINT('Ctrl Pts',(11.1648742640378,-41.1705036228854,0.));
#21646=CARTESIAN_POINT('Ctrl Pts',(11.1648742640378,-41.1705036228854,18.));
#21647=CARTESIAN_POINT('Ctrl Pts',(11.2353057980338,-41.2446278781981,0.));
#21648=CARTESIAN_POINT('Ctrl Pts',(11.2353057980338,-41.2446278781981,18.));
#21649=CARTESIAN_POINT('Ctrl Pts',(11.3062006993745,-41.3184930194148,0.));
#21650=CARTESIAN_POINT('Ctrl Pts',(11.3062006993745,-41.3184930194148,18.));
#21651=CARTESIAN_POINT('Ctrl Pts',(11.3775553120176,-41.3920989905986,0.));
#21652=CARTESIAN_POINT('Ctrl Pts',(11.3775553120176,-41.3920989905986,18.));
#21653=CARTESIAN_POINT('Ctrl Pts',(11.4493660393849,-41.4654456796071,0.));
#21654=CARTESIAN_POINT('Ctrl Pts',(11.4493660393849,-41.4654456796071,18.));
#21655=CARTESIAN_POINT('Ctrl Pts',(11.5216292382388,-41.5385328935506,0.));
#21656=CARTESIAN_POINT('Ctrl Pts',(11.5216292382388,-41.5385328935506,18.));
#21657=CARTESIAN_POINT('Ctrl Pts',(11.5943410868252,-41.6113603270596,0.));
#21658=CARTESIAN_POINT('Ctrl Pts',(11.5943410868252,-41.6113603270596,18.));
#21659=CARTESIAN_POINT('Ctrl Pts',(11.6674975352851,-41.6839275596248,0.));
#21660=CARTESIAN_POINT('Ctrl Pts',(11.6674975352851,-41.6839275596248,18.));
#21661=CARTESIAN_POINT('Ctrl Pts',(11.7410945211992,-41.7562341395977,0.));
#21662=CARTESIAN_POINT('Ctrl Pts',(11.7410945211992,-41.7562341395977,18.));
#21663=CARTESIAN_POINT('Ctrl Pts',(11.81512813804,-41.8282796562569,0.));
#21664=CARTESIAN_POINT('Ctrl Pts',(11.81512813804,-41.8282796562569,18.));
#21665=CARTESIAN_POINT('Ctrl Pts',(11.8895948153349,-41.9000638152266,0.));
#21666=CARTESIAN_POINT('Ctrl Pts',(11.8895948153349,-41.9000638152266,18.));
#21667=CARTESIAN_POINT('Ctrl Pts',(11.9644914999263,-41.9715865222182,0.));
#21668=CARTESIAN_POINT('Ctrl Pts',(11.9644914999263,-41.9715865222182,18.));
#21669=CARTESIAN_POINT('Ctrl Pts',(12.0398158079102,-42.0428479428228,0.));
#21670=CARTESIAN_POINT('Ctrl Pts',(12.0398158079102,-42.0428479428228,18.));
#21671=CARTESIAN_POINT('Ctrl Pts',(12.1155659644537,-42.1138483839101,0.));
#21672=CARTESIAN_POINT('Ctrl Pts',(12.1155659644537,-42.1138483839101,18.));
#21673=CARTESIAN_POINT('Ctrl Pts',(12.1765058047069,-42.1704402333854,0.));
#21674=CARTESIAN_POINT('Ctrl Pts',(12.1765058047069,-42.1704402333854,18.));
#21675=CARTESIAN_POINT('Ctrl Pts',(12.2224014666679,-42.2127669677092,0.));
#21676=CARTESIAN_POINT('Ctrl Pts',(12.2224014666679,-42.2127669677092,18.));
#21677=CARTESIAN_POINT('Ctrl Pts',(12.2530833383985,-42.2409327400055,0.));
#21678=CARTESIAN_POINT('Ctrl Pts',(12.2530833383985,-42.2409327400055,18.));
#21679=CARTESIAN_POINT('Ctrl Pts',(12.2684454652018,-42.2550026135057,0.));
#21680=CARTESIAN_POINT('Ctrl Pts',(12.2684454652018,-42.2550026135057,18.));
#21681=CARTESIAN_POINT('Ctrl Pts',(8.2289783962506,-36.6758703925241,0.));
#21682=CARTESIAN_POINT('Ctrl Pts',(8.23313075335376,-36.6943771018148,0.));
#21683=CARTESIAN_POINT('Ctrl Pts',(8.24192165947366,-36.7312504697652,0.));
#21684=CARTESIAN_POINT('Ctrl Pts',(8.2565665745182,-36.7861403757604,0.));
#21685=CARTESIAN_POINT('Ctrl Pts',(8.27886599440784,-36.8585291300917,0.));
#21686=CARTESIAN_POINT('Ctrl Pts',(8.3105254779459,-36.9479311729484,0.));
#21687=CARTESIAN_POINT('Ctrl Pts',(8.34490818952639,-37.0365602155148,0.));
#21688=CARTESIAN_POINT('Ctrl Pts',(8.38096706211447,-37.1247207489179,0.));
#21689=CARTESIAN_POINT('Ctrl Pts',(8.41793088313259,-37.2126332013933,0.));
#21690=CARTESIAN_POINT('Ctrl Pts',(8.45550849433959,-37.3003733151561,0.));
#21691=CARTESIAN_POINT('Ctrl Pts',(8.49372546467075,-37.3879218093514,0.));
#21692=CARTESIAN_POINT('Ctrl Pts',(8.53279758643783,-37.4752030152968,0.));
#21693=CARTESIAN_POINT('Ctrl Pts',(8.57299698459465,-37.5621256752108,0.));
#21694=CARTESIAN_POINT('Ctrl Pts',(8.61450621749154,-37.6486274754754,0.));
#21695=CARTESIAN_POINT('Ctrl Pts',(8.65732553894524,-37.7347032383719,0.));
#21696=CARTESIAN_POINT('Ctrl Pts',(8.70134776631143,-37.8203816669031,0.));
#21697=CARTESIAN_POINT('Ctrl Pts',(8.74640499479001,-37.9057107230066,0.));
#21698=CARTESIAN_POINT('Ctrl Pts',(8.79232279131091,-37.9907407304174,0.));
#21699=CARTESIAN_POINT('Ctrl Pts',(8.83897959763348,-38.0755058326913,0.));
#21700=CARTESIAN_POINT('Ctrl Pts',(8.88633535238434,-38.1600150482528,0.));
#21701=CARTESIAN_POINT('Ctrl Pts',(8.93439830996338,-38.2442625706309,0.));
#21702=CARTESIAN_POINT('Ctrl Pts',(8.98320483785759,-38.3282340281403,0.));
#21703=CARTESIAN_POINT('Ctrl Pts',(9.0327957936019,-38.4119138099805,0.));
#21704=CARTESIAN_POINT('Ctrl Pts',(9.08319014288085,-38.4952932486131,0.));
#21705=CARTESIAN_POINT('Ctrl Pts',(9.13437512010585,-38.5783736628826,0.));
#21706=CARTESIAN_POINT('Ctrl Pts',(9.18632019394329,-38.6611620045193,0.));
#21707=CARTESIAN_POINT('Ctrl Pts',(9.2389853919933,-38.7436682576832,0.));
#21708=CARTESIAN_POINT('Ctrl Pts',(9.29233110570902,-38.8259023794241,0.));
#21709=CARTESIAN_POINT('Ctrl Pts',(9.34632917154636,-38.9078708427078,0.));
#21710=CARTESIAN_POINT('Ctrl Pts',(9.40096600877643,-38.9895756526779,0.));
#21711=CARTESIAN_POINT('Ctrl Pts',(9.45623664577431,-39.0710161994951,0.));
#21712=CARTESIAN_POINT('Ctrl Pts',(9.5121410453562,-39.1521903958955,0.));
#21713=CARTESIAN_POINT('Ctrl Pts',(9.56867984233622,-39.2330959982788,0.));
#21714=CARTESIAN_POINT('Ctrl Pts',(9.62584947846542,-39.3137321153686,0.));
#21715=CARTESIAN_POINT('Ctrl Pts',(9.68364100883825,-39.3940995760289,0.));
#21716=CARTESIAN_POINT('Ctrl Pts',(9.74204258152662,-39.4742001555227,0.));
#21717=CARTESIAN_POINT('Ctrl Pts',(9.80104095251613,-39.5540361022309,0.));
#21718=CARTESIAN_POINT('Ctrl Pts',(9.86062324242559,-39.6336095893767,0.));
#21719=CARTESIAN_POINT('Ctrl Pts',(9.92077894513191,-39.712922089547,0.));
#21720=CARTESIAN_POINT('Ctrl Pts',(9.98150036150822,-39.7919742367922,0.));
#21721=CARTESIAN_POINT('Ctrl Pts',(10.0427815229883,-39.8707661565233,0.));
#21722=CARTESIAN_POINT('Ctrl Pts',(10.1046175096878,-39.9492976736738,0.));
#21723=CARTESIAN_POINT('Ctrl Pts',(10.1670036683795,-40.0275685525923,0.));
#21724=CARTESIAN_POINT('Ctrl Pts',(10.2299347125857,-40.1055787732578,0.));
#21725=CARTESIAN_POINT('Ctrl Pts',(10.2934044990237,-40.1833286010098,0.));
#21726=CARTESIAN_POINT('Ctrl Pts',(10.3574064830678,-40.2608184485326,0.));
#21727=CARTESIAN_POINT('Ctrl Pts',(10.421933993295,-40.3380487942952,0.));
#21728=CARTESIAN_POINT('Ctrl Pts',(10.48698054978,-40.4150200869536,0.));
#21729=CARTESIAN_POINT('Ctrl Pts',(10.552540223795,-40.4917326404439,0.));
#21730=CARTESIAN_POINT('Ctrl Pts',(10.618607730849,-40.5681866012103,0.));
#21731=CARTESIAN_POINT('Ctrl Pts',(10.6851782157325,-40.6443819999244,0.));
#21732=CARTESIAN_POINT('Ctrl Pts',(10.7522471109694,-40.7203187831783,0.));
#21733=CARTESIAN_POINT('Ctrl Pts',(10.8198099757795,-40.7959968527561,0.));
#21734=CARTESIAN_POINT('Ctrl Pts',(10.8878623066646,-40.8714161092412,0.));
#21735=CARTESIAN_POINT('Ctrl Pts',(10.956399476781,-40.9465764747798,0.));
#21736=CARTESIAN_POINT('Ctrl Pts',(11.0254168609972,-41.0214778832142,0.));
#21737=CARTESIAN_POINT('Ctrl Pts',(11.0949099155251,-41.0961202807715,0.));
#21738=CARTESIAN_POINT('Ctrl Pts',(11.1648742640378,-41.1705036228854,0.));
#21739=CARTESIAN_POINT('Ctrl Pts',(11.2353057980338,-41.2446278781981,0.));
#21740=CARTESIAN_POINT('Ctrl Pts',(11.3062006993745,-41.3184930194148,0.));
#21741=CARTESIAN_POINT('Ctrl Pts',(11.3775553120176,-41.3920989905986,0.));
#21742=CARTESIAN_POINT('Ctrl Pts',(11.4493660393849,-41.4654456796071,0.));
#21743=CARTESIAN_POINT('Ctrl Pts',(11.5216292382388,-41.5385328935506,0.));
#21744=CARTESIAN_POINT('Ctrl Pts',(11.5943410868252,-41.6113603270596,0.));
#21745=CARTESIAN_POINT('Ctrl Pts',(11.6674975352851,-41.6839275596248,0.));
#21746=CARTESIAN_POINT('Ctrl Pts',(11.7410945211992,-41.7562341395977,0.));
#21747=CARTESIAN_POINT('Ctrl Pts',(11.81512813804,-41.8282796562569,0.));
#21748=CARTESIAN_POINT('Ctrl Pts',(11.8895948153349,-41.9000638152266,0.));
#21749=CARTESIAN_POINT('Ctrl Pts',(11.9644914999263,-41.9715865222182,0.));
#21750=CARTESIAN_POINT('Ctrl Pts',(12.054880669507,-42.0571002269437,0.));
#21751=CARTESIAN_POINT('Ctrl Pts',(12.1307372881904,-42.1280354231517,0.));
#21752=CARTESIAN_POINT('Ctrl Pts',(12.1917619768791,-42.18457517013,0.));
#21753=CARTESIAN_POINT('Ctrl Pts',(12.2377212115623,-42.2268628664988,0.));
#21754=CARTESIAN_POINT('Ctrl Pts',(12.2684454652018,-42.2550026135057,0.));
#21755=CARTESIAN_POINT('Ctrl Pts',(8.2289783962506,-36.6758703925241,15.));
#21756=CARTESIAN_POINT('Ctrl Pts',(8.23313075335376,-36.6943771018148,15.));
#21757=CARTESIAN_POINT('Ctrl Pts',(8.24192165947366,-36.7312504697652,15.));
#21758=CARTESIAN_POINT('Ctrl Pts',(8.2565665745182,-36.7861403757604,15.));
#21759=CARTESIAN_POINT('Ctrl Pts',(8.27886599440784,-36.8585291300917,15.));
#21760=CARTESIAN_POINT('Ctrl Pts',(8.3105254779459,-36.9479311729484,15.));
#21761=CARTESIAN_POINT('Ctrl Pts',(8.34490818952639,-37.0365602155148,15.));
#21762=CARTESIAN_POINT('Ctrl Pts',(8.38096706211447,-37.1247207489179,15.));
#21763=CARTESIAN_POINT('Ctrl Pts',(8.41793088313259,-37.2126332013933,15.));
#21764=CARTESIAN_POINT('Ctrl Pts',(8.45550849433959,-37.3003733151561,15.));
#21765=CARTESIAN_POINT('Ctrl Pts',(8.49372546467075,-37.3879218093514,15.));
#21766=CARTESIAN_POINT('Ctrl Pts',(8.53279758643783,-37.4752030152968,15.));
#21767=CARTESIAN_POINT('Ctrl Pts',(8.57299698459465,-37.5621256752108,15.));
#21768=CARTESIAN_POINT('Ctrl Pts',(8.61450621749154,-37.6486274754754,15.));
#21769=CARTESIAN_POINT('Ctrl Pts',(8.65732553894524,-37.7347032383719,15.));
#21770=CARTESIAN_POINT('Ctrl Pts',(8.70134776631143,-37.8203816669031,15.));
#21771=CARTESIAN_POINT('Ctrl Pts',(8.74640499479001,-37.9057107230066,15.));
#21772=CARTESIAN_POINT('Ctrl Pts',(8.79232279131091,-37.9907407304174,15.));
#21773=CARTESIAN_POINT('Ctrl Pts',(8.83897959763348,-38.0755058326913,15.));
#21774=CARTESIAN_POINT('Ctrl Pts',(8.88633535238434,-38.1600150482528,15.));
#21775=CARTESIAN_POINT('Ctrl Pts',(8.93439830996338,-38.2442625706309,15.));
#21776=CARTESIAN_POINT('Ctrl Pts',(8.98320483785759,-38.3282340281403,15.));
#21777=CARTESIAN_POINT('Ctrl Pts',(9.0327957936019,-38.4119138099805,15.));
#21778=CARTESIAN_POINT('Ctrl Pts',(9.08319014288085,-38.4952932486131,15.));
#21779=CARTESIAN_POINT('Ctrl Pts',(9.13437512010585,-38.5783736628826,15.));
#21780=CARTESIAN_POINT('Ctrl Pts',(9.18632019394329,-38.6611620045193,15.));
#21781=CARTESIAN_POINT('Ctrl Pts',(9.2389853919933,-38.7436682576832,15.));
#21782=CARTESIAN_POINT('Ctrl Pts',(9.29233110570902,-38.8259023794241,15.));
#21783=CARTESIAN_POINT('Ctrl Pts',(9.34632917154636,-38.9078708427078,15.));
#21784=CARTESIAN_POINT('Ctrl Pts',(9.40096600877643,-38.9895756526779,15.));
#21785=CARTESIAN_POINT('Ctrl Pts',(9.45623664577431,-39.0710161994951,15.));
#21786=CARTESIAN_POINT('Ctrl Pts',(9.5121410453562,-39.1521903958955,15.));
#21787=CARTESIAN_POINT('Ctrl Pts',(9.56867984233622,-39.2330959982788,15.));
#21788=CARTESIAN_POINT('Ctrl Pts',(9.62584947846542,-39.3137321153686,15.));
#21789=CARTESIAN_POINT('Ctrl Pts',(9.68364100883825,-39.3940995760289,15.));
#21790=CARTESIAN_POINT('Ctrl Pts',(9.74204258152662,-39.4742001555227,15.));
#21791=CARTESIAN_POINT('Ctrl Pts',(9.80104095251613,-39.5540361022309,15.));
#21792=CARTESIAN_POINT('Ctrl Pts',(9.86062324242559,-39.6336095893767,15.));
#21793=CARTESIAN_POINT('Ctrl Pts',(9.92077894513191,-39.712922089547,15.));
#21794=CARTESIAN_POINT('Ctrl Pts',(9.98150036150822,-39.7919742367922,15.));
#21795=CARTESIAN_POINT('Ctrl Pts',(10.0427815229883,-39.8707661565233,15.));
#21796=CARTESIAN_POINT('Ctrl Pts',(10.1046175096878,-39.9492976736738,15.));
#21797=CARTESIAN_POINT('Ctrl Pts',(10.1670036683795,-40.0275685525923,15.));
#21798=CARTESIAN_POINT('Ctrl Pts',(10.2299347125857,-40.1055787732578,15.));
#21799=CARTESIAN_POINT('Ctrl Pts',(10.2934044990237,-40.1833286010098,15.));
#21800=CARTESIAN_POINT('Ctrl Pts',(10.3574064830678,-40.2608184485326,15.));
#21801=CARTESIAN_POINT('Ctrl Pts',(10.421933993295,-40.3380487942952,15.));
#21802=CARTESIAN_POINT('Ctrl Pts',(10.48698054978,-40.4150200869536,15.));
#21803=CARTESIAN_POINT('Ctrl Pts',(10.552540223795,-40.4917326404439,15.));
#21804=CARTESIAN_POINT('Ctrl Pts',(10.618607730849,-40.5681866012103,15.));
#21805=CARTESIAN_POINT('Ctrl Pts',(10.6851782157325,-40.6443819999244,15.));
#21806=CARTESIAN_POINT('Ctrl Pts',(10.7522471109694,-40.7203187831783,15.));
#21807=CARTESIAN_POINT('Ctrl Pts',(10.8198099757795,-40.7959968527561,15.));
#21808=CARTESIAN_POINT('Ctrl Pts',(10.8878623066646,-40.8714161092412,15.));
#21809=CARTESIAN_POINT('Ctrl Pts',(10.956399476781,-40.9465764747798,15.));
#21810=CARTESIAN_POINT('Ctrl Pts',(11.0254168609972,-41.0214778832142,15.));
#21811=CARTESIAN_POINT('Ctrl Pts',(11.0949099155251,-41.0961202807715,15.));
#21812=CARTESIAN_POINT('Ctrl Pts',(11.1648742640378,-41.1705036228854,15.));
#21813=CARTESIAN_POINT('Ctrl Pts',(11.2353057980338,-41.2446278781981,15.));
#21814=CARTESIAN_POINT('Ctrl Pts',(11.3062006993745,-41.3184930194148,15.));
#21815=CARTESIAN_POINT('Ctrl Pts',(11.3775553120176,-41.3920989905986,15.));
#21816=CARTESIAN_POINT('Ctrl Pts',(11.4493660393849,-41.4654456796071,15.));
#21817=CARTESIAN_POINT('Ctrl Pts',(11.5216292382388,-41.5385328935506,15.));
#21818=CARTESIAN_POINT('Ctrl Pts',(11.5943410868252,-41.6113603270596,15.));
#21819=CARTESIAN_POINT('Ctrl Pts',(11.6674975352851,-41.6839275596248,15.));
#21820=CARTESIAN_POINT('Ctrl Pts',(11.7410945211992,-41.7562341395977,15.));
#21821=CARTESIAN_POINT('Ctrl Pts',(11.81512813804,-41.8282796562569,15.));
#21822=CARTESIAN_POINT('Ctrl Pts',(11.8895948153349,-41.9000638152266,15.));
#21823=CARTESIAN_POINT('Ctrl Pts',(11.9644914999263,-41.9715865222182,15.));
#21824=CARTESIAN_POINT('Ctrl Pts',(12.054880669507,-42.0571002269437,15.));
#21825=CARTESIAN_POINT('Ctrl Pts',(12.1307372881904,-42.1280354231517,15.));
#21826=CARTESIAN_POINT('Ctrl Pts',(12.1917619768791,-42.18457517013,15.));
#21827=CARTESIAN_POINT('Ctrl Pts',(12.2377212115623,-42.2268628664988,15.));
#21828=CARTESIAN_POINT('Ctrl Pts',(12.2684454652018,-42.2550026135057,15.));
#21829=CARTESIAN_POINT('Ctrl Pts',(1.38952890043915,-43.9780537249529,0.));
#21830=CARTESIAN_POINT('Ctrl Pts',(1.38952890043915,-43.9780537249529,18.));
#21831=CARTESIAN_POINT('Ctrl Pts',(1.3997913212193,-43.9599253218252,0.));
#21832=CARTESIAN_POINT('Ctrl Pts',(1.3997913212193,-43.9599253218252,18.));
#21833=CARTESIAN_POINT('Ctrl Pts',(1.42026781296156,-43.9236568607623,0.));
#21834=CARTESIAN_POINT('Ctrl Pts',(1.42026781296156,-43.9236568607623,18.));
#21835=CARTESIAN_POINT('Ctrl Pts',(1.45083750111681,-43.8692192047561,0.));
#21836=CARTESIAN_POINT('Ctrl Pts',(1.45083750111681,-43.8692192047561,18.));
#21837=CARTESIAN_POINT('Ctrl Pts',(1.49130689006066,-43.7965657112708,0.));
#21838=CARTESIAN_POINT('Ctrl Pts',(1.49130689006066,-43.7965657112708,18.));
#21839=CARTESIAN_POINT('Ctrl Pts',(1.54140922714764,-43.7056321934163,0.));
#21840=CARTESIAN_POINT('Ctrl Pts',(1.54140922714764,-43.7056321934163,18.));
#21841=CARTESIAN_POINT('Ctrl Pts',(1.59102591108103,-43.6145820637333,0.));
#21842=CARTESIAN_POINT('Ctrl Pts',(1.59102591108103,-43.6145820637333,18.));
#21843=CARTESIAN_POINT('Ctrl Pts',(1.64015515906647,-43.5234155788248,0.));
#21844=CARTESIAN_POINT('Ctrl Pts',(1.64015515906647,-43.5234155788248,18.));
#21845=CARTESIAN_POINT('Ctrl Pts',(1.68879465270607,-43.4321333178711,0.));
#21846=CARTESIAN_POINT('Ctrl Pts',(1.68879465270607,-43.4321333178711,18.));
#21847=CARTESIAN_POINT('Ctrl Pts',(1.73694151741123,-43.3407363140236,0.));
#21848=CARTESIAN_POINT('Ctrl Pts',(1.73694151741123,-43.3407363140236,18.));
#21849=CARTESIAN_POINT('Ctrl Pts',(1.78459244842769,-43.2492259505872,0.));
#21850=CARTESIAN_POINT('Ctrl Pts',(1.78459244842769,-43.2492259505872,18.));
#21851=CARTESIAN_POINT('Ctrl Pts',(1.83174385734711,-43.1576038253643,0.));
#21852=CARTESIAN_POINT('Ctrl Pts',(1.83174385734711,-43.1576038253643,18.));
#21853=CARTESIAN_POINT('Ctrl Pts',(1.87839202014608,-43.065871623255,0.));
#21854=CARTESIAN_POINT('Ctrl Pts',(1.87839202014608,-43.065871623255,18.));
#21855=CARTESIAN_POINT('Ctrl Pts',(1.92453321512435,-42.9740309956624,0.));
#21856=CARTESIAN_POINT('Ctrl Pts',(1.92453321512435,-42.9740309956624,18.));
#21857=CARTESIAN_POINT('Ctrl Pts',(1.97016390194215,-42.8820834139973,0.));
#21858=CARTESIAN_POINT('Ctrl Pts',(1.97016390194215,-42.8820834139973,18.));
#21859=CARTESIAN_POINT('Ctrl Pts',(2.01528067528089,-42.7900301875309,0.));
#21860=CARTESIAN_POINT('Ctrl Pts',(2.01528067528089,-42.7900301875309,18.));
#21861=CARTESIAN_POINT('Ctrl Pts',(2.05988014924518,-42.6978725343209,0.));
#21862=CARTESIAN_POINT('Ctrl Pts',(2.05988014924518,-42.6978725343209,18.));
#21863=CARTESIAN_POINT('Ctrl Pts',(2.1039588640177,-42.6056116373455,0.));
#21864=CARTESIAN_POINT('Ctrl Pts',(2.1039588640177,-42.6056116373455,18.));
#21865=CARTESIAN_POINT('Ctrl Pts',(2.14751319676745,-42.5132487024335,0.));
#21866=CARTESIAN_POINT('Ctrl Pts',(2.14751319676745,-42.5132487024335,18.));
#21867=CARTESIAN_POINT('Ctrl Pts',(2.19053924976737,-42.4207850290047,0.));
#21868=CARTESIAN_POINT('Ctrl Pts',(2.19053924976737,-42.4207850290047,18.));
#21869=CARTESIAN_POINT('Ctrl Pts',(2.23303287465499,-42.3282220118033,0.));
#21870=CARTESIAN_POINT('Ctrl Pts',(2.23303287465499,-42.3282220118033,18.));
#21871=CARTESIAN_POINT('Ctrl Pts',(2.27498976664773,-42.2355611060784,0.));
#21872=CARTESIAN_POINT('Ctrl Pts',(2.27498976664773,-42.2355611060784,18.));
#21873=CARTESIAN_POINT('Ctrl Pts',(2.31640554742808,-42.1428038039937,0.));
#21874=CARTESIAN_POINT('Ctrl Pts',(2.31640554742808,-42.1428038039937,18.));
#21875=CARTESIAN_POINT('Ctrl Pts',(2.35727584066428,-42.0499516093661,0.));
#21876=CARTESIAN_POINT('Ctrl Pts',(2.35727584066428,-42.0499516093661,18.));
#21877=CARTESIAN_POINT('Ctrl Pts',(2.39759639399648,-41.9570060084039,0.));
#21878=CARTESIAN_POINT('Ctrl Pts',(2.39759639399648,-41.9570060084039,18.));
#21879=CARTESIAN_POINT('Ctrl Pts',(2.437363014342,-41.8639684667923,0.));
#21880=CARTESIAN_POINT('Ctrl Pts',(2.437363014342,-41.8639684667923,18.));
#21881=CARTESIAN_POINT('Ctrl Pts',(2.47657137427692,-41.7708404467533,0.));
#21882=CARTESIAN_POINT('Ctrl Pts',(2.47657137427692,-41.7708404467533,18.));
#21883=CARTESIAN_POINT('Ctrl Pts',(2.51521684674476,-41.6776234194583,0.));
#21884=CARTESIAN_POINT('Ctrl Pts',(2.51521684674476,-41.6776234194583,18.));
#21885=CARTESIAN_POINT('Ctrl Pts',(2.55329436064183,-41.5843188786284,0.));
#21886=CARTESIAN_POINT('Ctrl Pts',(2.55329436064183,-41.5843188786284,18.));
#21887=CARTESIAN_POINT('Ctrl Pts',(2.59079818040171,-41.4909283577703,0.));
#21888=CARTESIAN_POINT('Ctrl Pts',(2.59079818040171,-41.4909283577703,18.));
#21889=CARTESIAN_POINT('Ctrl Pts',(2.62772200460655,-41.3974534325936,0.));
#21890=CARTESIAN_POINT('Ctrl Pts',(2.62772200460655,-41.3974534325936,18.));
#21891=CARTESIAN_POINT('Ctrl Pts',(2.66405934050117,-41.3038957096306,0.));
#21892=CARTESIAN_POINT('Ctrl Pts',(2.66405934050117,-41.3038957096306,18.));
#21893=CARTESIAN_POINT('Ctrl Pts',(2.69980383625015,-41.2102568187956,0.));
#21894=CARTESIAN_POINT('Ctrl Pts',(2.69980383625015,-41.2102568187956,18.));
#21895=CARTESIAN_POINT('Ctrl Pts',(2.73494956725005,-41.1165384061145,0.));
#21896=CARTESIAN_POINT('Ctrl Pts',(2.73494956725005,-41.1165384061145,18.));
#21897=CARTESIAN_POINT('Ctrl Pts',(2.76949151194863,-41.0227421242398,0.));
#21898=CARTESIAN_POINT('Ctrl Pts',(2.76949151194863,-41.0227421242398,18.));
#21899=CARTESIAN_POINT('Ctrl Pts',(2.80342531768404,-40.9288696352159,0.));
#21900=CARTESIAN_POINT('Ctrl Pts',(2.80342531768404,-40.9288696352159,18.));
#21901=CARTESIAN_POINT('Ctrl Pts',(2.83674635946678,-40.8349226258683,0.));
#21902=CARTESIAN_POINT('Ctrl Pts',(2.83674635946678,-40.8349226258683,18.));
#21903=CARTESIAN_POINT('Ctrl Pts',(2.86944892209897,-40.7409028213129,0.));
#21904=CARTESIAN_POINT('Ctrl Pts',(2.86944892209897,-40.7409028213129,18.));
#21905=CARTESIAN_POINT('Ctrl Pts',(2.90152548734342,-40.6468119976928,0.));
#21906=CARTESIAN_POINT('Ctrl Pts',(2.90152548734342,-40.6468119976928,18.));
#21907=CARTESIAN_POINT('Ctrl Pts',(2.93296560822893,-40.5526520010651,0.));
#21908=CARTESIAN_POINT('Ctrl Pts',(2.93296560822893,-40.5526520010651,18.));
#21909=CARTESIAN_POINT('Ctrl Pts',(2.96375636417322,-40.4584247445196,0.));
#21910=CARTESIAN_POINT('Ctrl Pts',(2.96375636417322,-40.4584247445196,18.));
#21911=CARTESIAN_POINT('Ctrl Pts',(2.99388446458219,-40.3641321823444,0.));
#21912=CARTESIAN_POINT('Ctrl Pts',(2.99388446458219,-40.3641321823444,18.));
#21913=CARTESIAN_POINT('Ctrl Pts',(3.02333808901594,-40.2697762886113,0.));
#21914=CARTESIAN_POINT('Ctrl Pts',(3.02333808901594,-40.2697762886113,18.));
#21915=CARTESIAN_POINT('Ctrl Pts',(3.0521084742307,-40.1753590391515,0.));
#21916=CARTESIAN_POINT('Ctrl Pts',(3.0521084742307,-40.1753590391515,18.));
#21917=CARTESIAN_POINT('Ctrl Pts',(3.08019251155015,-40.0808823811787,0.));
#21918=CARTESIAN_POINT('Ctrl Pts',(3.08019251155015,-40.0808823811787,18.));
#21919=CARTESIAN_POINT('Ctrl Pts',(3.10759149802907,-39.9863482523153,0.));
#21920=CARTESIAN_POINT('Ctrl Pts',(3.10759149802907,-39.9863482523153,18.));
#21921=CARTESIAN_POINT('Ctrl Pts',(3.13430604330355,-39.8917586491576,0.));
#21922=CARTESIAN_POINT('Ctrl Pts',(3.13430604330355,-39.8917586491576,18.));
#21923=CARTESIAN_POINT('Ctrl Pts',(3.16033160752803,-39.7971156880138,0.));
#21924=CARTESIAN_POINT('Ctrl Pts',(3.16033160752803,-39.7971156880138,18.));
#21925=CARTESIAN_POINT('Ctrl Pts',(3.18565465503835,-39.7024216585552,0.));
#21926=CARTESIAN_POINT('Ctrl Pts',(3.18565465503835,-39.7024216585552,18.));
#21927=CARTESIAN_POINT('Ctrl Pts',(3.21024640045595,-39.607679107639,0.));
#21928=CARTESIAN_POINT('Ctrl Pts',(3.21024640045595,-39.607679107639,18.));
#21929=CARTESIAN_POINT('Ctrl Pts',(3.2340660969166,-39.5128908052622,0.));
#21930=CARTESIAN_POINT('Ctrl Pts',(3.2340660969166,-39.5128908052622,18.));
#21931=CARTESIAN_POINT('Ctrl Pts',(3.25707264313387,-39.4180596080755,0.));
#21932=CARTESIAN_POINT('Ctrl Pts',(3.25707264313387,-39.4180596080755,18.));
#21933=CARTESIAN_POINT('Ctrl Pts',(3.27923485388116,-39.3231883392913,0.));
#21934=CARTESIAN_POINT('Ctrl Pts',(3.27923485388116,-39.3231883392913,18.));
#21935=CARTESIAN_POINT('Ctrl Pts',(3.30054018081687,-39.2282796893977,0.));
#21936=CARTESIAN_POINT('Ctrl Pts',(3.30054018081687,-39.2282796893977,18.));
#21937=CARTESIAN_POINT('Ctrl Pts',(3.32100933979557,-39.1333360409949,0.));
#21938=CARTESIAN_POINT('Ctrl Pts',(3.32100933979557,-39.1333360409949,18.));
#21939=CARTESIAN_POINT('Ctrl Pts',(3.34068601264472,-39.0383596151636,0.));
#21940=CARTESIAN_POINT('Ctrl Pts',(3.34068601264472,-39.0383596151636,18.));
#21941=CARTESIAN_POINT('Ctrl Pts',(3.3596092279948,-38.9433528420174,0.));
#21942=CARTESIAN_POINT('Ctrl Pts',(3.3596092279948,-38.9433528420174,18.));
#21943=CARTESIAN_POINT('Ctrl Pts',(3.37778863054481,-38.8483186930884,0.));
#21944=CARTESIAN_POINT('Ctrl Pts',(3.37778863054481,-38.8483186930884,18.));
#21945=CARTESIAN_POINT('Ctrl Pts',(3.39518333281817,-38.7532609709905,0.));
#21946=CARTESIAN_POINT('Ctrl Pts',(3.39518333281817,-38.7532609709905,18.));
#21947=CARTESIAN_POINT('Ctrl Pts',(3.411667175119,-38.6581847668347,0.));
#21948=CARTESIAN_POINT('Ctrl Pts',(3.411667175119,-38.6581847668347,18.));
#21949=CARTESIAN_POINT('Ctrl Pts',(3.42705871084996,-38.5630961226878,0.));
#21950=CARTESIAN_POINT('Ctrl Pts',(3.42705871084996,-38.5630961226878,18.));
#21951=CARTESIAN_POINT('Ctrl Pts',(3.44118343200302,-38.4680013094732,0.));
#21952=CARTESIAN_POINT('Ctrl Pts',(3.44118343200302,-38.4680013094732,18.));
#21953=CARTESIAN_POINT('Ctrl Pts',(3.45393053211022,-38.3729061502716,0.));
#21954=CARTESIAN_POINT('Ctrl Pts',(3.45393053211022,-38.3729061502716,18.));
#21955=CARTESIAN_POINT('Ctrl Pts',(3.46530185256872,-38.2778154909527,0.));
#21956=CARTESIAN_POINT('Ctrl Pts',(3.46530185256872,-38.2778154909527,18.));
#21957=CARTESIAN_POINT('Ctrl Pts',(3.47549027265411,-38.1827321816559,0.));
#21958=CARTESIAN_POINT('Ctrl Pts',(3.47549027265411,-38.1827321816559,18.));
#21959=CARTESIAN_POINT('Ctrl Pts',(3.48478279878233,-38.0876589224537,0.));
#21960=CARTESIAN_POINT('Ctrl Pts',(3.48478279878233,-38.0876589224537,18.));
#21961=CARTESIAN_POINT('Ctrl Pts',(3.49340804454645,-37.9926009950482,0.));
#21962=CARTESIAN_POINT('Ctrl Pts',(3.49340804454645,-37.9926009950482,18.));
#21963=CARTESIAN_POINT('Ctrl Pts',(3.50139628556083,-37.8975688353863,0.));
#21964=CARTESIAN_POINT('Ctrl Pts',(3.50139628556083,-37.8975688353863,18.));
#21965=CARTESIAN_POINT('Ctrl Pts',(3.50844720825127,-37.8025803811856,0.));
#21966=CARTESIAN_POINT('Ctrl Pts',(3.50844720825127,-37.8025803811856,18.));
#21967=CARTESIAN_POINT('Ctrl Pts',(3.51375922979957,-37.7076643105286,0.));
#21968=CARTESIAN_POINT('Ctrl Pts',(3.51375922979957,-37.7076643105286,18.));
#21969=CARTESIAN_POINT('Ctrl Pts',(3.51624243734644,-37.6128545966533,0.));
#21970=CARTESIAN_POINT('Ctrl Pts',(3.51624243734644,-37.6128545966533,18.));
#21971=CARTESIAN_POINT('Ctrl Pts',(3.51508109065209,-37.5371179004295,0.));
#21972=CARTESIAN_POINT('Ctrl Pts',(3.51508109065209,-37.5371179004295,18.));
#21973=CARTESIAN_POINT('Ctrl Pts',(3.5120473187636,-37.4803889700239,0.));
#21974=CARTESIAN_POINT('Ctrl Pts',(3.5120473187636,-37.4803889700239,18.));
#21975=CARTESIAN_POINT('Ctrl Pts',(3.50901346997656,-37.4426037737699,0.));
#21976=CARTESIAN_POINT('Ctrl Pts',(3.50901346997656,-37.4426037737699,18.));
#21977=CARTESIAN_POINT('Ctrl Pts',(3.50724370857672,-37.4237196983922,0.));
#21978=CARTESIAN_POINT('Ctrl Pts',(3.50724370857672,-37.4237196983922,18.));
#21979=CARTESIAN_POINT('',(1.38952890043928,-43.9780537249529,0.));
#21980=CARTESIAN_POINT('Ctrl Pts',(3.50724370857672,-37.4237196983922,0.));
#21981=CARTESIAN_POINT('Ctrl Pts',(3.50901346997656,-37.4426037737699,0.));
#21982=CARTESIAN_POINT('Ctrl Pts',(3.5120473187636,-37.4803889700239,0.));
#21983=CARTESIAN_POINT('Ctrl Pts',(3.51508109065209,-37.5371179004295,0.));
#21984=CARTESIAN_POINT('Ctrl Pts',(3.51624243734644,-37.6128545966533,0.));
#21985=CARTESIAN_POINT('Ctrl Pts',(3.51375922979957,-37.7076643105286,0.));
#21986=CARTESIAN_POINT('Ctrl Pts',(3.50844720825127,-37.8025803811856,0.));
#21987=CARTESIAN_POINT('Ctrl Pts',(3.50139628556083,-37.8975688353863,0.));
#21988=CARTESIAN_POINT('Ctrl Pts',(3.49340804454645,-37.9926009950482,0.));
#21989=CARTESIAN_POINT('Ctrl Pts',(3.48478279878233,-38.0876589224537,0.));
#21990=CARTESIAN_POINT('Ctrl Pts',(3.47549027265411,-38.1827321816559,0.));
#21991=CARTESIAN_POINT('Ctrl Pts',(3.46530185256872,-38.2778154909527,0.));
#21992=CARTESIAN_POINT('Ctrl Pts',(3.45393053211022,-38.3729061502716,0.));
#21993=CARTESIAN_POINT('Ctrl Pts',(3.44118343200302,-38.4680013094732,0.));
#21994=CARTESIAN_POINT('Ctrl Pts',(3.42705871084996,-38.5630961226878,0.));
#21995=CARTESIAN_POINT('Ctrl Pts',(3.411667175119,-38.6581847668347,0.));
#21996=CARTESIAN_POINT('Ctrl Pts',(3.39518333281817,-38.7532609709905,0.));
#21997=CARTESIAN_POINT('Ctrl Pts',(3.37778863054481,-38.8483186930884,0.));
#21998=CARTESIAN_POINT('Ctrl Pts',(3.3596092279948,-38.9433528420174,0.));
#21999=CARTESIAN_POINT('Ctrl Pts',(3.34068601264472,-39.0383596151636,0.));
#22000=CARTESIAN_POINT('Ctrl Pts',(3.32100933979557,-39.1333360409949,0.));
#22001=CARTESIAN_POINT('Ctrl Pts',(3.30054018081687,-39.2282796893977,0.));
#22002=CARTESIAN_POINT('Ctrl Pts',(3.27923485388116,-39.3231883392913,0.));
#22003=CARTESIAN_POINT('Ctrl Pts',(3.25707264313387,-39.4180596080755,0.));
#22004=CARTESIAN_POINT('Ctrl Pts',(3.2340660969166,-39.5128908052622,0.));
#22005=CARTESIAN_POINT('Ctrl Pts',(3.21024640045595,-39.607679107639,0.));
#22006=CARTESIAN_POINT('Ctrl Pts',(3.18565465503835,-39.7024216585552,0.));
#22007=CARTESIAN_POINT('Ctrl Pts',(3.16033160752803,-39.7971156880138,0.));
#22008=CARTESIAN_POINT('Ctrl Pts',(3.13430604330355,-39.8917586491576,0.));
#22009=CARTESIAN_POINT('Ctrl Pts',(3.10759149802907,-39.9863482523153,0.));
#22010=CARTESIAN_POINT('Ctrl Pts',(3.08019251155015,-40.0808823811787,0.));
#22011=CARTESIAN_POINT('Ctrl Pts',(3.0521084742307,-40.1753590391515,0.));
#22012=CARTESIAN_POINT('Ctrl Pts',(3.02333808901594,-40.2697762886113,0.));
#22013=CARTESIAN_POINT('Ctrl Pts',(2.99388446458219,-40.3641321823444,0.));
#22014=CARTESIAN_POINT('Ctrl Pts',(2.96375636417322,-40.4584247445196,0.));
#22015=CARTESIAN_POINT('Ctrl Pts',(2.93296560822893,-40.5526520010651,0.));
#22016=CARTESIAN_POINT('Ctrl Pts',(2.90152548734342,-40.6468119976928,0.));
#22017=CARTESIAN_POINT('Ctrl Pts',(2.86944892209897,-40.7409028213129,0.));
#22018=CARTESIAN_POINT('Ctrl Pts',(2.83674635946678,-40.8349226258683,0.));
#22019=CARTESIAN_POINT('Ctrl Pts',(2.80342531768404,-40.9288696352159,0.));
#22020=CARTESIAN_POINT('Ctrl Pts',(2.76949151194863,-41.0227421242398,0.));
#22021=CARTESIAN_POINT('Ctrl Pts',(2.73494956725005,-41.1165384061145,0.));
#22022=CARTESIAN_POINT('Ctrl Pts',(2.69980383625015,-41.2102568187956,0.));
#22023=CARTESIAN_POINT('Ctrl Pts',(2.66405934050117,-41.3038957096306,0.));
#22024=CARTESIAN_POINT('Ctrl Pts',(2.62772200460655,-41.3974534325936,0.));
#22025=CARTESIAN_POINT('Ctrl Pts',(2.59079818040171,-41.4909283577703,0.));
#22026=CARTESIAN_POINT('Ctrl Pts',(2.55329436064183,-41.5843188786284,0.));
#22027=CARTESIAN_POINT('Ctrl Pts',(2.51521684674476,-41.6776234194583,0.));
#22028=CARTESIAN_POINT('Ctrl Pts',(2.47657137427692,-41.7708404467533,0.));
#22029=CARTESIAN_POINT('Ctrl Pts',(2.437363014342,-41.8639684667923,0.));
#22030=CARTESIAN_POINT('Ctrl Pts',(2.39759639399648,-41.9570060084039,0.));
#22031=CARTESIAN_POINT('Ctrl Pts',(2.35727584066428,-42.0499516093661,0.));
#22032=CARTESIAN_POINT('Ctrl Pts',(2.31640554742808,-42.1428038039937,0.));
#22033=CARTESIAN_POINT('Ctrl Pts',(2.27498976664773,-42.2355611060784,0.));
#22034=CARTESIAN_POINT('Ctrl Pts',(2.23303287465499,-42.3282220118033,0.));
#22035=CARTESIAN_POINT('Ctrl Pts',(2.19053924976737,-42.4207850290047,0.));
#22036=CARTESIAN_POINT('Ctrl Pts',(2.14751319676745,-42.5132487024335,0.));
#22037=CARTESIAN_POINT('Ctrl Pts',(2.1039588640177,-42.6056116373455,0.));
#22038=CARTESIAN_POINT('Ctrl Pts',(2.05988014924518,-42.6978725343209,0.));
#22039=CARTESIAN_POINT('Ctrl Pts',(2.01528067528089,-42.7900301875309,0.));
#22040=CARTESIAN_POINT('Ctrl Pts',(1.97016390194215,-42.8820834139973,0.));
#22041=CARTESIAN_POINT('Ctrl Pts',(1.92453321512435,-42.9740309956624,0.));
#22042=CARTESIAN_POINT('Ctrl Pts',(1.87839202014608,-43.065871623255,0.));
#22043=CARTESIAN_POINT('Ctrl Pts',(1.83174385734711,-43.1576038253643,0.));
#22044=CARTESIAN_POINT('Ctrl Pts',(1.78459244842769,-43.2492259505872,0.));
#22045=CARTESIAN_POINT('Ctrl Pts',(1.73694151741123,-43.3407363140236,0.));
#22046=CARTESIAN_POINT('Ctrl Pts',(1.68879465270607,-43.4321333178711,0.));
#22047=CARTESIAN_POINT('Ctrl Pts',(1.64015515906647,-43.5234155788248,0.));
#22048=CARTESIAN_POINT('Ctrl Pts',(1.59102591108103,-43.6145820637333,0.));
#22049=CARTESIAN_POINT('Ctrl Pts',(1.53148589036096,-43.7238422193529,0.));
#22050=CARTESIAN_POINT('Ctrl Pts',(1.48126213998558,-43.8147465842503,0.));
#22051=CARTESIAN_POINT('Ctrl Pts',(1.44069595482722,-43.8873767449247,0.));
#22052=CARTESIAN_POINT('Ctrl Pts',(1.41005374202873,-43.9417969186811,0.));
#22053=CARTESIAN_POINT('Ctrl Pts',(1.38952890043915,-43.9780537249529,0.));
#22054=CARTESIAN_POINT('',(1.38952890043928,-43.9780537249529,15.));
#22055=CARTESIAN_POINT('Ctrl Pts',(1.38952890043915,-43.9780537249529,15.));
#22056=CARTESIAN_POINT('Ctrl Pts',(1.3997913212193,-43.9599253218252,15.));
#22057=CARTESIAN_POINT('Ctrl Pts',(1.42026781296156,-43.9236568607623,15.));
#22058=CARTESIAN_POINT('Ctrl Pts',(1.45083750111681,-43.8692192047561,15.));
#22059=CARTESIAN_POINT('Ctrl Pts',(1.49130689006066,-43.7965657112708,15.));
#22060=CARTESIAN_POINT('Ctrl Pts',(1.54140922714764,-43.7056321934163,15.));
#22061=CARTESIAN_POINT('Ctrl Pts',(1.59102591108103,-43.6145820637333,15.));
#22062=CARTESIAN_POINT('Ctrl Pts',(1.64015515906647,-43.5234155788248,15.));
#22063=CARTESIAN_POINT('Ctrl Pts',(1.68879465270607,-43.4321333178711,15.));
#22064=CARTESIAN_POINT('Ctrl Pts',(1.73694151741123,-43.3407363140236,15.));
#22065=CARTESIAN_POINT('Ctrl Pts',(1.78459244842769,-43.2492259505872,15.));
#22066=CARTESIAN_POINT('Ctrl Pts',(1.83174385734711,-43.1576038253643,15.));
#22067=CARTESIAN_POINT('Ctrl Pts',(1.87839202014608,-43.065871623255,15.));
#22068=CARTESIAN_POINT('Ctrl Pts',(1.92453321512435,-42.9740309956624,15.));
#22069=CARTESIAN_POINT('Ctrl Pts',(1.97016390194215,-42.8820834139973,15.));
#22070=CARTESIAN_POINT('Ctrl Pts',(2.01528067528089,-42.7900301875309,15.));
#22071=CARTESIAN_POINT('Ctrl Pts',(2.05988014924518,-42.6978725343209,15.));
#22072=CARTESIAN_POINT('Ctrl Pts',(2.1039588640177,-42.6056116373455,15.));
#22073=CARTESIAN_POINT('Ctrl Pts',(2.14751319676745,-42.5132487024335,15.));
#22074=CARTESIAN_POINT('Ctrl Pts',(2.19053924976737,-42.4207850290047,15.));
#22075=CARTESIAN_POINT('Ctrl Pts',(2.23303287465499,-42.3282220118033,15.));
#22076=CARTESIAN_POINT('Ctrl Pts',(2.27498976664773,-42.2355611060784,15.));
#22077=CARTESIAN_POINT('Ctrl Pts',(2.31640554742808,-42.1428038039937,15.));
#22078=CARTESIAN_POINT('Ctrl Pts',(2.35727584066428,-42.0499516093661,15.));
#22079=CARTESIAN_POINT('Ctrl Pts',(2.39759639399648,-41.9570060084039,15.));
#22080=CARTESIAN_POINT('Ctrl Pts',(2.437363014342,-41.8639684667923,15.));
#22081=CARTESIAN_POINT('Ctrl Pts',(2.47657137427692,-41.7708404467533,15.));
#22082=CARTESIAN_POINT('Ctrl Pts',(2.51521684674476,-41.6776234194583,15.));
#22083=CARTESIAN_POINT('Ctrl Pts',(2.55329436064183,-41.5843188786284,15.));
#22084=CARTESIAN_POINT('Ctrl Pts',(2.59079818040171,-41.4909283577703,15.));
#22085=CARTESIAN_POINT('Ctrl Pts',(2.62772200460655,-41.3974534325936,15.));
#22086=CARTESIAN_POINT('Ctrl Pts',(2.66405934050117,-41.3038957096306,15.));
#22087=CARTESIAN_POINT('Ctrl Pts',(2.69980383625015,-41.2102568187956,15.));
#22088=CARTESIAN_POINT('Ctrl Pts',(2.73494956725005,-41.1165384061145,15.));
#22089=CARTESIAN_POINT('Ctrl Pts',(2.76949151194863,-41.0227421242398,15.));
#22090=CARTESIAN_POINT('Ctrl Pts',(2.80342531768404,-40.9288696352159,15.));
#22091=CARTESIAN_POINT('Ctrl Pts',(2.83674635946678,-40.8349226258683,15.));
#22092=CARTESIAN_POINT('Ctrl Pts',(2.86944892209897,-40.7409028213129,15.));
#22093=CARTESIAN_POINT('Ctrl Pts',(2.90152548734342,-40.6468119976928,15.));
#22094=CARTESIAN_POINT('Ctrl Pts',(2.93296560822893,-40.5526520010651,15.));
#22095=CARTESIAN_POINT('Ctrl Pts',(2.96375636417322,-40.4584247445196,15.));
#22096=CARTESIAN_POINT('Ctrl Pts',(2.99388446458219,-40.3641321823444,15.));
#22097=CARTESIAN_POINT('Ctrl Pts',(3.02333808901594,-40.2697762886113,15.));
#22098=CARTESIAN_POINT('Ctrl Pts',(3.0521084742307,-40.1753590391515,15.));
#22099=CARTESIAN_POINT('Ctrl Pts',(3.08019251155015,-40.0808823811787,15.));
#22100=CARTESIAN_POINT('Ctrl Pts',(3.10759149802907,-39.9863482523153,15.));
#22101=CARTESIAN_POINT('Ctrl Pts',(3.13430604330355,-39.8917586491576,15.));
#22102=CARTESIAN_POINT('Ctrl Pts',(3.16033160752803,-39.7971156880138,15.));
#22103=CARTESIAN_POINT('Ctrl Pts',(3.18565465503835,-39.7024216585552,15.));
#22104=CARTESIAN_POINT('Ctrl Pts',(3.21024640045595,-39.607679107639,15.));
#22105=CARTESIAN_POINT('Ctrl Pts',(3.2340660969166,-39.5128908052622,15.));
#22106=CARTESIAN_POINT('Ctrl Pts',(3.25707264313387,-39.4180596080755,15.));
#22107=CARTESIAN_POINT('Ctrl Pts',(3.27923485388116,-39.3231883392913,15.));
#22108=CARTESIAN_POINT('Ctrl Pts',(3.30054018081687,-39.2282796893977,15.));
#22109=CARTESIAN_POINT('Ctrl Pts',(3.32100933979557,-39.1333360409949,15.));
#22110=CARTESIAN_POINT('Ctrl Pts',(3.34068601264472,-39.0383596151636,15.));
#22111=CARTESIAN_POINT('Ctrl Pts',(3.3596092279948,-38.9433528420174,15.));
#22112=CARTESIAN_POINT('Ctrl Pts',(3.37778863054481,-38.8483186930884,15.));
#22113=CARTESIAN_POINT('Ctrl Pts',(3.39518333281817,-38.7532609709905,15.));
#22114=CARTESIAN_POINT('Ctrl Pts',(3.411667175119,-38.6581847668347,15.));
#22115=CARTESIAN_POINT('Ctrl Pts',(3.42705871084996,-38.5630961226878,15.));
#22116=CARTESIAN_POINT('Ctrl Pts',(3.44118343200302,-38.4680013094732,15.));
#22117=CARTESIAN_POINT('Ctrl Pts',(3.45393053211022,-38.3729061502716,15.));
#22118=CARTESIAN_POINT('Ctrl Pts',(3.46530185256872,-38.2778154909527,15.));
#22119=CARTESIAN_POINT('Ctrl Pts',(3.47549027265411,-38.1827321816559,15.));
#22120=CARTESIAN_POINT('Ctrl Pts',(3.48478279878233,-38.0876589224537,15.));
#22121=CARTESIAN_POINT('Ctrl Pts',(3.49340804454645,-37.9926009950482,15.));
#22122=CARTESIAN_POINT('Ctrl Pts',(3.50139628556083,-37.8975688353863,15.));
#22123=CARTESIAN_POINT('Ctrl Pts',(3.50844720825127,-37.8025803811856,15.));
#22124=CARTESIAN_POINT('Ctrl Pts',(3.51375922979957,-37.7076643105286,15.));
#22125=CARTESIAN_POINT('Ctrl Pts',(3.51624243734644,-37.6128545966533,15.));
#22126=CARTESIAN_POINT('Ctrl Pts',(3.51508109065209,-37.5371179004295,15.));
#22127=CARTESIAN_POINT('Ctrl Pts',(3.5120473187636,-37.4803889700239,15.));
#22128=CARTESIAN_POINT('Ctrl Pts',(3.50901346997656,-37.4426037737699,15.));
#22129=CARTESIAN_POINT('Ctrl Pts',(3.50724370857672,-37.4237196983922,15.));
#22130=CARTESIAN_POINT('',(1.38952890043928,-43.9780537249529,0.));
#22131=CARTESIAN_POINT('Origin',(-2.01948391736579E-27,-1.13331566353736E-11,
0.));
#22132=CARTESIAN_POINT('',(-1.38952890043917,-43.9780537249529,0.));
#22133=CARTESIAN_POINT('Origin',(-2.01948391736579E-27,-1.13331566353736E-11,
0.));
#22134=CARTESIAN_POINT('',(-1.38952890043917,-43.9780537249529,15.));
#22135=CARTESIAN_POINT('Origin',(-2.01948391736579E-27,-1.13331566353736E-11,
15.));
#22136=CARTESIAN_POINT('',(-1.38952890043917,-43.9780537249529,0.));
#22137=CARTESIAN_POINT('Ctrl Pts',(-3.50724370857673,-37.4237196983922,
0.));
#22138=CARTESIAN_POINT('Ctrl Pts',(-3.50724370857673,-37.4237196983922,
18.));
#22139=CARTESIAN_POINT('Ctrl Pts',(-3.50901346997657,-37.4426037737699,
0.));
#22140=CARTESIAN_POINT('Ctrl Pts',(-3.50901346997657,-37.4426037737699,
18.));
#22141=CARTESIAN_POINT('Ctrl Pts',(-3.51204731876362,-37.4803889700239,
0.));
#22142=CARTESIAN_POINT('Ctrl Pts',(-3.51204731876362,-37.4803889700239,
18.));
#22143=CARTESIAN_POINT('Ctrl Pts',(-3.51508109065211,-37.5371179004295,
0.));
#22144=CARTESIAN_POINT('Ctrl Pts',(-3.51508109065211,-37.5371179004295,
18.));
#22145=CARTESIAN_POINT('Ctrl Pts',(-3.51624243734646,-37.6128545966533,
0.));
#22146=CARTESIAN_POINT('Ctrl Pts',(-3.51624243734646,-37.6128545966533,
18.));
#22147=CARTESIAN_POINT('Ctrl Pts',(-3.51375922979958,-37.7076643105286,
0.));
#22148=CARTESIAN_POINT('Ctrl Pts',(-3.51375922979958,-37.7076643105286,
18.));
#22149=CARTESIAN_POINT('Ctrl Pts',(-3.50844720825129,-37.8025803811856,
0.));
#22150=CARTESIAN_POINT('Ctrl Pts',(-3.50844720825129,-37.8025803811856,
18.));
#22151=CARTESIAN_POINT('Ctrl Pts',(-3.50139628556084,-37.8975688353863,
0.));
#22152=CARTESIAN_POINT('Ctrl Pts',(-3.50139628556084,-37.8975688353863,
18.));
#22153=CARTESIAN_POINT('Ctrl Pts',(-3.49340804454646,-37.9926009950482,
0.));
#22154=CARTESIAN_POINT('Ctrl Pts',(-3.49340804454646,-37.9926009950482,
18.));
#22155=CARTESIAN_POINT('Ctrl Pts',(-3.48478279878234,-38.0876589224537,
0.));
#22156=CARTESIAN_POINT('Ctrl Pts',(-3.48478279878234,-38.0876589224537,
18.));
#22157=CARTESIAN_POINT('Ctrl Pts',(-3.47549027265412,-38.1827321816559,
0.));
#22158=CARTESIAN_POINT('Ctrl Pts',(-3.47549027265412,-38.1827321816559,
18.));
#22159=CARTESIAN_POINT('Ctrl Pts',(-3.46530185256873,-38.2778154909527,
0.));
#22160=CARTESIAN_POINT('Ctrl Pts',(-3.46530185256873,-38.2778154909527,
18.));
#22161=CARTESIAN_POINT('Ctrl Pts',(-3.45393053211023,-38.3729061502716,
0.));
#22162=CARTESIAN_POINT('Ctrl Pts',(-3.45393053211023,-38.3729061502716,
18.));
#22163=CARTESIAN_POINT('Ctrl Pts',(-3.44118343200304,-38.4680013094732,
0.));
#22164=CARTESIAN_POINT('Ctrl Pts',(-3.44118343200304,-38.4680013094732,
18.));
#22165=CARTESIAN_POINT('Ctrl Pts',(-3.42705871084998,-38.5630961226878,
0.));
#22166=CARTESIAN_POINT('Ctrl Pts',(-3.42705871084998,-38.5630961226878,
18.));
#22167=CARTESIAN_POINT('Ctrl Pts',(-3.41166717511902,-38.6581847668347,
0.));
#22168=CARTESIAN_POINT('Ctrl Pts',(-3.41166717511902,-38.6581847668347,
18.));
#22169=CARTESIAN_POINT('Ctrl Pts',(-3.39518333281819,-38.7532609709905,
0.));
#22170=CARTESIAN_POINT('Ctrl Pts',(-3.39518333281819,-38.7532609709905,
18.));
#22171=CARTESIAN_POINT('Ctrl Pts',(-3.37778863054483,-38.8483186930884,
0.));
#22172=CARTESIAN_POINT('Ctrl Pts',(-3.37778863054483,-38.8483186930884,
18.));
#22173=CARTESIAN_POINT('Ctrl Pts',(-3.35960922799482,-38.9433528420174,
0.));
#22174=CARTESIAN_POINT('Ctrl Pts',(-3.35960922799482,-38.9433528420174,
18.));
#22175=CARTESIAN_POINT('Ctrl Pts',(-3.34068601264473,-39.0383596151636,
0.));
#22176=CARTESIAN_POINT('Ctrl Pts',(-3.34068601264473,-39.0383596151636,
18.));
#22177=CARTESIAN_POINT('Ctrl Pts',(-3.32100933979558,-39.1333360409949,
0.));
#22178=CARTESIAN_POINT('Ctrl Pts',(-3.32100933979558,-39.1333360409949,
18.));
#22179=CARTESIAN_POINT('Ctrl Pts',(-3.30054018081688,-39.2282796893977,
0.));
#22180=CARTESIAN_POINT('Ctrl Pts',(-3.30054018081688,-39.2282796893977,
18.));
#22181=CARTESIAN_POINT('Ctrl Pts',(-3.27923485388118,-39.3231883392913,
0.));
#22182=CARTESIAN_POINT('Ctrl Pts',(-3.27923485388118,-39.3231883392913,
18.));
#22183=CARTESIAN_POINT('Ctrl Pts',(-3.25707264313389,-39.4180596080755,
0.));
#22184=CARTESIAN_POINT('Ctrl Pts',(-3.25707264313389,-39.4180596080755,
18.));
#22185=CARTESIAN_POINT('Ctrl Pts',(-3.23406609691662,-39.5128908052622,
0.));
#22186=CARTESIAN_POINT('Ctrl Pts',(-3.23406609691662,-39.5128908052622,
18.));
#22187=CARTESIAN_POINT('Ctrl Pts',(-3.21024640045596,-39.607679107639,0.));
#22188=CARTESIAN_POINT('Ctrl Pts',(-3.21024640045596,-39.607679107639,18.));
#22189=CARTESIAN_POINT('Ctrl Pts',(-3.18565465503836,-39.7024216585552,
0.));
#22190=CARTESIAN_POINT('Ctrl Pts',(-3.18565465503836,-39.7024216585552,
18.));
#22191=CARTESIAN_POINT('Ctrl Pts',(-3.16033160752805,-39.7971156880138,
0.));
#22192=CARTESIAN_POINT('Ctrl Pts',(-3.16033160752805,-39.7971156880138,
18.));
#22193=CARTESIAN_POINT('Ctrl Pts',(-3.13430604330357,-39.8917586491576,
0.));
#22194=CARTESIAN_POINT('Ctrl Pts',(-3.13430604330357,-39.8917586491576,
18.));
#22195=CARTESIAN_POINT('Ctrl Pts',(-3.10759149802909,-39.9863482523153,
0.));
#22196=CARTESIAN_POINT('Ctrl Pts',(-3.10759149802909,-39.9863482523153,
18.));
#22197=CARTESIAN_POINT('Ctrl Pts',(-3.08019251155016,-40.0808823811787,
0.));
#22198=CARTESIAN_POINT('Ctrl Pts',(-3.08019251155016,-40.0808823811787,
18.));
#22199=CARTESIAN_POINT('Ctrl Pts',(-3.05210847423072,-40.1753590391515,
0.));
#22200=CARTESIAN_POINT('Ctrl Pts',(-3.05210847423072,-40.1753590391515,
18.));
#22201=CARTESIAN_POINT('Ctrl Pts',(-3.02333808901596,-40.2697762886113,
0.));
#22202=CARTESIAN_POINT('Ctrl Pts',(-3.02333808901596,-40.2697762886113,
18.));
#22203=CARTESIAN_POINT('Ctrl Pts',(-2.9938844645822,-40.3641321823444,0.));
#22204=CARTESIAN_POINT('Ctrl Pts',(-2.9938844645822,-40.3641321823444,18.));
#22205=CARTESIAN_POINT('Ctrl Pts',(-2.96375636417323,-40.4584247445196,
0.));
#22206=CARTESIAN_POINT('Ctrl Pts',(-2.96375636417323,-40.4584247445196,
18.));
#22207=CARTESIAN_POINT('Ctrl Pts',(-2.93296560822894,-40.5526520010651,
0.));
#22208=CARTESIAN_POINT('Ctrl Pts',(-2.93296560822894,-40.5526520010651,
18.));
#22209=CARTESIAN_POINT('Ctrl Pts',(-2.90152548734344,-40.6468119976928,
0.));
#22210=CARTESIAN_POINT('Ctrl Pts',(-2.90152548734344,-40.6468119976928,
18.));
#22211=CARTESIAN_POINT('Ctrl Pts',(-2.86944892209898,-40.7409028213129,
0.));
#22212=CARTESIAN_POINT('Ctrl Pts',(-2.86944892209898,-40.7409028213129,
18.));
#22213=CARTESIAN_POINT('Ctrl Pts',(-2.8367463594668,-40.8349226258683,0.));
#22214=CARTESIAN_POINT('Ctrl Pts',(-2.8367463594668,-40.8349226258683,18.));
#22215=CARTESIAN_POINT('Ctrl Pts',(-2.80342531768406,-40.9288696352159,
0.));
#22216=CARTESIAN_POINT('Ctrl Pts',(-2.80342531768406,-40.9288696352159,
18.));
#22217=CARTESIAN_POINT('Ctrl Pts',(-2.76949151194864,-41.0227421242398,
0.));
#22218=CARTESIAN_POINT('Ctrl Pts',(-2.76949151194864,-41.0227421242398,
18.));
#22219=CARTESIAN_POINT('Ctrl Pts',(-2.73494956725006,-41.1165384061145,
0.));
#22220=CARTESIAN_POINT('Ctrl Pts',(-2.73494956725006,-41.1165384061145,
18.));
#22221=CARTESIAN_POINT('Ctrl Pts',(-2.69980383625016,-41.2102568187956,
0.));
#22222=CARTESIAN_POINT('Ctrl Pts',(-2.69980383625016,-41.2102568187956,
18.));
#22223=CARTESIAN_POINT('Ctrl Pts',(-2.66405934050119,-41.3038957096306,
0.));
#22224=CARTESIAN_POINT('Ctrl Pts',(-2.66405934050119,-41.3038957096306,
18.));
#22225=CARTESIAN_POINT('Ctrl Pts',(-2.62772200460657,-41.3974534325936,
0.));
#22226=CARTESIAN_POINT('Ctrl Pts',(-2.62772200460657,-41.3974534325936,
18.));
#22227=CARTESIAN_POINT('Ctrl Pts',(-2.59079818040173,-41.4909283577703,
0.));
#22228=CARTESIAN_POINT('Ctrl Pts',(-2.59079818040173,-41.4909283577703,
18.));
#22229=CARTESIAN_POINT('Ctrl Pts',(-2.55329436064185,-41.5843188786284,
0.));
#22230=CARTESIAN_POINT('Ctrl Pts',(-2.55329436064185,-41.5843188786284,
18.));
#22231=CARTESIAN_POINT('Ctrl Pts',(-2.51521684674478,-41.6776234194583,
0.));
#22232=CARTESIAN_POINT('Ctrl Pts',(-2.51521684674478,-41.6776234194583,
18.));
#22233=CARTESIAN_POINT('Ctrl Pts',(-2.47657137427694,-41.7708404467533,
0.));
#22234=CARTESIAN_POINT('Ctrl Pts',(-2.47657137427694,-41.7708404467533,
18.));
#22235=CARTESIAN_POINT('Ctrl Pts',(-2.43736301434201,-41.8639684667923,
0.));
#22236=CARTESIAN_POINT('Ctrl Pts',(-2.43736301434201,-41.8639684667923,
18.));
#22237=CARTESIAN_POINT('Ctrl Pts',(-2.39759639399649,-41.9570060084039,
0.));
#22238=CARTESIAN_POINT('Ctrl Pts',(-2.39759639399649,-41.9570060084039,
18.));
#22239=CARTESIAN_POINT('Ctrl Pts',(-2.3572758406643,-42.0499516093661,0.));
#22240=CARTESIAN_POINT('Ctrl Pts',(-2.3572758406643,-42.0499516093661,18.));
#22241=CARTESIAN_POINT('Ctrl Pts',(-2.3164055474281,-42.1428038039937,0.));
#22242=CARTESIAN_POINT('Ctrl Pts',(-2.3164055474281,-42.1428038039937,18.));
#22243=CARTESIAN_POINT('Ctrl Pts',(-2.27498976664775,-42.2355611060784,
0.));
#22244=CARTESIAN_POINT('Ctrl Pts',(-2.27498976664775,-42.2355611060784,
18.));
#22245=CARTESIAN_POINT('Ctrl Pts',(-2.23303287465501,-42.3282220118033,
0.));
#22246=CARTESIAN_POINT('Ctrl Pts',(-2.23303287465501,-42.3282220118033,
18.));
#22247=CARTESIAN_POINT('Ctrl Pts',(-2.19053924976738,-42.4207850290047,
0.));
#22248=CARTESIAN_POINT('Ctrl Pts',(-2.19053924976738,-42.4207850290047,
18.));
#22249=CARTESIAN_POINT('Ctrl Pts',(-2.14751319676746,-42.5132487024335,
0.));
#22250=CARTESIAN_POINT('Ctrl Pts',(-2.14751319676746,-42.5132487024335,
18.));
#22251=CARTESIAN_POINT('Ctrl Pts',(-2.10395886401772,-42.6056116373455,
0.));
#22252=CARTESIAN_POINT('Ctrl Pts',(-2.10395886401772,-42.6056116373455,
18.));
#22253=CARTESIAN_POINT('Ctrl Pts',(-2.0598801492452,-42.6978725343209,0.));
#22254=CARTESIAN_POINT('Ctrl Pts',(-2.0598801492452,-42.6978725343209,18.));
#22255=CARTESIAN_POINT('Ctrl Pts',(-2.0152806752809,-42.7900301875309,0.));
#22256=CARTESIAN_POINT('Ctrl Pts',(-2.0152806752809,-42.7900301875309,18.));
#22257=CARTESIAN_POINT('Ctrl Pts',(-1.97016390194217,-42.8820834139973,
0.));
#22258=CARTESIAN_POINT('Ctrl Pts',(-1.97016390194217,-42.8820834139973,
18.));
#22259=CARTESIAN_POINT('Ctrl Pts',(-1.92453321512437,-42.9740309956624,
0.));
#22260=CARTESIAN_POINT('Ctrl Pts',(-1.92453321512437,-42.9740309956624,
18.));
#22261=CARTESIAN_POINT('Ctrl Pts',(-1.8783920201461,-43.065871623255,0.));
#22262=CARTESIAN_POINT('Ctrl Pts',(-1.8783920201461,-43.065871623255,18.));
#22263=CARTESIAN_POINT('Ctrl Pts',(-1.83174385734712,-43.1576038253643,
0.));
#22264=CARTESIAN_POINT('Ctrl Pts',(-1.83174385734712,-43.1576038253643,
18.));
#22265=CARTESIAN_POINT('Ctrl Pts',(-1.78459244842771,-43.2492259505872,
0.));
#22266=CARTESIAN_POINT('Ctrl Pts',(-1.78459244842771,-43.2492259505872,
18.));
#22267=CARTESIAN_POINT('Ctrl Pts',(-1.73694151741125,-43.3407363140236,
0.));
#22268=CARTESIAN_POINT('Ctrl Pts',(-1.73694151741125,-43.3407363140236,
18.));
#22269=CARTESIAN_POINT('Ctrl Pts',(-1.68879465270609,-43.4321333178711,
0.));
#22270=CARTESIAN_POINT('Ctrl Pts',(-1.68879465270609,-43.4321333178711,
18.));
#22271=CARTESIAN_POINT('Ctrl Pts',(-1.64015515906649,-43.5234155788248,
0.));
#22272=CARTESIAN_POINT('Ctrl Pts',(-1.64015515906649,-43.5234155788248,
18.));
#22273=CARTESIAN_POINT('Ctrl Pts',(-1.59102591108105,-43.6145820637333,
0.));
#22274=CARTESIAN_POINT('Ctrl Pts',(-1.59102591108105,-43.6145820637333,
18.));
#22275=CARTESIAN_POINT('Ctrl Pts',(-1.54140922714765,-43.7056321934163,
0.));
#22276=CARTESIAN_POINT('Ctrl Pts',(-1.54140922714765,-43.7056321934163,
18.));
#22277=CARTESIAN_POINT('Ctrl Pts',(-1.49130689006068,-43.7965657112708,
0.));
#22278=CARTESIAN_POINT('Ctrl Pts',(-1.49130689006068,-43.7965657112708,
18.));
#22279=CARTESIAN_POINT('Ctrl Pts',(-1.45083750111683,-43.8692192047561,
0.));
#22280=CARTESIAN_POINT('Ctrl Pts',(-1.45083750111683,-43.8692192047561,
18.));
#22281=CARTESIAN_POINT('Ctrl Pts',(-1.42026781296157,-43.9236568607623,
0.));
#22282=CARTESIAN_POINT('Ctrl Pts',(-1.42026781296157,-43.9236568607623,
18.));
#22283=CARTESIAN_POINT('Ctrl Pts',(-1.39979132121932,-43.9599253218251,
0.));
#22284=CARTESIAN_POINT('Ctrl Pts',(-1.39979132121932,-43.9599253218251,
18.));
#22285=CARTESIAN_POINT('Ctrl Pts',(-1.38952890043917,-43.9780537249529,
0.));
#22286=CARTESIAN_POINT('Ctrl Pts',(-1.38952890043917,-43.9780537249529,
18.));
#22287=CARTESIAN_POINT('Ctrl Pts',(-3.50724370857673,-37.4237196983922,
0.));
#22288=CARTESIAN_POINT('Ctrl Pts',(-3.50901346997657,-37.4426037737699,
0.));
#22289=CARTESIAN_POINT('Ctrl Pts',(-3.51204731876362,-37.4803889700239,
0.));
#22290=CARTESIAN_POINT('Ctrl Pts',(-3.51508109065211,-37.5371179004295,
0.));
#22291=CARTESIAN_POINT('Ctrl Pts',(-3.51624243734646,-37.6128545966533,
0.));
#22292=CARTESIAN_POINT('Ctrl Pts',(-3.51375922979958,-37.7076643105286,
0.));
#22293=CARTESIAN_POINT('Ctrl Pts',(-3.50844720825129,-37.8025803811856,
0.));
#22294=CARTESIAN_POINT('Ctrl Pts',(-3.50139628556084,-37.8975688353863,
0.));
#22295=CARTESIAN_POINT('Ctrl Pts',(-3.49340804454646,-37.9926009950482,
0.));
#22296=CARTESIAN_POINT('Ctrl Pts',(-3.48478279878234,-38.0876589224537,
0.));
#22297=CARTESIAN_POINT('Ctrl Pts',(-3.47549027265412,-38.1827321816559,
0.));
#22298=CARTESIAN_POINT('Ctrl Pts',(-3.46530185256873,-38.2778154909527,
0.));
#22299=CARTESIAN_POINT('Ctrl Pts',(-3.45393053211023,-38.3729061502716,
0.));
#22300=CARTESIAN_POINT('Ctrl Pts',(-3.44118343200304,-38.4680013094732,
0.));
#22301=CARTESIAN_POINT('Ctrl Pts',(-3.42705871084998,-38.5630961226878,
0.));
#22302=CARTESIAN_POINT('Ctrl Pts',(-3.41166717511902,-38.6581847668347,
0.));
#22303=CARTESIAN_POINT('Ctrl Pts',(-3.39518333281819,-38.7532609709905,
0.));
#22304=CARTESIAN_POINT('Ctrl Pts',(-3.37778863054483,-38.8483186930884,
0.));
#22305=CARTESIAN_POINT('Ctrl Pts',(-3.35960922799482,-38.9433528420174,
0.));
#22306=CARTESIAN_POINT('Ctrl Pts',(-3.34068601264473,-39.0383596151636,
0.));
#22307=CARTESIAN_POINT('Ctrl Pts',(-3.32100933979558,-39.1333360409949,
0.));
#22308=CARTESIAN_POINT('Ctrl Pts',(-3.30054018081688,-39.2282796893977,
0.));
#22309=CARTESIAN_POINT('Ctrl Pts',(-3.27923485388118,-39.3231883392913,
0.));
#22310=CARTESIAN_POINT('Ctrl Pts',(-3.25707264313389,-39.4180596080755,
0.));
#22311=CARTESIAN_POINT('Ctrl Pts',(-3.23406609691662,-39.5128908052622,
0.));
#22312=CARTESIAN_POINT('Ctrl Pts',(-3.21024640045596,-39.607679107639,0.));
#22313=CARTESIAN_POINT('Ctrl Pts',(-3.18565465503836,-39.7024216585552,
0.));
#22314=CARTESIAN_POINT('Ctrl Pts',(-3.16033160752805,-39.7971156880138,
0.));
#22315=CARTESIAN_POINT('Ctrl Pts',(-3.13430604330357,-39.8917586491576,
0.));
#22316=CARTESIAN_POINT('Ctrl Pts',(-3.10759149802909,-39.9863482523153,
0.));
#22317=CARTESIAN_POINT('Ctrl Pts',(-3.08019251155016,-40.0808823811787,
0.));
#22318=CARTESIAN_POINT('Ctrl Pts',(-3.05210847423072,-40.1753590391515,
0.));
#22319=CARTESIAN_POINT('Ctrl Pts',(-3.02333808901596,-40.2697762886113,
0.));
#22320=CARTESIAN_POINT('Ctrl Pts',(-2.9938844645822,-40.3641321823444,0.));
#22321=CARTESIAN_POINT('Ctrl Pts',(-2.96375636417323,-40.4584247445196,
0.));
#22322=CARTESIAN_POINT('Ctrl Pts',(-2.93296560822894,-40.5526520010651,
0.));
#22323=CARTESIAN_POINT('Ctrl Pts',(-2.90152548734344,-40.6468119976928,
0.));
#22324=CARTESIAN_POINT('Ctrl Pts',(-2.86944892209898,-40.7409028213129,
0.));
#22325=CARTESIAN_POINT('Ctrl Pts',(-2.8367463594668,-40.8349226258683,0.));
#22326=CARTESIAN_POINT('Ctrl Pts',(-2.80342531768406,-40.9288696352159,
0.));
#22327=CARTESIAN_POINT('Ctrl Pts',(-2.76949151194864,-41.0227421242398,
0.));
#22328=CARTESIAN_POINT('Ctrl Pts',(-2.73494956725006,-41.1165384061145,
0.));
#22329=CARTESIAN_POINT('Ctrl Pts',(-2.69980383625016,-41.2102568187956,
0.));
#22330=CARTESIAN_POINT('Ctrl Pts',(-2.66405934050119,-41.3038957096306,
0.));
#22331=CARTESIAN_POINT('Ctrl Pts',(-2.62772200460657,-41.3974534325936,
0.));
#22332=CARTESIAN_POINT('Ctrl Pts',(-2.59079818040173,-41.4909283577703,
0.));
#22333=CARTESIAN_POINT('Ctrl Pts',(-2.55329436064185,-41.5843188786284,
0.));
#22334=CARTESIAN_POINT('Ctrl Pts',(-2.51521684674478,-41.6776234194583,
0.));
#22335=CARTESIAN_POINT('Ctrl Pts',(-2.47657137427694,-41.7708404467533,
0.));
#22336=CARTESIAN_POINT('Ctrl Pts',(-2.43736301434201,-41.8639684667923,
0.));
#22337=CARTESIAN_POINT('Ctrl Pts',(-2.39759639399649,-41.9570060084039,
0.));
#22338=CARTESIAN_POINT('Ctrl Pts',(-2.3572758406643,-42.0499516093661,0.));
#22339=CARTESIAN_POINT('Ctrl Pts',(-2.3164055474281,-42.1428038039937,0.));
#22340=CARTESIAN_POINT('Ctrl Pts',(-2.27498976664775,-42.2355611060784,
0.));
#22341=CARTESIAN_POINT('Ctrl Pts',(-2.23303287465501,-42.3282220118033,
0.));
#22342=CARTESIAN_POINT('Ctrl Pts',(-2.19053924976738,-42.4207850290047,
0.));
#22343=CARTESIAN_POINT('Ctrl Pts',(-2.14751319676746,-42.5132487024335,
0.));
#22344=CARTESIAN_POINT('Ctrl Pts',(-2.10395886401772,-42.6056116373455,
0.));
#22345=CARTESIAN_POINT('Ctrl Pts',(-2.0598801492452,-42.6978725343209,0.));
#22346=CARTESIAN_POINT('Ctrl Pts',(-2.0152806752809,-42.7900301875309,0.));
#22347=CARTESIAN_POINT('Ctrl Pts',(-1.97016390194217,-42.8820834139973,
0.));
#22348=CARTESIAN_POINT('Ctrl Pts',(-1.92453321512437,-42.9740309956624,
0.));
#22349=CARTESIAN_POINT('Ctrl Pts',(-1.8783920201461,-43.065871623255,0.));
#22350=CARTESIAN_POINT('Ctrl Pts',(-1.83174385734712,-43.1576038253643,
0.));
#22351=CARTESIAN_POINT('Ctrl Pts',(-1.78459244842771,-43.2492259505872,
0.));
#22352=CARTESIAN_POINT('Ctrl Pts',(-1.73694151741125,-43.3407363140236,
0.));
#22353=CARTESIAN_POINT('Ctrl Pts',(-1.68879465270609,-43.4321333178711,
0.));
#22354=CARTESIAN_POINT('Ctrl Pts',(-1.64015515906649,-43.5234155788248,
0.));
#22355=CARTESIAN_POINT('Ctrl Pts',(-1.59102591108105,-43.6145820637333,
0.));
#22356=CARTESIAN_POINT('Ctrl Pts',(-1.53148589036097,-43.7238422193529,
0.));
#22357=CARTESIAN_POINT('Ctrl Pts',(-1.48126213998561,-43.8147465842503,
0.));
#22358=CARTESIAN_POINT('Ctrl Pts',(-1.44069595482724,-43.8873767449247,
0.));
#22359=CARTESIAN_POINT('Ctrl Pts',(-1.41005374202874,-43.9417969186811,
0.));
#22360=CARTESIAN_POINT('Ctrl Pts',(-1.38952890043917,-43.9780537249529,
0.));
#22361=CARTESIAN_POINT('Ctrl Pts',(-3.50724370857673,-37.4237196983922,
15.));
#22362=CARTESIAN_POINT('Ctrl Pts',(-3.50901346997657,-37.4426037737699,
15.));
#22363=CARTESIAN_POINT('Ctrl Pts',(-3.51204731876362,-37.4803889700239,
15.));
#22364=CARTESIAN_POINT('Ctrl Pts',(-3.51508109065211,-37.5371179004295,
15.));
#22365=CARTESIAN_POINT('Ctrl Pts',(-3.51624243734646,-37.6128545966533,
15.));
#22366=CARTESIAN_POINT('Ctrl Pts',(-3.51375922979958,-37.7076643105286,
15.));
#22367=CARTESIAN_POINT('Ctrl Pts',(-3.50844720825129,-37.8025803811856,
15.));
#22368=CARTESIAN_POINT('Ctrl Pts',(-3.50139628556084,-37.8975688353863,
15.));
#22369=CARTESIAN_POINT('Ctrl Pts',(-3.49340804454646,-37.9926009950482,
15.));
#22370=CARTESIAN_POINT('Ctrl Pts',(-3.48478279878234,-38.0876589224537,
15.));
#22371=CARTESIAN_POINT('Ctrl Pts',(-3.47549027265412,-38.1827321816559,
15.));
#22372=CARTESIAN_POINT('Ctrl Pts',(-3.46530185256873,-38.2778154909527,
15.));
#22373=CARTESIAN_POINT('Ctrl Pts',(-3.45393053211023,-38.3729061502716,
15.));
#22374=CARTESIAN_POINT('Ctrl Pts',(-3.44118343200304,-38.4680013094732,
15.));
#22375=CARTESIAN_POINT('Ctrl Pts',(-3.42705871084998,-38.5630961226878,
15.));
#22376=CARTESIAN_POINT('Ctrl Pts',(-3.41166717511902,-38.6581847668347,
15.));
#22377=CARTESIAN_POINT('Ctrl Pts',(-3.39518333281819,-38.7532609709905,
15.));
#22378=CARTESIAN_POINT('Ctrl Pts',(-3.37778863054483,-38.8483186930884,
15.));
#22379=CARTESIAN_POINT('Ctrl Pts',(-3.35960922799482,-38.9433528420174,
15.));
#22380=CARTESIAN_POINT('Ctrl Pts',(-3.34068601264473,-39.0383596151636,
15.));
#22381=CARTESIAN_POINT('Ctrl Pts',(-3.32100933979558,-39.1333360409949,
15.));
#22382=CARTESIAN_POINT('Ctrl Pts',(-3.30054018081688,-39.2282796893977,
15.));
#22383=CARTESIAN_POINT('Ctrl Pts',(-3.27923485388118,-39.3231883392913,
15.));
#22384=CARTESIAN_POINT('Ctrl Pts',(-3.25707264313389,-39.4180596080755,
15.));
#22385=CARTESIAN_POINT('Ctrl Pts',(-3.23406609691662,-39.5128908052622,
15.));
#22386=CARTESIAN_POINT('Ctrl Pts',(-3.21024640045596,-39.607679107639,15.));
#22387=CARTESIAN_POINT('Ctrl Pts',(-3.18565465503836,-39.7024216585552,
15.));
#22388=CARTESIAN_POINT('Ctrl Pts',(-3.16033160752805,-39.7971156880138,
15.));
#22389=CARTESIAN_POINT('Ctrl Pts',(-3.13430604330357,-39.8917586491576,
15.));
#22390=CARTESIAN_POINT('Ctrl Pts',(-3.10759149802909,-39.9863482523153,
15.));
#22391=CARTESIAN_POINT('Ctrl Pts',(-3.08019251155016,-40.0808823811787,
15.));
#22392=CARTESIAN_POINT('Ctrl Pts',(-3.05210847423072,-40.1753590391515,
15.));
#22393=CARTESIAN_POINT('Ctrl Pts',(-3.02333808901596,-40.2697762886113,
15.));
#22394=CARTESIAN_POINT('Ctrl Pts',(-2.9938844645822,-40.3641321823444,15.));
#22395=CARTESIAN_POINT('Ctrl Pts',(-2.96375636417323,-40.4584247445196,
15.));
#22396=CARTESIAN_POINT('Ctrl Pts',(-2.93296560822894,-40.5526520010651,
15.));
#22397=CARTESIAN_POINT('Ctrl Pts',(-2.90152548734344,-40.6468119976928,
15.));
#22398=CARTESIAN_POINT('Ctrl Pts',(-2.86944892209898,-40.7409028213129,
15.));
#22399=CARTESIAN_POINT('Ctrl Pts',(-2.8367463594668,-40.8349226258683,15.));
#22400=CARTESIAN_POINT('Ctrl Pts',(-2.80342531768406,-40.9288696352159,
15.));
#22401=CARTESIAN_POINT('Ctrl Pts',(-2.76949151194864,-41.0227421242398,
15.));
#22402=CARTESIAN_POINT('Ctrl Pts',(-2.73494956725006,-41.1165384061145,
15.));
#22403=CARTESIAN_POINT('Ctrl Pts',(-2.69980383625016,-41.2102568187956,
15.));
#22404=CARTESIAN_POINT('Ctrl Pts',(-2.66405934050119,-41.3038957096306,
15.));
#22405=CARTESIAN_POINT('Ctrl Pts',(-2.62772200460657,-41.3974534325936,
15.));
#22406=CARTESIAN_POINT('Ctrl Pts',(-2.59079818040173,-41.4909283577703,
15.));
#22407=CARTESIAN_POINT('Ctrl Pts',(-2.55329436064185,-41.5843188786284,
15.));
#22408=CARTESIAN_POINT('Ctrl Pts',(-2.51521684674478,-41.6776234194583,
15.));
#22409=CARTESIAN_POINT('Ctrl Pts',(-2.47657137427694,-41.7708404467533,
15.));
#22410=CARTESIAN_POINT('Ctrl Pts',(-2.43736301434201,-41.8639684667923,
15.));
#22411=CARTESIAN_POINT('Ctrl Pts',(-2.39759639399649,-41.9570060084039,
15.));
#22412=CARTESIAN_POINT('Ctrl Pts',(-2.3572758406643,-42.0499516093661,15.));
#22413=CARTESIAN_POINT('Ctrl Pts',(-2.3164055474281,-42.1428038039937,15.));
#22414=CARTESIAN_POINT('Ctrl Pts',(-2.27498976664775,-42.2355611060784,
15.));
#22415=CARTESIAN_POINT('Ctrl Pts',(-2.23303287465501,-42.3282220118033,
15.));
#22416=CARTESIAN_POINT('Ctrl Pts',(-2.19053924976738,-42.4207850290047,
15.));
#22417=CARTESIAN_POINT('Ctrl Pts',(-2.14751319676746,-42.5132487024335,
15.));
#22418=CARTESIAN_POINT('Ctrl Pts',(-2.10395886401772,-42.6056116373455,
15.));
#22419=CARTESIAN_POINT('Ctrl Pts',(-2.0598801492452,-42.6978725343209,15.));
#22420=CARTESIAN_POINT('Ctrl Pts',(-2.0152806752809,-42.7900301875309,15.));
#22421=CARTESIAN_POINT('Ctrl Pts',(-1.97016390194217,-42.8820834139973,
15.));
#22422=CARTESIAN_POINT('Ctrl Pts',(-1.92453321512437,-42.9740309956624,
15.));
#22423=CARTESIAN_POINT('Ctrl Pts',(-1.8783920201461,-43.065871623255,15.));
#22424=CARTESIAN_POINT('Ctrl Pts',(-1.83174385734712,-43.1576038253643,
15.));
#22425=CARTESIAN_POINT('Ctrl Pts',(-1.78459244842771,-43.2492259505872,
15.));
#22426=CARTESIAN_POINT('Ctrl Pts',(-1.73694151741125,-43.3407363140236,
15.));
#22427=CARTESIAN_POINT('Ctrl Pts',(-1.68879465270609,-43.4321333178711,
15.));
#22428=CARTESIAN_POINT('Ctrl Pts',(-1.64015515906649,-43.5234155788248,
15.));
#22429=CARTESIAN_POINT('Ctrl Pts',(-1.59102591108105,-43.6145820637333,
15.));
#22430=CARTESIAN_POINT('Ctrl Pts',(-1.53148589036097,-43.7238422193529,
15.));
#22431=CARTESIAN_POINT('Ctrl Pts',(-1.48126213998561,-43.8147465842503,
15.));
#22432=CARTESIAN_POINT('Ctrl Pts',(-1.44069595482724,-43.8873767449247,
15.));
#22433=CARTESIAN_POINT('Ctrl Pts',(-1.41005374202874,-43.9417969186811,
15.));
#22434=CARTESIAN_POINT('Ctrl Pts',(-1.38952890043917,-43.9780537249529,
15.));
#22435=CARTESIAN_POINT('Ctrl Pts',(-12.2684454652018,-42.2550026135057,
0.));
#22436=CARTESIAN_POINT('Ctrl Pts',(-12.2684454652018,-42.2550026135057,
18.));
#22437=CARTESIAN_POINT('Ctrl Pts',(-12.2530833383985,-42.2409327400055,
0.));
#22438=CARTESIAN_POINT('Ctrl Pts',(-12.2530833383985,-42.2409327400055,
18.));
#22439=CARTESIAN_POINT('Ctrl Pts',(-12.222401466668,-42.2127669677092,0.));
#22440=CARTESIAN_POINT('Ctrl Pts',(-12.222401466668,-42.2127669677092,18.));
#22441=CARTESIAN_POINT('Ctrl Pts',(-12.1765058047069,-42.1704402333854,
0.));
#22442=CARTESIAN_POINT('Ctrl Pts',(-12.1765058047069,-42.1704402333854,
18.));
#22443=CARTESIAN_POINT('Ctrl Pts',(-12.1155659644537,-42.1138483839101,
0.));
#22444=CARTESIAN_POINT('Ctrl Pts',(-12.1155659644537,-42.1138483839101,
18.));
#22445=CARTESIAN_POINT('Ctrl Pts',(-12.0398158079102,-42.0428479428228,
0.));
#22446=CARTESIAN_POINT('Ctrl Pts',(-12.0398158079102,-42.0428479428228,
18.));
#22447=CARTESIAN_POINT('Ctrl Pts',(-11.9644914999263,-41.9715865222182,
0.));
#22448=CARTESIAN_POINT('Ctrl Pts',(-11.9644914999263,-41.9715865222182,
18.));
#22449=CARTESIAN_POINT('Ctrl Pts',(-11.8895948153349,-41.9000638152266,
0.));
#22450=CARTESIAN_POINT('Ctrl Pts',(-11.8895948153349,-41.9000638152266,
18.));
#22451=CARTESIAN_POINT('Ctrl Pts',(-11.81512813804,-41.8282796562569,0.));
#22452=CARTESIAN_POINT('Ctrl Pts',(-11.81512813804,-41.8282796562569,18.));
#22453=CARTESIAN_POINT('Ctrl Pts',(-11.7410945211992,-41.7562341395977,
0.));
#22454=CARTESIAN_POINT('Ctrl Pts',(-11.7410945211992,-41.7562341395977,
18.));
#22455=CARTESIAN_POINT('Ctrl Pts',(-11.6674975352852,-41.6839275596248,
0.));
#22456=CARTESIAN_POINT('Ctrl Pts',(-11.6674975352852,-41.6839275596248,
18.));
#22457=CARTESIAN_POINT('Ctrl Pts',(-11.5943410868252,-41.6113603270596,
0.));
#22458=CARTESIAN_POINT('Ctrl Pts',(-11.5943410868252,-41.6113603270596,
18.));
#22459=CARTESIAN_POINT('Ctrl Pts',(-11.5216292382388,-41.5385328935506,
0.));
#22460=CARTESIAN_POINT('Ctrl Pts',(-11.5216292382388,-41.5385328935506,
18.));
#22461=CARTESIAN_POINT('Ctrl Pts',(-11.449366039385,-41.4654456796071,0.));
#22462=CARTESIAN_POINT('Ctrl Pts',(-11.449366039385,-41.4654456796071,18.));
#22463=CARTESIAN_POINT('Ctrl Pts',(-11.3775553120177,-41.3920989905986,
0.));
#22464=CARTESIAN_POINT('Ctrl Pts',(-11.3775553120177,-41.3920989905986,
18.));
#22465=CARTESIAN_POINT('Ctrl Pts',(-11.3062006993745,-41.3184930194148,
0.));
#22466=CARTESIAN_POINT('Ctrl Pts',(-11.3062006993745,-41.3184930194148,
18.));
#22467=CARTESIAN_POINT('Ctrl Pts',(-11.2353057980338,-41.2446278781981,
0.));
#22468=CARTESIAN_POINT('Ctrl Pts',(-11.2353057980338,-41.2446278781981,
18.));
#22469=CARTESIAN_POINT('Ctrl Pts',(-11.1648742640378,-41.1705036228854,
0.));
#22470=CARTESIAN_POINT('Ctrl Pts',(-11.1648742640378,-41.1705036228854,
18.));
#22471=CARTESIAN_POINT('Ctrl Pts',(-11.0949099155251,-41.0961202807715,
0.));
#22472=CARTESIAN_POINT('Ctrl Pts',(-11.0949099155251,-41.0961202807715,
18.));
#22473=CARTESIAN_POINT('Ctrl Pts',(-11.0254168609972,-41.0214778832142,
0.));
#22474=CARTESIAN_POINT('Ctrl Pts',(-11.0254168609972,-41.0214778832142,
18.));
#22475=CARTESIAN_POINT('Ctrl Pts',(-10.956399476781,-40.9465764747798,0.));
#22476=CARTESIAN_POINT('Ctrl Pts',(-10.956399476781,-40.9465764747798,18.));
#22477=CARTESIAN_POINT('Ctrl Pts',(-10.8878623066647,-40.8714161092412,
0.));
#22478=CARTESIAN_POINT('Ctrl Pts',(-10.8878623066647,-40.8714161092412,
18.));
#22479=CARTESIAN_POINT('Ctrl Pts',(-10.8198099757795,-40.7959968527561,
0.));
#22480=CARTESIAN_POINT('Ctrl Pts',(-10.8198099757795,-40.7959968527561,
18.));
#22481=CARTESIAN_POINT('Ctrl Pts',(-10.7522471109694,-40.7203187831783,
0.));
#22482=CARTESIAN_POINT('Ctrl Pts',(-10.7522471109694,-40.7203187831783,
18.));
#22483=CARTESIAN_POINT('Ctrl Pts',(-10.6851782157325,-40.6443819999244,
0.));
#22484=CARTESIAN_POINT('Ctrl Pts',(-10.6851782157325,-40.6443819999244,
18.));
#22485=CARTESIAN_POINT('Ctrl Pts',(-10.618607730849,-40.5681866012103,0.));
#22486=CARTESIAN_POINT('Ctrl Pts',(-10.618607730849,-40.5681866012103,18.));
#22487=CARTESIAN_POINT('Ctrl Pts',(-10.5525402237951,-40.4917326404439,
0.));
#22488=CARTESIAN_POINT('Ctrl Pts',(-10.5525402237951,-40.4917326404439,
18.));
#22489=CARTESIAN_POINT('Ctrl Pts',(-10.48698054978,-40.4150200869536,0.));
#22490=CARTESIAN_POINT('Ctrl Pts',(-10.48698054978,-40.4150200869536,18.));
#22491=CARTESIAN_POINT('Ctrl Pts',(-10.4219339932951,-40.3380487942952,
0.));
#22492=CARTESIAN_POINT('Ctrl Pts',(-10.4219339932951,-40.3380487942952,
18.));
#22493=CARTESIAN_POINT('Ctrl Pts',(-10.3574064830678,-40.2608184485326,
0.));
#22494=CARTESIAN_POINT('Ctrl Pts',(-10.3574064830678,-40.2608184485326,
18.));
#22495=CARTESIAN_POINT('Ctrl Pts',(-10.2934044990237,-40.1833286010098,
0.));
#22496=CARTESIAN_POINT('Ctrl Pts',(-10.2934044990237,-40.1833286010098,
18.));
#22497=CARTESIAN_POINT('Ctrl Pts',(-10.2299347125857,-40.1055787732578,
0.));
#22498=CARTESIAN_POINT('Ctrl Pts',(-10.2299347125857,-40.1055787732578,
18.));
#22499=CARTESIAN_POINT('Ctrl Pts',(-10.1670036683795,-40.0275685525923,
0.));
#22500=CARTESIAN_POINT('Ctrl Pts',(-10.1670036683795,-40.0275685525923,
18.));
#22501=CARTESIAN_POINT('Ctrl Pts',(-10.1046175096878,-39.9492976736738,
0.));
#22502=CARTESIAN_POINT('Ctrl Pts',(-10.1046175096878,-39.9492976736738,
18.));
#22503=CARTESIAN_POINT('Ctrl Pts',(-10.0427815229883,-39.8707661565233,
0.));
#22504=CARTESIAN_POINT('Ctrl Pts',(-10.0427815229883,-39.8707661565233,
18.));
#22505=CARTESIAN_POINT('Ctrl Pts',(-9.98150036150824,-39.7919742367922,
0.));
#22506=CARTESIAN_POINT('Ctrl Pts',(-9.98150036150824,-39.7919742367922,
18.));
#22507=CARTESIAN_POINT('Ctrl Pts',(-9.92077894513193,-39.712922089547,0.));
#22508=CARTESIAN_POINT('Ctrl Pts',(-9.92077894513193,-39.712922089547,18.));
#22509=CARTESIAN_POINT('Ctrl Pts',(-9.86062324242561,-39.6336095893767,
0.));
#22510=CARTESIAN_POINT('Ctrl Pts',(-9.86062324242561,-39.6336095893767,
18.));
#22511=CARTESIAN_POINT('Ctrl Pts',(-9.80104095251614,-39.5540361022309,
0.));
#22512=CARTESIAN_POINT('Ctrl Pts',(-9.80104095251614,-39.5540361022309,
18.));
#22513=CARTESIAN_POINT('Ctrl Pts',(-9.74204258152664,-39.4742001555227,
0.));
#22514=CARTESIAN_POINT('Ctrl Pts',(-9.74204258152664,-39.4742001555227,
18.));
#22515=CARTESIAN_POINT('Ctrl Pts',(-9.68364100883828,-39.3940995760289,
0.));
#22516=CARTESIAN_POINT('Ctrl Pts',(-9.68364100883828,-39.3940995760289,
18.));
#22517=CARTESIAN_POINT('Ctrl Pts',(-9.62584947846544,-39.3137321153686,
0.));
#22518=CARTESIAN_POINT('Ctrl Pts',(-9.62584947846544,-39.3137321153686,
18.));
#22519=CARTESIAN_POINT('Ctrl Pts',(-9.56867984233624,-39.2330959982788,
0.));
#22520=CARTESIAN_POINT('Ctrl Pts',(-9.56867984233624,-39.2330959982788,
18.));
#22521=CARTESIAN_POINT('Ctrl Pts',(-9.51214104535621,-39.1521903958955,
0.));
#22522=CARTESIAN_POINT('Ctrl Pts',(-9.51214104535621,-39.1521903958955,
18.));
#22523=CARTESIAN_POINT('Ctrl Pts',(-9.45623664577432,-39.0710161994951,
0.));
#22524=CARTESIAN_POINT('Ctrl Pts',(-9.45623664577432,-39.0710161994951,
18.));
#22525=CARTESIAN_POINT('Ctrl Pts',(-9.40096600877644,-38.9895756526779,
0.));
#22526=CARTESIAN_POINT('Ctrl Pts',(-9.40096600877644,-38.9895756526779,
18.));
#22527=CARTESIAN_POINT('Ctrl Pts',(-9.34632917154637,-38.9078708427078,
0.));
#22528=CARTESIAN_POINT('Ctrl Pts',(-9.34632917154637,-38.9078708427078,
18.));
#22529=CARTESIAN_POINT('Ctrl Pts',(-9.29233110570904,-38.8259023794241,
0.));
#22530=CARTESIAN_POINT('Ctrl Pts',(-9.29233110570904,-38.8259023794241,
18.));
#22531=CARTESIAN_POINT('Ctrl Pts',(-9.23898539199332,-38.7436682576832,
0.));
#22532=CARTESIAN_POINT('Ctrl Pts',(-9.23898539199332,-38.7436682576832,
18.));
#22533=CARTESIAN_POINT('Ctrl Pts',(-9.1863201939433,-38.6611620045193,0.));
#22534=CARTESIAN_POINT('Ctrl Pts',(-9.1863201939433,-38.6611620045193,18.));
#22535=CARTESIAN_POINT('Ctrl Pts',(-9.13437512010587,-38.5783736628826,
0.));
#22536=CARTESIAN_POINT('Ctrl Pts',(-9.13437512010587,-38.5783736628826,
18.));
#22537=CARTESIAN_POINT('Ctrl Pts',(-9.08319014288087,-38.4952932486131,
0.));
#22538=CARTESIAN_POINT('Ctrl Pts',(-9.08319014288087,-38.4952932486131,
18.));
#22539=CARTESIAN_POINT('Ctrl Pts',(-9.03279579360191,-38.4119138099805,
0.));
#22540=CARTESIAN_POINT('Ctrl Pts',(-9.03279579360191,-38.4119138099805,
18.));
#22541=CARTESIAN_POINT('Ctrl Pts',(-8.98320483785761,-38.3282340281403,
0.));
#22542=CARTESIAN_POINT('Ctrl Pts',(-8.98320483785761,-38.3282340281403,
18.));
#22543=CARTESIAN_POINT('Ctrl Pts',(-8.9343983099634,-38.2442625706309,0.));
#22544=CARTESIAN_POINT('Ctrl Pts',(-8.9343983099634,-38.2442625706309,18.));
#22545=CARTESIAN_POINT('Ctrl Pts',(-8.88633535238435,-38.1600150482528,
0.));
#22546=CARTESIAN_POINT('Ctrl Pts',(-8.88633535238435,-38.1600150482528,
18.));
#22547=CARTESIAN_POINT('Ctrl Pts',(-8.8389795976335,-38.0755058326913,0.));
#22548=CARTESIAN_POINT('Ctrl Pts',(-8.8389795976335,-38.0755058326913,18.));
#22549=CARTESIAN_POINT('Ctrl Pts',(-8.79232279131093,-37.9907407304174,
0.));
#22550=CARTESIAN_POINT('Ctrl Pts',(-8.79232279131093,-37.9907407304174,
18.));
#22551=CARTESIAN_POINT('Ctrl Pts',(-8.74640499479003,-37.9057107230066,
0.));
#22552=CARTESIAN_POINT('Ctrl Pts',(-8.74640499479003,-37.9057107230066,
18.));
#22553=CARTESIAN_POINT('Ctrl Pts',(-8.70134776631144,-37.8203816669031,
0.));
#22554=CARTESIAN_POINT('Ctrl Pts',(-8.70134776631144,-37.8203816669031,
18.));
#22555=CARTESIAN_POINT('Ctrl Pts',(-8.65732553894525,-37.7347032383719,
0.));
#22556=CARTESIAN_POINT('Ctrl Pts',(-8.65732553894525,-37.7347032383719,
18.));
#22557=CARTESIAN_POINT('Ctrl Pts',(-8.61450621749156,-37.6486274754754,
0.));
#22558=CARTESIAN_POINT('Ctrl Pts',(-8.61450621749156,-37.6486274754754,
18.));
#22559=CARTESIAN_POINT('Ctrl Pts',(-8.57299698459467,-37.5621256752108,
0.));
#22560=CARTESIAN_POINT('Ctrl Pts',(-8.57299698459467,-37.5621256752108,
18.));
#22561=CARTESIAN_POINT('Ctrl Pts',(-8.53279758643785,-37.4752030152968,
0.));
#22562=CARTESIAN_POINT('Ctrl Pts',(-8.53279758643785,-37.4752030152968,
18.));
#22563=CARTESIAN_POINT('Ctrl Pts',(-8.49372546467076,-37.3879218093514,
0.));
#22564=CARTESIAN_POINT('Ctrl Pts',(-8.49372546467076,-37.3879218093514,
18.));
#22565=CARTESIAN_POINT('Ctrl Pts',(-8.45550849433961,-37.3003733151561,
0.));
#22566=CARTESIAN_POINT('Ctrl Pts',(-8.45550849433961,-37.3003733151561,
18.));
#22567=CARTESIAN_POINT('Ctrl Pts',(-8.41793088313261,-37.2126332013933,
0.));
#22568=CARTESIAN_POINT('Ctrl Pts',(-8.41793088313261,-37.2126332013933,
18.));
#22569=CARTESIAN_POINT('Ctrl Pts',(-8.38096706211449,-37.1247207489179,
0.));
#22570=CARTESIAN_POINT('Ctrl Pts',(-8.38096706211449,-37.1247207489179,
18.));
#22571=CARTESIAN_POINT('Ctrl Pts',(-8.3449081895264,-37.0365602155148,0.));
#22572=CARTESIAN_POINT('Ctrl Pts',(-8.3449081895264,-37.0365602155148,18.));
#22573=CARTESIAN_POINT('Ctrl Pts',(-8.31052547794592,-36.9479311729484,
0.));
#22574=CARTESIAN_POINT('Ctrl Pts',(-8.31052547794592,-36.9479311729484,
18.));
#22575=CARTESIAN_POINT('Ctrl Pts',(-8.27886599440786,-36.8585291300917,
0.));
#22576=CARTESIAN_POINT('Ctrl Pts',(-8.27886599440786,-36.8585291300917,
18.));
#22577=CARTESIAN_POINT('Ctrl Pts',(-8.25656657451821,-36.7861403757604,
0.));
#22578=CARTESIAN_POINT('Ctrl Pts',(-8.25656657451821,-36.7861403757604,
18.));
#22579=CARTESIAN_POINT('Ctrl Pts',(-8.24192165947368,-36.7312504697652,
0.));
#22580=CARTESIAN_POINT('Ctrl Pts',(-8.24192165947368,-36.7312504697652,
18.));
#22581=CARTESIAN_POINT('Ctrl Pts',(-8.23313075335377,-36.6943771018148,
0.));
#22582=CARTESIAN_POINT('Ctrl Pts',(-8.23313075335377,-36.6943771018148,
18.));
#22583=CARTESIAN_POINT('Ctrl Pts',(-8.22897839625062,-36.6758703925241,
0.));
#22584=CARTESIAN_POINT('Ctrl Pts',(-8.22897839625062,-36.6758703925241,
18.));
#22585=CARTESIAN_POINT('',(-12.2684454652017,-42.2550026135057,0.));
#22586=CARTESIAN_POINT('Ctrl Pts',(-8.22897839625062,-36.6758703925241,
0.));
#22587=CARTESIAN_POINT('Ctrl Pts',(-8.23313075335377,-36.6943771018148,
0.));
#22588=CARTESIAN_POINT('Ctrl Pts',(-8.24192165947368,-36.7312504697652,
0.));
#22589=CARTESIAN_POINT('Ctrl Pts',(-8.25656657451821,-36.7861403757604,
0.));
#22590=CARTESIAN_POINT('Ctrl Pts',(-8.27886599440786,-36.8585291300917,
0.));
#22591=CARTESIAN_POINT('Ctrl Pts',(-8.31052547794592,-36.9479311729484,
0.));
#22592=CARTESIAN_POINT('Ctrl Pts',(-8.3449081895264,-37.0365602155148,0.));
#22593=CARTESIAN_POINT('Ctrl Pts',(-8.38096706211449,-37.1247207489179,
0.));
#22594=CARTESIAN_POINT('Ctrl Pts',(-8.41793088313261,-37.2126332013933,
0.));
#22595=CARTESIAN_POINT('Ctrl Pts',(-8.45550849433961,-37.3003733151561,
0.));
#22596=CARTESIAN_POINT('Ctrl Pts',(-8.49372546467076,-37.3879218093514,
0.));
#22597=CARTESIAN_POINT('Ctrl Pts',(-8.53279758643785,-37.4752030152968,
0.));
#22598=CARTESIAN_POINT('Ctrl Pts',(-8.57299698459467,-37.5621256752108,
0.));
#22599=CARTESIAN_POINT('Ctrl Pts',(-8.61450621749156,-37.6486274754754,
0.));
#22600=CARTESIAN_POINT('Ctrl Pts',(-8.65732553894525,-37.7347032383719,
0.));
#22601=CARTESIAN_POINT('Ctrl Pts',(-8.70134776631144,-37.8203816669031,
0.));
#22602=CARTESIAN_POINT('Ctrl Pts',(-8.74640499479003,-37.9057107230066,
0.));
#22603=CARTESIAN_POINT('Ctrl Pts',(-8.79232279131093,-37.9907407304174,
0.));
#22604=CARTESIAN_POINT('Ctrl Pts',(-8.8389795976335,-38.0755058326913,0.));
#22605=CARTESIAN_POINT('Ctrl Pts',(-8.88633535238435,-38.1600150482528,
0.));
#22606=CARTESIAN_POINT('Ctrl Pts',(-8.9343983099634,-38.2442625706309,0.));
#22607=CARTESIAN_POINT('Ctrl Pts',(-8.98320483785761,-38.3282340281403,
0.));
#22608=CARTESIAN_POINT('Ctrl Pts',(-9.03279579360191,-38.4119138099805,
0.));
#22609=CARTESIAN_POINT('Ctrl Pts',(-9.08319014288087,-38.4952932486131,
0.));
#22610=CARTESIAN_POINT('Ctrl Pts',(-9.13437512010587,-38.5783736628826,
0.));
#22611=CARTESIAN_POINT('Ctrl Pts',(-9.1863201939433,-38.6611620045193,0.));
#22612=CARTESIAN_POINT('Ctrl Pts',(-9.23898539199332,-38.7436682576832,
0.));
#22613=CARTESIAN_POINT('Ctrl Pts',(-9.29233110570904,-38.8259023794241,
0.));
#22614=CARTESIAN_POINT('Ctrl Pts',(-9.34632917154637,-38.9078708427078,
0.));
#22615=CARTESIAN_POINT('Ctrl Pts',(-9.40096600877644,-38.9895756526779,
0.));
#22616=CARTESIAN_POINT('Ctrl Pts',(-9.45623664577432,-39.0710161994951,
0.));
#22617=CARTESIAN_POINT('Ctrl Pts',(-9.51214104535621,-39.1521903958955,
0.));
#22618=CARTESIAN_POINT('Ctrl Pts',(-9.56867984233624,-39.2330959982788,
0.));
#22619=CARTESIAN_POINT('Ctrl Pts',(-9.62584947846544,-39.3137321153686,
0.));
#22620=CARTESIAN_POINT('Ctrl Pts',(-9.68364100883828,-39.3940995760289,
0.));
#22621=CARTESIAN_POINT('Ctrl Pts',(-9.74204258152664,-39.4742001555227,
0.));
#22622=CARTESIAN_POINT('Ctrl Pts',(-9.80104095251614,-39.5540361022309,
0.));
#22623=CARTESIAN_POINT('Ctrl Pts',(-9.86062324242561,-39.6336095893767,
0.));
#22624=CARTESIAN_POINT('Ctrl Pts',(-9.92077894513193,-39.712922089547,0.));
#22625=CARTESIAN_POINT('Ctrl Pts',(-9.98150036150824,-39.7919742367922,
0.));
#22626=CARTESIAN_POINT('Ctrl Pts',(-10.0427815229883,-39.8707661565233,
0.));
#22627=CARTESIAN_POINT('Ctrl Pts',(-10.1046175096878,-39.9492976736738,
0.));
#22628=CARTESIAN_POINT('Ctrl Pts',(-10.1670036683795,-40.0275685525923,
0.));
#22629=CARTESIAN_POINT('Ctrl Pts',(-10.2299347125857,-40.1055787732578,
0.));
#22630=CARTESIAN_POINT('Ctrl Pts',(-10.2934044990237,-40.1833286010098,
0.));
#22631=CARTESIAN_POINT('Ctrl Pts',(-10.3574064830678,-40.2608184485326,
0.));
#22632=CARTESIAN_POINT('Ctrl Pts',(-10.4219339932951,-40.3380487942952,
0.));
#22633=CARTESIAN_POINT('Ctrl Pts',(-10.48698054978,-40.4150200869536,0.));
#22634=CARTESIAN_POINT('Ctrl Pts',(-10.5525402237951,-40.4917326404439,
0.));
#22635=CARTESIAN_POINT('Ctrl Pts',(-10.618607730849,-40.5681866012103,0.));
#22636=CARTESIAN_POINT('Ctrl Pts',(-10.6851782157325,-40.6443819999244,
0.));
#22637=CARTESIAN_POINT('Ctrl Pts',(-10.7522471109694,-40.7203187831783,
0.));
#22638=CARTESIAN_POINT('Ctrl Pts',(-10.8198099757795,-40.7959968527561,
0.));
#22639=CARTESIAN_POINT('Ctrl Pts',(-10.8878623066647,-40.8714161092412,
0.));
#22640=CARTESIAN_POINT('Ctrl Pts',(-10.956399476781,-40.9465764747798,0.));
#22641=CARTESIAN_POINT('Ctrl Pts',(-11.0254168609972,-41.0214778832142,
0.));
#22642=CARTESIAN_POINT('Ctrl Pts',(-11.0949099155251,-41.0961202807715,
0.));
#22643=CARTESIAN_POINT('Ctrl Pts',(-11.1648742640378,-41.1705036228854,
0.));
#22644=CARTESIAN_POINT('Ctrl Pts',(-11.2353057980338,-41.2446278781981,
0.));
#22645=CARTESIAN_POINT('Ctrl Pts',(-11.3062006993745,-41.3184930194148,
0.));
#22646=CARTESIAN_POINT('Ctrl Pts',(-11.3775553120177,-41.3920989905986,
0.));
#22647=CARTESIAN_POINT('Ctrl Pts',(-11.449366039385,-41.4654456796071,0.));
#22648=CARTESIAN_POINT('Ctrl Pts',(-11.5216292382388,-41.5385328935506,
0.));
#22649=CARTESIAN_POINT('Ctrl Pts',(-11.5943410868252,-41.6113603270596,
0.));
#22650=CARTESIAN_POINT('Ctrl Pts',(-11.6674975352852,-41.6839275596248,
0.));
#22651=CARTESIAN_POINT('Ctrl Pts',(-11.7410945211992,-41.7562341395977,
0.));
#22652=CARTESIAN_POINT('Ctrl Pts',(-11.81512813804,-41.8282796562569,0.));
#22653=CARTESIAN_POINT('Ctrl Pts',(-11.8895948153349,-41.9000638152266,
0.));
#22654=CARTESIAN_POINT('Ctrl Pts',(-11.9644914999263,-41.9715865222182,
0.));
#22655=CARTESIAN_POINT('Ctrl Pts',(-12.054880669507,-42.0571002269437,0.));
#22656=CARTESIAN_POINT('Ctrl Pts',(-12.1307372881904,-42.1280354231517,
0.));
#22657=CARTESIAN_POINT('Ctrl Pts',(-12.1917619768791,-42.18457517013,0.));
#22658=CARTESIAN_POINT('Ctrl Pts',(-12.2377212115625,-42.2268628664988,
0.));
#22659=CARTESIAN_POINT('Ctrl Pts',(-12.2684454652018,-42.2550026135057,
0.));
#22660=CARTESIAN_POINT('',(-12.2684454652017,-42.2550026135057,15.));
#22661=CARTESIAN_POINT('Ctrl Pts',(-12.2684454652018,-42.2550026135057,
15.));
#22662=CARTESIAN_POINT('Ctrl Pts',(-12.2530833383985,-42.2409327400055,
15.));
#22663=CARTESIAN_POINT('Ctrl Pts',(-12.222401466668,-42.2127669677092,15.));
#22664=CARTESIAN_POINT('Ctrl Pts',(-12.1765058047069,-42.1704402333854,
15.));
#22665=CARTESIAN_POINT('Ctrl Pts',(-12.1155659644537,-42.1138483839101,
15.));
#22666=CARTESIAN_POINT('Ctrl Pts',(-12.0398158079102,-42.0428479428228,
15.));
#22667=CARTESIAN_POINT('Ctrl Pts',(-11.9644914999263,-41.9715865222182,
15.));
#22668=CARTESIAN_POINT('Ctrl Pts',(-11.8895948153349,-41.9000638152266,
15.));
#22669=CARTESIAN_POINT('Ctrl Pts',(-11.81512813804,-41.8282796562569,15.));
#22670=CARTESIAN_POINT('Ctrl Pts',(-11.7410945211992,-41.7562341395977,
15.));
#22671=CARTESIAN_POINT('Ctrl Pts',(-11.6674975352852,-41.6839275596248,
15.));
#22672=CARTESIAN_POINT('Ctrl Pts',(-11.5943410868252,-41.6113603270596,
15.));
#22673=CARTESIAN_POINT('Ctrl Pts',(-11.5216292382388,-41.5385328935506,
15.));
#22674=CARTESIAN_POINT('Ctrl Pts',(-11.449366039385,-41.4654456796071,15.));
#22675=CARTESIAN_POINT('Ctrl Pts',(-11.3775553120177,-41.3920989905986,
15.));
#22676=CARTESIAN_POINT('Ctrl Pts',(-11.3062006993745,-41.3184930194148,
15.));
#22677=CARTESIAN_POINT('Ctrl Pts',(-11.2353057980338,-41.2446278781981,
15.));
#22678=CARTESIAN_POINT('Ctrl Pts',(-11.1648742640378,-41.1705036228854,
15.));
#22679=CARTESIAN_POINT('Ctrl Pts',(-11.0949099155251,-41.0961202807715,
15.));
#22680=CARTESIAN_POINT('Ctrl Pts',(-11.0254168609972,-41.0214778832142,
15.));
#22681=CARTESIAN_POINT('Ctrl Pts',(-10.956399476781,-40.9465764747798,15.));
#22682=CARTESIAN_POINT('Ctrl Pts',(-10.8878623066647,-40.8714161092412,
15.));
#22683=CARTESIAN_POINT('Ctrl Pts',(-10.8198099757795,-40.7959968527561,
15.));
#22684=CARTESIAN_POINT('Ctrl Pts',(-10.7522471109694,-40.7203187831783,
15.));
#22685=CARTESIAN_POINT('Ctrl Pts',(-10.6851782157325,-40.6443819999244,
15.));
#22686=CARTESIAN_POINT('Ctrl Pts',(-10.618607730849,-40.5681866012103,15.));
#22687=CARTESIAN_POINT('Ctrl Pts',(-10.5525402237951,-40.4917326404439,
15.));
#22688=CARTESIAN_POINT('Ctrl Pts',(-10.48698054978,-40.4150200869536,15.));
#22689=CARTESIAN_POINT('Ctrl Pts',(-10.4219339932951,-40.3380487942952,
15.));
#22690=CARTESIAN_POINT('Ctrl Pts',(-10.3574064830678,-40.2608184485326,
15.));
#22691=CARTESIAN_POINT('Ctrl Pts',(-10.2934044990237,-40.1833286010098,
15.));
#22692=CARTESIAN_POINT('Ctrl Pts',(-10.2299347125857,-40.1055787732578,
15.));
#22693=CARTESIAN_POINT('Ctrl Pts',(-10.1670036683795,-40.0275685525923,
15.));
#22694=CARTESIAN_POINT('Ctrl Pts',(-10.1046175096878,-39.9492976736738,
15.));
#22695=CARTESIAN_POINT('Ctrl Pts',(-10.0427815229883,-39.8707661565233,
15.));
#22696=CARTESIAN_POINT('Ctrl Pts',(-9.98150036150824,-39.7919742367922,
15.));
#22697=CARTESIAN_POINT('Ctrl Pts',(-9.92077894513193,-39.712922089547,15.));
#22698=CARTESIAN_POINT('Ctrl Pts',(-9.86062324242561,-39.6336095893767,
15.));
#22699=CARTESIAN_POINT('Ctrl Pts',(-9.80104095251614,-39.5540361022309,
15.));
#22700=CARTESIAN_POINT('Ctrl Pts',(-9.74204258152664,-39.4742001555227,
15.));
#22701=CARTESIAN_POINT('Ctrl Pts',(-9.68364100883828,-39.3940995760289,
15.));
#22702=CARTESIAN_POINT('Ctrl Pts',(-9.62584947846544,-39.3137321153686,
15.));
#22703=CARTESIAN_POINT('Ctrl Pts',(-9.56867984233624,-39.2330959982788,
15.));
#22704=CARTESIAN_POINT('Ctrl Pts',(-9.51214104535621,-39.1521903958955,
15.));
#22705=CARTESIAN_POINT('Ctrl Pts',(-9.45623664577432,-39.0710161994951,
15.));
#22706=CARTESIAN_POINT('Ctrl Pts',(-9.40096600877644,-38.9895756526779,
15.));
#22707=CARTESIAN_POINT('Ctrl Pts',(-9.34632917154637,-38.9078708427078,
15.));
#22708=CARTESIAN_POINT('Ctrl Pts',(-9.29233110570904,-38.8259023794241,
15.));
#22709=CARTESIAN_POINT('Ctrl Pts',(-9.23898539199332,-38.7436682576832,
15.));
#22710=CARTESIAN_POINT('Ctrl Pts',(-9.1863201939433,-38.6611620045193,15.));
#22711=CARTESIAN_POINT('Ctrl Pts',(-9.13437512010587,-38.5783736628826,
15.));
#22712=CARTESIAN_POINT('Ctrl Pts',(-9.08319014288087,-38.4952932486131,
15.));
#22713=CARTESIAN_POINT('Ctrl Pts',(-9.03279579360191,-38.4119138099805,
15.));
#22714=CARTESIAN_POINT('Ctrl Pts',(-8.98320483785761,-38.3282340281403,
15.));
#22715=CARTESIAN_POINT('Ctrl Pts',(-8.9343983099634,-38.2442625706309,15.));
#22716=CARTESIAN_POINT('Ctrl Pts',(-8.88633535238435,-38.1600150482528,
15.));
#22717=CARTESIAN_POINT('Ctrl Pts',(-8.8389795976335,-38.0755058326913,15.));
#22718=CARTESIAN_POINT('Ctrl Pts',(-8.79232279131093,-37.9907407304174,
15.));
#22719=CARTESIAN_POINT('Ctrl Pts',(-8.74640499479003,-37.9057107230066,
15.));
#22720=CARTESIAN_POINT('Ctrl Pts',(-8.70134776631144,-37.8203816669031,
15.));
#22721=CARTESIAN_POINT('Ctrl Pts',(-8.65732553894525,-37.7347032383719,
15.));
#22722=CARTESIAN_POINT('Ctrl Pts',(-8.61450621749156,-37.6486274754754,
15.));
#22723=CARTESIAN_POINT('Ctrl Pts',(-8.57299698459467,-37.5621256752108,
15.));
#22724=CARTESIAN_POINT('Ctrl Pts',(-8.53279758643785,-37.4752030152968,
15.));
#22725=CARTESIAN_POINT('Ctrl Pts',(-8.49372546467076,-37.3879218093514,
15.));
#22726=CARTESIAN_POINT('Ctrl Pts',(-8.45550849433961,-37.3003733151561,
15.));
#22727=CARTESIAN_POINT('Ctrl Pts',(-8.41793088313261,-37.2126332013933,
15.));
#22728=CARTESIAN_POINT('Ctrl Pts',(-8.38096706211449,-37.1247207489179,
15.));
#22729=CARTESIAN_POINT('Ctrl Pts',(-8.3449081895264,-37.0365602155148,15.));
#22730=CARTESIAN_POINT('Ctrl Pts',(-8.31052547794592,-36.9479311729484,
15.));
#22731=CARTESIAN_POINT('Ctrl Pts',(-8.27886599440786,-36.8585291300917,
15.));
#22732=CARTESIAN_POINT('Ctrl Pts',(-8.25656657451821,-36.7861403757604,
15.));
#22733=CARTESIAN_POINT('Ctrl Pts',(-8.24192165947368,-36.7312504697652,
15.));
#22734=CARTESIAN_POINT('Ctrl Pts',(-8.23313075335377,-36.6943771018148,
15.));
#22735=CARTESIAN_POINT('Ctrl Pts',(-8.22897839625062,-36.6758703925241,
15.));
#22736=CARTESIAN_POINT('',(-12.2684454652017,-42.2550026135057,0.));
#22737=CARTESIAN_POINT('Origin',(-3.50213800024364E-12,-1.07784724682657E-11,
0.));
#22738=CARTESIAN_POINT('',(-14.911486495888,-41.396226524684,0.));
#22739=CARTESIAN_POINT('Origin',(-3.50213800024364E-12,-1.07784724682657E-11,
0.));
#22740=CARTESIAN_POINT('',(-14.911486495888,-41.396226524684,15.));
#22741=CARTESIAN_POINT('Origin',(-3.50213800024364E-12,-1.07784724682657E-11,
15.));
#22742=CARTESIAN_POINT('',(-14.911486495888,-41.396226524684,0.));
#22743=CARTESIAN_POINT('Ctrl Pts',(-14.9001523628048,-34.5082745737944,
0.));
#22744=CARTESIAN_POINT('Ctrl Pts',(-14.9001523628048,-34.5082745737944,
18.));
#22745=CARTESIAN_POINT('Ctrl Pts',(-14.9076710061311,-34.525687510388,0.));
#22746=CARTESIAN_POINT('Ctrl Pts',(-14.9076710061311,-34.525687510388,18.));
#22747=CARTESIAN_POINT('Ctrl Pts',(-14.9222326355678,-34.5606858566713,
0.));
#22748=CARTESIAN_POINT('Ctrl Pts',(-14.9222326355678,-34.5606858566713,
18.));
#22749=CARTESIAN_POINT('Ctrl Pts',(-14.9426481276593,-34.6137007885254,
0.));
#22750=CARTESIAN_POINT('Ctrl Pts',(-14.9426481276593,-34.6137007885254,
18.));
#22751=CARTESIAN_POINT('Ctrl Pts',(-14.9671565602316,-34.6853717911268,
0.));
#22752=CARTESIAN_POINT('Ctrl Pts',(-14.9671565602316,-34.6853717911268,
18.));
#22753=CARTESIAN_POINT('Ctrl Pts',(-14.9940927023322,-34.7763085406486,
0.));
#22754=CARTESIAN_POINT('Ctrl Pts',(-14.9940927023322,-34.7763085406486,
18.));
#22755=CARTESIAN_POINT('Ctrl Pts',(-15.0183713484962,-34.8682205930809,
0.));
#22756=CARTESIAN_POINT('Ctrl Pts',(-15.0183713484962,-34.8682205930809,
18.));
#22757=CARTESIAN_POINT('Ctrl Pts',(-15.041018569143,-34.9607388363587,0.));
#22758=CARTESIAN_POINT('Ctrl Pts',(-15.041018569143,-34.9607388363587,18.));
#22759=CARTESIAN_POINT('Ctrl Pts',(-15.0627878528202,-35.0535882932913,
0.));
#22760=CARTESIAN_POINT('Ctrl Pts',(-15.0627878528202,-35.0535882932913,
18.));
#22761=CARTESIAN_POINT('Ctrl Pts',(-15.08395927165,-35.1466591020976,0.));
#22762=CARTESIAN_POINT('Ctrl Pts',(-15.08395927165,-35.1466591020976,18.));
#22763=CARTESIAN_POINT('Ctrl Pts',(-15.104500806927,-35.2399506932815,0.));
#22764=CARTESIAN_POINT('Ctrl Pts',(-15.104500806927,-35.2399506932815,18.));
#22765=CARTESIAN_POINT('Ctrl Pts',(-15.1241934020682,-35.3335286891314,
0.));
#22766=CARTESIAN_POINT('Ctrl Pts',(-15.1241934020682,-35.3335286891314,
18.));
#22767=CARTESIAN_POINT('Ctrl Pts',(-15.1427632633831,-35.4274792115856,
0.));
#22768=CARTESIAN_POINT('Ctrl Pts',(-15.1427632633831,-35.4274792115856,
18.));
#22769=CARTESIAN_POINT('Ctrl Pts',(-15.1600260710384,-35.5218591529745,
0.));
#22770=CARTESIAN_POINT('Ctrl Pts',(-15.1600260710384,-35.5218591529745,
18.));
#22771=CARTESIAN_POINT('Ctrl Pts',(-15.1759785763051,-35.6166644736253,
0.));
#22772=CARTESIAN_POINT('Ctrl Pts',(-15.1759785763051,-35.6166644736253,
18.));
#22773=CARTESIAN_POINT('Ctrl Pts',(-15.1907243629659,-35.7118553943773,
0.));
#22774=CARTESIAN_POINT('Ctrl Pts',(-15.1907243629659,-35.7118553943773,
18.));
#22775=CARTESIAN_POINT('Ctrl Pts',(-15.2044274601769,-35.8073720252878,
0.));
#22776=CARTESIAN_POINT('Ctrl Pts',(-15.2044274601769,-35.8073720252878,
18.));
#22777=CARTESIAN_POINT('Ctrl Pts',(-15.2172585668056,-35.9031525499277,
0.));
#22778=CARTESIAN_POINT('Ctrl Pts',(-15.2172585668056,-35.9031525499277,
18.));
#22779=CARTESIAN_POINT('Ctrl Pts',(-15.2293360946131,-35.9991531408727,
0.));
#22780=CARTESIAN_POINT('Ctrl Pts',(-15.2293360946131,-35.9991531408727,
18.));
#22781=CARTESIAN_POINT('Ctrl Pts',(-15.240697754828,-36.095357546697,0.));
#22782=CARTESIAN_POINT('Ctrl Pts',(-15.240697754828,-36.095357546697,18.));
#22783=CARTESIAN_POINT('Ctrl Pts',(-15.2513334565427,-36.1917659216814,
0.));
#22784=CARTESIAN_POINT('Ctrl Pts',(-15.2513334565427,-36.1917659216814,
18.));
#22785=CARTESIAN_POINT('Ctrl Pts',(-15.2612053303774,-36.2883880151607,
0.));
#22786=CARTESIAN_POINT('Ctrl Pts',(-15.2612053303774,-36.2883880151607,
18.));
#22787=CARTESIAN_POINT('Ctrl Pts',(-15.2702711460937,-36.3852352131887,
0.));
#22788=CARTESIAN_POINT('Ctrl Pts',(-15.2702711460937,-36.3852352131887,
18.));
#22789=CARTESIAN_POINT('Ctrl Pts',(-15.2785104654792,-36.4823116513289,
0.));
#22790=CARTESIAN_POINT('Ctrl Pts',(-15.2785104654792,-36.4823116513289,
18.));
#22791=CARTESIAN_POINT('Ctrl Pts',(-15.2859343913094,-36.5796108931244,
0.));
#22792=CARTESIAN_POINT('Ctrl Pts',(-15.2859343913094,-36.5796108931244,
18.));
#22793=CARTESIAN_POINT('Ctrl Pts',(-15.2925717100767,-36.6771206167755,
0.));
#22794=CARTESIAN_POINT('Ctrl Pts',(-15.2925717100767,-36.6771206167755,
18.));
#22795=CARTESIAN_POINT('Ctrl Pts',(-15.2984606286738,-36.7748254044502,
0.));
#22796=CARTESIAN_POINT('Ctrl Pts',(-15.2984606286738,-36.7748254044502,
18.));
#22797=CARTESIAN_POINT('Ctrl Pts',(-15.3036390436952,-36.8727100302512,
0.));
#22798=CARTESIAN_POINT('Ctrl Pts',(-15.3036390436952,-36.8727100302512,
18.));
#22799=CARTESIAN_POINT('Ctrl Pts',(-15.3081335446406,-36.970763176802,0.));
#22800=CARTESIAN_POINT('Ctrl Pts',(-15.3081335446406,-36.970763176802,18.));
#22801=CARTESIAN_POINT('Ctrl Pts',(-15.3119562971444,-37.0689784837457,
0.));
#22802=CARTESIAN_POINT('Ctrl Pts',(-15.3119562971444,-37.0689784837457,
18.));
#22803=CARTESIAN_POINT('Ctrl Pts',(-15.3151109648809,-37.1673525354641,
0.));
#22804=CARTESIAN_POINT('Ctrl Pts',(-15.3151109648809,-37.1673525354641,
18.));
#22805=CARTESIAN_POINT('Ctrl Pts',(-15.3175963510698,-37.2658836214694,
0.));
#22806=CARTESIAN_POINT('Ctrl Pts',(-15.3175963510698,-37.2658836214694,
18.));
#22807=CARTESIAN_POINT('Ctrl Pts',(-15.3194106233802,-37.3645702997848,
0.));
#22808=CARTESIAN_POINT('Ctrl Pts',(-15.3194106233802,-37.3645702997848,
18.));
#22809=CARTESIAN_POINT('Ctrl Pts',(-15.3205561366169,-37.4634097578665,
0.));
#22810=CARTESIAN_POINT('Ctrl Pts',(-15.3205561366169,-37.4634097578665,
18.));
#22811=CARTESIAN_POINT('Ctrl Pts',(-15.3210406145546,-37.562397408596,0.));
#22812=CARTESIAN_POINT('Ctrl Pts',(-15.3210406145546,-37.562397408596,18.));
#22813=CARTESIAN_POINT('Ctrl Pts',(-15.3208746890781,-37.6615277218027,
0.));
#22814=CARTESIAN_POINT('Ctrl Pts',(-15.3208746890781,-37.6615277218027,
18.));
#22815=CARTESIAN_POINT('Ctrl Pts',(-15.320070396385,-37.7607947318286,0.));
#22816=CARTESIAN_POINT('Ctrl Pts',(-15.320070396385,-37.7607947318286,18.));
#22817=CARTESIAN_POINT('Ctrl Pts',(-15.3186394335023,-37.8601926265378,
0.));
#22818=CARTESIAN_POINT('Ctrl Pts',(-15.3186394335023,-37.8601926265378,
18.));
#22819=CARTESIAN_POINT('Ctrl Pts',(-15.3165911656268,-37.959716421934,0.));
#22820=CARTESIAN_POINT('Ctrl Pts',(-15.3165911656268,-37.959716421934,18.));
#22821=CARTESIAN_POINT('Ctrl Pts',(-15.3139321941687,-38.0593621055415,
0.));
#22822=CARTESIAN_POINT('Ctrl Pts',(-15.3139321941687,-38.0593621055415,
18.));
#22823=CARTESIAN_POINT('Ctrl Pts',(-15.310667421514,-38.1591262705847,0.));
#22824=CARTESIAN_POINT('Ctrl Pts',(-15.310667421514,-38.1591262705847,18.));
#22825=CARTESIAN_POINT('Ctrl Pts',(-15.3068007250314,-38.2590058835965,
0.));
#22826=CARTESIAN_POINT('Ctrl Pts',(-15.3068007250314,-38.2590058835965,
18.));
#22827=CARTESIAN_POINT('Ctrl Pts',(-15.3023357307483,-38.3589980188324,
0.));
#22828=CARTESIAN_POINT('Ctrl Pts',(-15.3023357307483,-38.3589980188324,
18.));
#22829=CARTESIAN_POINT('Ctrl Pts',(-15.297276703747,-38.4590995527814,0.));
#22830=CARTESIAN_POINT('Ctrl Pts',(-15.297276703747,-38.4590995527814,18.));
#22831=CARTESIAN_POINT('Ctrl Pts',(-15.2916287700102,-38.5593070891769,
0.));
#22832=CARTESIAN_POINT('Ctrl Pts',(-15.2916287700102,-38.5593070891769,
18.));
#22833=CARTESIAN_POINT('Ctrl Pts',(-15.2853974668211,-38.659617115053,0.));
#22834=CARTESIAN_POINT('Ctrl Pts',(-15.2853974668211,-38.659617115053,18.));
#22835=CARTESIAN_POINT('Ctrl Pts',(-15.2785884727112,-38.7600260961351,
0.));
#22836=CARTESIAN_POINT('Ctrl Pts',(-15.2785884727112,-38.7600260961351,
18.));
#22837=CARTESIAN_POINT('Ctrl Pts',(-15.2712072937639,-38.860530586589,0.));
#22838=CARTESIAN_POINT('Ctrl Pts',(-15.2712072937639,-38.860530586589,18.));
#22839=CARTESIAN_POINT('Ctrl Pts',(-15.2632589109473,-38.9611273555758,
0.));
#22840=CARTESIAN_POINT('Ctrl Pts',(-15.2632589109473,-38.9611273555758,
18.));
#22841=CARTESIAN_POINT('Ctrl Pts',(-15.2547476855825,-39.061813415425,0.));
#22842=CARTESIAN_POINT('Ctrl Pts',(-15.2547476855825,-39.061813415425,18.));
#22843=CARTESIAN_POINT('Ctrl Pts',(-15.2456775636447,-39.1625859371304,
0.));
#22844=CARTESIAN_POINT('Ctrl Pts',(-15.2456775636447,-39.1625859371304,
18.));
#22845=CARTESIAN_POINT('Ctrl Pts',(-15.2360522089072,-39.2634421927888,
0.));
#22846=CARTESIAN_POINT('Ctrl Pts',(-15.2360522089072,-39.2634421927888,
18.));
#22847=CARTESIAN_POINT('Ctrl Pts',(-15.225875156307,-39.3643794927167,0.));
#22848=CARTESIAN_POINT('Ctrl Pts',(-15.225875156307,-39.3643794927167,18.));
#22849=CARTESIAN_POINT('Ctrl Pts',(-15.2151499908149,-39.4653951093947,
0.));
#22850=CARTESIAN_POINT('Ctrl Pts',(-15.2151499908149,-39.4653951093947,
18.));
#22851=CARTESIAN_POINT('Ctrl Pts',(-15.2038804098649,-39.5664862602472,
0.));
#22852=CARTESIAN_POINT('Ctrl Pts',(-15.2038804098649,-39.5664862602472,
18.));
#22853=CARTESIAN_POINT('Ctrl Pts',(-15.1920701163804,-39.6676501731673,
0.));
#22854=CARTESIAN_POINT('Ctrl Pts',(-15.1920701163804,-39.6676501731673,
18.));
#22855=CARTESIAN_POINT('Ctrl Pts',(-15.1797227547562,-39.7688841338802,
0.));
#22856=CARTESIAN_POINT('Ctrl Pts',(-15.1797227547562,-39.7688841338802,
18.));
#22857=CARTESIAN_POINT('Ctrl Pts',(-15.1668418393198,-39.8701855339908,
0.));
#22858=CARTESIAN_POINT('Ctrl Pts',(-15.1668418393198,-39.8701855339908,
18.));
#22859=CARTESIAN_POINT('Ctrl Pts',(-15.1534306754871,-39.9715519332134,
0.));
#22860=CARTESIAN_POINT('Ctrl Pts',(-15.1534306754871,-39.9715519332134,
18.));
#22861=CARTESIAN_POINT('Ctrl Pts',(-15.1394923361537,-40.0729810652204,
0.));
#22862=CARTESIAN_POINT('Ctrl Pts',(-15.1394923361537,-40.0729810652204,
18.));
#22863=CARTESIAN_POINT('Ctrl Pts',(-15.1250297462408,-40.1744707357902,
0.));
#22864=CARTESIAN_POINT('Ctrl Pts',(-15.1250297462408,-40.1744707357902,
18.));
#22865=CARTESIAN_POINT('Ctrl Pts',(-15.1100457495259,-40.2760187401821,
0.));
#22866=CARTESIAN_POINT('Ctrl Pts',(-15.1100457495259,-40.2760187401821,
18.));
#22867=CARTESIAN_POINT('Ctrl Pts',(-15.0945431800724,-40.3776227809037,
0.));
#22868=CARTESIAN_POINT('Ctrl Pts',(-15.0945431800724,-40.3776227809037,
18.));
#22869=CARTESIAN_POINT('Ctrl Pts',(-15.0785249502524,-40.4792803645352,
0.));
#22870=CARTESIAN_POINT('Ctrl Pts',(-15.0785249502524,-40.4792803645352,
18.));
#22871=CARTESIAN_POINT('Ctrl Pts',(-15.0619940893017,-40.58098877043,0.));
#22872=CARTESIAN_POINT('Ctrl Pts',(-15.0619940893017,-40.58098877043,18.));
#22873=CARTESIAN_POINT('Ctrl Pts',(-15.0449536183143,-40.6827452453667,
0.));
#22874=CARTESIAN_POINT('Ctrl Pts',(-15.0449536183143,-40.6827452453667,
18.));
#22875=CARTESIAN_POINT('Ctrl Pts',(-15.0274064563211,-40.7845471608654,
0.));
#22876=CARTESIAN_POINT('Ctrl Pts',(-15.0274064563211,-40.7845471608654,
18.));
#22877=CARTESIAN_POINT('Ctrl Pts',(-15.0093553188655,-40.8863921801,0.));
#22878=CARTESIAN_POINT('Ctrl Pts',(-15.0093553188655,-40.8863921801,18.));
#22879=CARTESIAN_POINT('Ctrl Pts',(-14.9908026205824,-40.9882784321884,
0.));
#22880=CARTESIAN_POINT('Ctrl Pts',(-14.9908026205824,-40.9882784321884,
18.));
#22881=CARTESIAN_POINT('Ctrl Pts',(-14.9717503874227,-41.0902046498729,
0.));
#22882=CARTESIAN_POINT('Ctrl Pts',(-14.9717503874227,-41.0902046498729,
18.));
#22883=CARTESIAN_POINT('Ctrl Pts',(-14.9522002356298,-41.1921700381957,
0.));
#22884=CARTESIAN_POINT('Ctrl Pts',(-14.9522002356298,-41.1921700381957,
18.));
#22885=CARTESIAN_POINT('Ctrl Pts',(-14.936162723752,-41.2737733455422,0.));
#22886=CARTESIAN_POINT('Ctrl Pts',(-14.936162723752,-41.2737733455422,18.));
#22887=CARTESIAN_POINT('Ctrl Pts',(-14.9239113834707,-41.3349931861715,
0.));
#22888=CARTESIAN_POINT('Ctrl Pts',(-14.9239113834707,-41.3349931861715,
18.));
#22889=CARTESIAN_POINT('Ctrl Pts',(-14.9156446533966,-41.3758141263348,
0.));
#22890=CARTESIAN_POINT('Ctrl Pts',(-14.9156446533966,-41.3758141263348,
18.));
#22891=CARTESIAN_POINT('Ctrl Pts',(-14.911486495888,-41.396226524684,0.));
#22892=CARTESIAN_POINT('Ctrl Pts',(-14.911486495888,-41.396226524684,18.));
#22893=CARTESIAN_POINT('Ctrl Pts',(-14.9001523628048,-34.5082745737944,
0.));
#22894=CARTESIAN_POINT('Ctrl Pts',(-14.9076710061311,-34.525687510388,0.));
#22895=CARTESIAN_POINT('Ctrl Pts',(-14.9222326355678,-34.5606858566713,
0.));
#22896=CARTESIAN_POINT('Ctrl Pts',(-14.9426481276593,-34.6137007885254,
0.));
#22897=CARTESIAN_POINT('Ctrl Pts',(-14.9671565602316,-34.6853717911268,
0.));
#22898=CARTESIAN_POINT('Ctrl Pts',(-14.9940927023322,-34.7763085406486,
0.));
#22899=CARTESIAN_POINT('Ctrl Pts',(-15.0183713484962,-34.8682205930809,
0.));
#22900=CARTESIAN_POINT('Ctrl Pts',(-15.041018569143,-34.9607388363587,0.));
#22901=CARTESIAN_POINT('Ctrl Pts',(-15.0627878528202,-35.0535882932913,
0.));
#22902=CARTESIAN_POINT('Ctrl Pts',(-15.08395927165,-35.1466591020976,0.));
#22903=CARTESIAN_POINT('Ctrl Pts',(-15.104500806927,-35.2399506932815,0.));
#22904=CARTESIAN_POINT('Ctrl Pts',(-15.1241934020682,-35.3335286891314,
0.));
#22905=CARTESIAN_POINT('Ctrl Pts',(-15.1427632633831,-35.4274792115856,
0.));
#22906=CARTESIAN_POINT('Ctrl Pts',(-15.1600260710384,-35.5218591529745,
0.));
#22907=CARTESIAN_POINT('Ctrl Pts',(-15.1759785763051,-35.6166644736253,
0.));
#22908=CARTESIAN_POINT('Ctrl Pts',(-15.1907243629659,-35.7118553943773,
0.));
#22909=CARTESIAN_POINT('Ctrl Pts',(-15.2044274601769,-35.8073720252878,
0.));
#22910=CARTESIAN_POINT('Ctrl Pts',(-15.2172585668056,-35.9031525499277,
0.));
#22911=CARTESIAN_POINT('Ctrl Pts',(-15.2293360946131,-35.9991531408727,
0.));
#22912=CARTESIAN_POINT('Ctrl Pts',(-15.240697754828,-36.095357546697,0.));
#22913=CARTESIAN_POINT('Ctrl Pts',(-15.2513334565427,-36.1917659216814,
0.));
#22914=CARTESIAN_POINT('Ctrl Pts',(-15.2612053303774,-36.2883880151607,
0.));
#22915=CARTESIAN_POINT('Ctrl Pts',(-15.2702711460937,-36.3852352131887,
0.));
#22916=CARTESIAN_POINT('Ctrl Pts',(-15.2785104654792,-36.4823116513289,
0.));
#22917=CARTESIAN_POINT('Ctrl Pts',(-15.2859343913094,-36.5796108931244,
0.));
#22918=CARTESIAN_POINT('Ctrl Pts',(-15.2925717100767,-36.6771206167755,
0.));
#22919=CARTESIAN_POINT('Ctrl Pts',(-15.2984606286738,-36.7748254044502,
0.));
#22920=CARTESIAN_POINT('Ctrl Pts',(-15.3036390436952,-36.8727100302512,
0.));
#22921=CARTESIAN_POINT('Ctrl Pts',(-15.3081335446406,-36.970763176802,0.));
#22922=CARTESIAN_POINT('Ctrl Pts',(-15.3119562971444,-37.0689784837457,
0.));
#22923=CARTESIAN_POINT('Ctrl Pts',(-15.3151109648809,-37.1673525354641,
0.));
#22924=CARTESIAN_POINT('Ctrl Pts',(-15.3175963510698,-37.2658836214694,
0.));
#22925=CARTESIAN_POINT('Ctrl Pts',(-15.3194106233802,-37.3645702997848,
0.));
#22926=CARTESIAN_POINT('Ctrl Pts',(-15.3205561366169,-37.4634097578665,
0.));
#22927=CARTESIAN_POINT('Ctrl Pts',(-15.3210406145546,-37.562397408596,0.));
#22928=CARTESIAN_POINT('Ctrl Pts',(-15.3208746890781,-37.6615277218027,
0.));
#22929=CARTESIAN_POINT('Ctrl Pts',(-15.320070396385,-37.7607947318286,0.));
#22930=CARTESIAN_POINT('Ctrl Pts',(-15.3186394335023,-37.8601926265378,
0.));
#22931=CARTESIAN_POINT('Ctrl Pts',(-15.3165911656268,-37.959716421934,0.));
#22932=CARTESIAN_POINT('Ctrl Pts',(-15.3139321941687,-38.0593621055415,
0.));
#22933=CARTESIAN_POINT('Ctrl Pts',(-15.310667421514,-38.1591262705847,0.));
#22934=CARTESIAN_POINT('Ctrl Pts',(-15.3068007250314,-38.2590058835965,
0.));
#22935=CARTESIAN_POINT('Ctrl Pts',(-15.3023357307483,-38.3589980188324,
0.));
#22936=CARTESIAN_POINT('Ctrl Pts',(-15.297276703747,-38.4590995527814,0.));
#22937=CARTESIAN_POINT('Ctrl Pts',(-15.2916287700102,-38.5593070891769,
0.));
#22938=CARTESIAN_POINT('Ctrl Pts',(-15.2853974668211,-38.659617115053,0.));
#22939=CARTESIAN_POINT('Ctrl Pts',(-15.2785884727112,-38.7600260961351,
0.));
#22940=CARTESIAN_POINT('Ctrl Pts',(-15.2712072937639,-38.860530586589,0.));
#22941=CARTESIAN_POINT('Ctrl Pts',(-15.2632589109473,-38.9611273555758,
0.));
#22942=CARTESIAN_POINT('Ctrl Pts',(-15.2547476855825,-39.061813415425,0.));
#22943=CARTESIAN_POINT('Ctrl Pts',(-15.2456775636447,-39.1625859371304,
0.));
#22944=CARTESIAN_POINT('Ctrl Pts',(-15.2360522089072,-39.2634421927888,
0.));
#22945=CARTESIAN_POINT('Ctrl Pts',(-15.225875156307,-39.3643794927167,0.));
#22946=CARTESIAN_POINT('Ctrl Pts',(-15.2151499908149,-39.4653951093947,
0.));
#22947=CARTESIAN_POINT('Ctrl Pts',(-15.2038804098649,-39.5664862602472,
0.));
#22948=CARTESIAN_POINT('Ctrl Pts',(-15.1920701163804,-39.6676501731673,
0.));
#22949=CARTESIAN_POINT('Ctrl Pts',(-15.1797227547562,-39.7688841338802,
0.));
#22950=CARTESIAN_POINT('Ctrl Pts',(-15.1668418393198,-39.8701855339908,
0.));
#22951=CARTESIAN_POINT('Ctrl Pts',(-15.1534306754871,-39.9715519332134,
0.));
#22952=CARTESIAN_POINT('Ctrl Pts',(-15.1394923361537,-40.0729810652204,
0.));
#22953=CARTESIAN_POINT('Ctrl Pts',(-15.1250297462408,-40.1744707357902,
0.));
#22954=CARTESIAN_POINT('Ctrl Pts',(-15.1100457495259,-40.2760187401821,
0.));
#22955=CARTESIAN_POINT('Ctrl Pts',(-15.0945431800724,-40.3776227809037,
0.));
#22956=CARTESIAN_POINT('Ctrl Pts',(-15.0785249502524,-40.4792803645352,
0.));
#22957=CARTESIAN_POINT('Ctrl Pts',(-15.0619940893017,-40.58098877043,0.));
#22958=CARTESIAN_POINT('Ctrl Pts',(-15.0449536183143,-40.6827452453667,
0.));
#22959=CARTESIAN_POINT('Ctrl Pts',(-15.0274064563211,-40.7845471608654,
0.));
#22960=CARTESIAN_POINT('Ctrl Pts',(-15.0093553188655,-40.8863921801,0.));
#22961=CARTESIAN_POINT('Ctrl Pts',(-14.9908026205824,-40.9882784321884,
0.));
#22962=CARTESIAN_POINT('Ctrl Pts',(-14.9679399407908,-41.1105898934098,
0.));
#22963=CARTESIAN_POINT('Ctrl Pts',(-14.9482653093396,-41.2125650743922,
0.));
#22964=CARTESIAN_POINT('Ctrl Pts',(-14.9321285285561,-41.2941761025922,
0.));
#22965=CARTESIAN_POINT('Ctrl Pts',(-14.919802810928,-41.3554017279611,0.));
#22966=CARTESIAN_POINT('Ctrl Pts',(-14.911486495888,-41.396226524684,0.));
#22967=CARTESIAN_POINT('Ctrl Pts',(-14.9001523628048,-34.5082745737944,
15.));
#22968=CARTESIAN_POINT('Ctrl Pts',(-14.9076710061311,-34.525687510388,15.));
#22969=CARTESIAN_POINT('Ctrl Pts',(-14.9222326355678,-34.5606858566713,
15.));
#22970=CARTESIAN_POINT('Ctrl Pts',(-14.9426481276593,-34.6137007885254,
15.));
#22971=CARTESIAN_POINT('Ctrl Pts',(-14.9671565602316,-34.6853717911268,
15.));
#22972=CARTESIAN_POINT('Ctrl Pts',(-14.9940927023322,-34.7763085406486,
15.));
#22973=CARTESIAN_POINT('Ctrl Pts',(-15.0183713484962,-34.8682205930809,
15.));
#22974=CARTESIAN_POINT('Ctrl Pts',(-15.041018569143,-34.9607388363587,15.));
#22975=CARTESIAN_POINT('Ctrl Pts',(-15.0627878528202,-35.0535882932913,
15.));
#22976=CARTESIAN_POINT('Ctrl Pts',(-15.08395927165,-35.1466591020976,15.));
#22977=CARTESIAN_POINT('Ctrl Pts',(-15.104500806927,-35.2399506932815,15.));
#22978=CARTESIAN_POINT('Ctrl Pts',(-15.1241934020682,-35.3335286891314,
15.));
#22979=CARTESIAN_POINT('Ctrl Pts',(-15.1427632633831,-35.4274792115856,
15.));
#22980=CARTESIAN_POINT('Ctrl Pts',(-15.1600260710384,-35.5218591529745,
15.));
#22981=CARTESIAN_POINT('Ctrl Pts',(-15.1759785763051,-35.6166644736253,
15.));
#22982=CARTESIAN_POINT('Ctrl Pts',(-15.1907243629659,-35.7118553943773,
15.));
#22983=CARTESIAN_POINT('Ctrl Pts',(-15.2044274601769,-35.8073720252878,
15.));
#22984=CARTESIAN_POINT('Ctrl Pts',(-15.2172585668056,-35.9031525499277,
15.));
#22985=CARTESIAN_POINT('Ctrl Pts',(-15.2293360946131,-35.9991531408727,
15.));
#22986=CARTESIAN_POINT('Ctrl Pts',(-15.240697754828,-36.095357546697,15.));
#22987=CARTESIAN_POINT('Ctrl Pts',(-15.2513334565427,-36.1917659216814,
15.));
#22988=CARTESIAN_POINT('Ctrl Pts',(-15.2612053303774,-36.2883880151607,
15.));
#22989=CARTESIAN_POINT('Ctrl Pts',(-15.2702711460937,-36.3852352131887,
15.));
#22990=CARTESIAN_POINT('Ctrl Pts',(-15.2785104654792,-36.4823116513289,
15.));
#22991=CARTESIAN_POINT('Ctrl Pts',(-15.2859343913094,-36.5796108931244,
15.));
#22992=CARTESIAN_POINT('Ctrl Pts',(-15.2925717100767,-36.6771206167755,
15.));
#22993=CARTESIAN_POINT('Ctrl Pts',(-15.2984606286738,-36.7748254044502,
15.));
#22994=CARTESIAN_POINT('Ctrl Pts',(-15.3036390436952,-36.8727100302512,
15.));
#22995=CARTESIAN_POINT('Ctrl Pts',(-15.3081335446406,-36.970763176802,15.));
#22996=CARTESIAN_POINT('Ctrl Pts',(-15.3119562971444,-37.0689784837457,
15.));
#22997=CARTESIAN_POINT('Ctrl Pts',(-15.3151109648809,-37.1673525354641,
15.));
#22998=CARTESIAN_POINT('Ctrl Pts',(-15.3175963510698,-37.2658836214694,
15.));
#22999=CARTESIAN_POINT('Ctrl Pts',(-15.3194106233802,-37.3645702997848,
15.));
#23000=CARTESIAN_POINT('Ctrl Pts',(-15.3205561366169,-37.4634097578665,
15.));
#23001=CARTESIAN_POINT('Ctrl Pts',(-15.3210406145546,-37.562397408596,15.));
#23002=CARTESIAN_POINT('Ctrl Pts',(-15.3208746890781,-37.6615277218027,
15.));
#23003=CARTESIAN_POINT('Ctrl Pts',(-15.320070396385,-37.7607947318286,15.));
#23004=CARTESIAN_POINT('Ctrl Pts',(-15.3186394335023,-37.8601926265378,
15.));
#23005=CARTESIAN_POINT('Ctrl Pts',(-15.3165911656268,-37.959716421934,15.));
#23006=CARTESIAN_POINT('Ctrl Pts',(-15.3139321941687,-38.0593621055415,
15.));
#23007=CARTESIAN_POINT('Ctrl Pts',(-15.310667421514,-38.1591262705847,15.));
#23008=CARTESIAN_POINT('Ctrl Pts',(-15.3068007250314,-38.2590058835965,
15.));
#23009=CARTESIAN_POINT('Ctrl Pts',(-15.3023357307483,-38.3589980188324,
15.));
#23010=CARTESIAN_POINT('Ctrl Pts',(-15.297276703747,-38.4590995527814,15.));
#23011=CARTESIAN_POINT('Ctrl Pts',(-15.2916287700102,-38.5593070891769,
15.));
#23012=CARTESIAN_POINT('Ctrl Pts',(-15.2853974668211,-38.659617115053,15.));
#23013=CARTESIAN_POINT('Ctrl Pts',(-15.2785884727112,-38.7600260961351,
15.));
#23014=CARTESIAN_POINT('Ctrl Pts',(-15.2712072937639,-38.860530586589,15.));
#23015=CARTESIAN_POINT('Ctrl Pts',(-15.2632589109473,-38.9611273555758,
15.));
#23016=CARTESIAN_POINT('Ctrl Pts',(-15.2547476855825,-39.061813415425,15.));
#23017=CARTESIAN_POINT('Ctrl Pts',(-15.2456775636447,-39.1625859371304,
15.));
#23018=CARTESIAN_POINT('Ctrl Pts',(-15.2360522089072,-39.2634421927888,
15.));
#23019=CARTESIAN_POINT('Ctrl Pts',(-15.225875156307,-39.3643794927167,15.));
#23020=CARTESIAN_POINT('Ctrl Pts',(-15.2151499908149,-39.4653951093947,
15.));
#23021=CARTESIAN_POINT('Ctrl Pts',(-15.2038804098649,-39.5664862602472,
15.));
#23022=CARTESIAN_POINT('Ctrl Pts',(-15.1920701163804,-39.6676501731673,
15.));
#23023=CARTESIAN_POINT('Ctrl Pts',(-15.1797227547562,-39.7688841338802,
15.));
#23024=CARTESIAN_POINT('Ctrl Pts',(-15.1668418393198,-39.8701855339908,
15.));
#23025=CARTESIAN_POINT('Ctrl Pts',(-15.1534306754871,-39.9715519332134,
15.));
#23026=CARTESIAN_POINT('Ctrl Pts',(-15.1394923361537,-40.0729810652204,
15.));
#23027=CARTESIAN_POINT('Ctrl Pts',(-15.1250297462408,-40.1744707357902,
15.));
#23028=CARTESIAN_POINT('Ctrl Pts',(-15.1100457495259,-40.2760187401821,
15.));
#23029=CARTESIAN_POINT('Ctrl Pts',(-15.0945431800724,-40.3776227809037,
15.));
#23030=CARTESIAN_POINT('Ctrl Pts',(-15.0785249502524,-40.4792803645352,
15.));
#23031=CARTESIAN_POINT('Ctrl Pts',(-15.0619940893017,-40.58098877043,15.));
#23032=CARTESIAN_POINT('Ctrl Pts',(-15.0449536183143,-40.6827452453667,
15.));
#23033=CARTESIAN_POINT('Ctrl Pts',(-15.0274064563211,-40.7845471608654,
15.));
#23034=CARTESIAN_POINT('Ctrl Pts',(-15.0093553188655,-40.8863921801,15.));
#23035=CARTESIAN_POINT('Ctrl Pts',(-14.9908026205824,-40.9882784321884,
15.));
#23036=CARTESIAN_POINT('Ctrl Pts',(-14.9679399407908,-41.1105898934098,
15.));
#23037=CARTESIAN_POINT('Ctrl Pts',(-14.9482653093396,-41.2125650743922,
15.));
#23038=CARTESIAN_POINT('Ctrl Pts',(-14.9321285285561,-41.2941761025922,
15.));
#23039=CARTESIAN_POINT('Ctrl Pts',(-14.919802810928,-41.3554017279611,15.));
#23040=CARTESIAN_POINT('Ctrl Pts',(-14.911486495888,-41.396226524684,15.));
#23041=CARTESIAN_POINT('Ctrl Pts',(-24.725498909423,-36.3957374383337,0.));
#23042=CARTESIAN_POINT('Ctrl Pts',(-24.725498909423,-36.3957374383337,18.));
#23043=CARTESIAN_POINT('Ctrl Pts',(-24.7065408286023,-36.3871033517098,
0.));
#23044=CARTESIAN_POINT('Ctrl Pts',(-24.7065408286023,-36.3871033517098,
18.));
#23045=CARTESIAN_POINT('Ctrl Pts',(-24.6686569322616,-36.369797330215,0.));
#23046=CARTESIAN_POINT('Ctrl Pts',(-24.6686569322616,-36.369797330215,18.));
#23047=CARTESIAN_POINT('Ctrl Pts',(-24.6119278836614,-36.3437247532368,
0.));
#23048=CARTESIAN_POINT('Ctrl Pts',(-24.6119278836614,-36.3437247532368,
18.));
#23049=CARTESIAN_POINT('Ctrl Pts',(-24.5364828082556,-36.3087341522969,
0.));
#23050=CARTESIAN_POINT('Ctrl Pts',(-24.5364828082556,-36.3087341522969,
18.));
#23051=CARTESIAN_POINT('Ctrl Pts',(-24.4424997853605,-36.2646168058395,
0.));
#23052=CARTESIAN_POINT('Ctrl Pts',(-24.4424997853605,-36.2646168058395,
18.));
#23053=CARTESIAN_POINT('Ctrl Pts',(-24.3488411214068,-36.2201196586696,
0.));
#23054=CARTESIAN_POINT('Ctrl Pts',(-24.3488411214068,-36.2201196586696,
18.));
#23055=CARTESIAN_POINT('Ctrl Pts',(-24.2555084095332,-36.1752418704833,
0.));
#23056=CARTESIAN_POINT('Ctrl Pts',(-24.2555084095332,-36.1752418704833,
18.));
#23057=CARTESIAN_POINT('Ctrl Pts',(-24.1625038657964,-36.1299825471271,
0.));
#23058=CARTESIAN_POINT('Ctrl Pts',(-24.1625038657964,-36.1299825471271,
18.));
#23059=CARTESIAN_POINT('Ctrl Pts',(-24.0698304230588,-36.0843408347974,
0.));
#23060=CARTESIAN_POINT('Ctrl Pts',(-24.0698304230588,-36.0843408347974,
18.));
#23061=CARTESIAN_POINT('Ctrl Pts',(-23.9774915680089,-36.0383159101253,
0.));
#23062=CARTESIAN_POINT('Ctrl Pts',(-23.9774915680089,-36.0383159101253,
18.));
#23063=CARTESIAN_POINT('Ctrl Pts',(-23.8854911428946,-35.9919069565469,
0.));
#23064=CARTESIAN_POINT('Ctrl Pts',(-23.8854911428946,-35.9919069565469,
18.));
#23065=CARTESIAN_POINT('Ctrl Pts',(-23.7938331508737,-35.9451131482488,
0.));
#23066=CARTESIAN_POINT('Ctrl Pts',(-23.7938331508737,-35.9451131482488,
18.));
#23067=CARTESIAN_POINT('Ctrl Pts',(-23.7025215735353,-35.8979336336837,
0.));
#23068=CARTESIAN_POINT('Ctrl Pts',(-23.7025215735353,-35.8979336336837,
18.));
#23069=CARTESIAN_POINT('Ctrl Pts',(-23.611560139948,-35.8503675222885,0.));
#23070=CARTESIAN_POINT('Ctrl Pts',(-23.611560139948,-35.8503675222885,18.));
#23071=CARTESIAN_POINT('Ctrl Pts',(-23.5209523746427,-35.8024138716896,
0.));
#23072=CARTESIAN_POINT('Ctrl Pts',(-23.5209523746427,-35.8024138716896,
18.));
#23073=CARTESIAN_POINT('Ctrl Pts',(-23.4307017328227,-35.7540716771372,
0.));
#23074=CARTESIAN_POINT('Ctrl Pts',(-23.4307017328227,-35.7540716771372,
18.));
#23075=CARTESIAN_POINT('Ctrl Pts',(-23.3408117088762,-35.7053398620512,
0.));
#23076=CARTESIAN_POINT('Ctrl Pts',(-23.3408117088762,-35.7053398620512,
18.));
#23077=CARTESIAN_POINT('Ctrl Pts',(-23.2512859425032,-35.6562172725207,
0.));
#23078=CARTESIAN_POINT('Ctrl Pts',(-23.2512859425032,-35.6562172725207,
18.));
#23079=CARTESIAN_POINT('Ctrl Pts',(-23.1621283508111,-35.6067026687722,
0.));
#23080=CARTESIAN_POINT('Ctrl Pts',(-23.1621283508111,-35.6067026687722,
18.));
#23081=CARTESIAN_POINT('Ctrl Pts',(-23.0733431097058,-35.5567947408311,
0.));
#23082=CARTESIAN_POINT('Ctrl Pts',(-23.0733431097058,-35.5567947408311,
18.));
#23083=CARTESIAN_POINT('Ctrl Pts',(-22.9849345572033,-35.5064921357308,
0.));
#23084=CARTESIAN_POINT('Ctrl Pts',(-22.9849345572033,-35.5064921357308,
18.));
#23085=CARTESIAN_POINT('Ctrl Pts',(-22.8969071125089,-35.4557934871468,
0.));
#23086=CARTESIAN_POINT('Ctrl Pts',(-22.8969071125089,-35.4557934871468,
18.));
#23087=CARTESIAN_POINT('Ctrl Pts',(-22.8092652000706,-35.4046974393492,
0.));
#23088=CARTESIAN_POINT('Ctrl Pts',(-22.8092652000706,-35.4046974393492,
18.));
#23089=CARTESIAN_POINT('Ctrl Pts',(-22.7220131336912,-35.3532026952313,
0.));
#23090=CARTESIAN_POINT('Ctrl Pts',(-22.7220131336912,-35.3532026952313,
18.));
#23091=CARTESIAN_POINT('Ctrl Pts',(-22.635155167154,-35.3013079759252,0.));
#23092=CARTESIAN_POINT('Ctrl Pts',(-22.635155167154,-35.3013079759252,18.));
#23093=CARTESIAN_POINT('Ctrl Pts',(-22.5486956608909,-35.2490119207975,
0.));
#23094=CARTESIAN_POINT('Ctrl Pts',(-22.5486956608909,-35.2490119207975,
18.));
#23095=CARTESIAN_POINT('Ctrl Pts',(-22.4626392230023,-35.1963130003352,
0.));
#23096=CARTESIAN_POINT('Ctrl Pts',(-22.4626392230023,-35.1963130003352,
18.));
#23097=CARTESIAN_POINT('Ctrl Pts',(-22.3769908340843,-35.1432094422642,
0.));
#23098=CARTESIAN_POINT('Ctrl Pts',(-22.3769908340843,-35.1432094422642,
18.));
#23099=CARTESIAN_POINT('Ctrl Pts',(-22.2917560356803,-35.0896991159359,
0.));
#23100=CARTESIAN_POINT('Ctrl Pts',(-22.2917560356803,-35.0896991159359,
18.));
#23101=CARTESIAN_POINT('Ctrl Pts',(-22.2069408519233,-35.0357795922459,
0.));
#23102=CARTESIAN_POINT('Ctrl Pts',(-22.2069408519233,-35.0357795922459,
18.));
#23103=CARTESIAN_POINT('Ctrl Pts',(-22.1225514798584,-34.9814483545602,
0.));
#23104=CARTESIAN_POINT('Ctrl Pts',(-22.1225514798584,-34.9814483545602,
18.));
#23105=CARTESIAN_POINT('Ctrl Pts',(-22.0385940162683,-34.9267029879922,
0.));
#23106=CARTESIAN_POINT('Ctrl Pts',(-22.0385940162683,-34.9267029879922,
18.));
#23107=CARTESIAN_POINT('Ctrl Pts',(-21.9550742217675,-34.8715413418101,
0.));
#23108=CARTESIAN_POINT('Ctrl Pts',(-21.9550742217675,-34.8715413418101,
18.));
#23109=CARTESIAN_POINT('Ctrl Pts',(-21.8719971302817,-34.8159618014436,
0.));
#23110=CARTESIAN_POINT('Ctrl Pts',(-21.8719971302817,-34.8159618014436,
18.));
#23111=CARTESIAN_POINT('Ctrl Pts',(-21.7893672401137,-34.7599631530844,
0.));
#23112=CARTESIAN_POINT('Ctrl Pts',(-21.7893672401137,-34.7599631530844,
18.));
#23113=CARTESIAN_POINT('Ctrl Pts',(-21.7071892844497,-34.7035440429025,
0.));
#23114=CARTESIAN_POINT('Ctrl Pts',(-21.7071892844497,-34.7035440429025,
18.));
#23115=CARTESIAN_POINT('Ctrl Pts',(-21.6254689009796,-34.6467025072367,
0.));
#23116=CARTESIAN_POINT('Ctrl Pts',(-21.6254689009796,-34.6467025072367,
18.));
#23117=CARTESIAN_POINT('Ctrl Pts',(-21.5442132160757,-34.5894355639081,
0.));
#23118=CARTESIAN_POINT('Ctrl Pts',(-21.5442132160757,-34.5894355639081,
18.));
#23119=CARTESIAN_POINT('Ctrl Pts',(-21.4634317666005,-34.5317385658329,
0.));
#23120=CARTESIAN_POINT('Ctrl Pts',(-21.4634317666005,-34.5317385658329,
18.));
#23121=CARTESIAN_POINT('Ctrl Pts',(-21.3831361300104,-34.4736054662052,
0.));
#23122=CARTESIAN_POINT('Ctrl Pts',(-21.3831361300104,-34.4736054662052,
18.));
#23123=CARTESIAN_POINT('Ctrl Pts',(-21.3033382073239,-34.4150300340623,
0.));
#23124=CARTESIAN_POINT('Ctrl Pts',(-21.3033382073239,-34.4150300340623,
18.));
#23125=CARTESIAN_POINT('Ctrl Pts',(-21.2240487218079,-34.3560069185815,
0.));
#23126=CARTESIAN_POINT('Ctrl Pts',(-21.2240487218079,-34.3560069185815,
18.));
#23127=CARTESIAN_POINT('Ctrl Pts',(-21.1452759244399,-34.2965325673384,
0.));
#23128=CARTESIAN_POINT('Ctrl Pts',(-21.1452759244399,-34.2965325673384,
18.));
#23129=CARTESIAN_POINT('Ctrl Pts',(-21.0670234747355,-34.2366067284279,
0.));
#23130=CARTESIAN_POINT('Ctrl Pts',(-21.0670234747355,-34.2366067284279,
18.));
#23131=CARTESIAN_POINT('Ctrl Pts',(-20.9892914622612,-34.176231731809,0.));
#23132=CARTESIAN_POINT('Ctrl Pts',(-20.9892914622612,-34.176231731809,18.));
#23133=CARTESIAN_POINT('Ctrl Pts',(-20.9120805673809,-34.1154095510973,
0.));
#23134=CARTESIAN_POINT('Ctrl Pts',(-20.9120805673809,-34.1154095510973,
18.));
#23135=CARTESIAN_POINT('Ctrl Pts',(-20.8353957068415,-34.0541392299678,
0.));
#23136=CARTESIAN_POINT('Ctrl Pts',(-20.8353957068415,-34.0541392299678,
18.));
#23137=CARTESIAN_POINT('Ctrl Pts',(-20.7592491770603,-33.9924146647395,
0.));
#23138=CARTESIAN_POINT('Ctrl Pts',(-20.7592491770603,-33.9924146647395,
18.));
#23139=CARTESIAN_POINT('Ctrl Pts',(-20.683665762903,-33.9302209962425,0.));
#23140=CARTESIAN_POINT('Ctrl Pts',(-20.683665762903,-33.9302209962425,18.));
#23141=CARTESIAN_POINT('Ctrl Pts',(-20.6086800574386,-33.8675365150454,
0.));
#23142=CARTESIAN_POINT('Ctrl Pts',(-20.6086800574386,-33.8675365150454,
18.));
#23143=CARTESIAN_POINT('Ctrl Pts',(-20.5343269914034,-33.8043393734971,
0.));
#23144=CARTESIAN_POINT('Ctrl Pts',(-20.5343269914034,-33.8043393734971,
18.));
#23145=CARTESIAN_POINT('Ctrl Pts',(-20.4606334536183,-33.7406135254082,
0.));
#23146=CARTESIAN_POINT('Ctrl Pts',(-20.4606334536183,-33.7406135254082,
18.));
#23147=CARTESIAN_POINT('Ctrl Pts',(-20.3876111773341,-33.6763537716992,
0.));
#23148=CARTESIAN_POINT('Ctrl Pts',(-20.3876111773341,-33.6763537716992,
18.));
#23149=CARTESIAN_POINT('Ctrl Pts',(-20.3152448035298,-33.6115742164079,
0.));
#23150=CARTESIAN_POINT('Ctrl Pts',(-20.3152448035298,-33.6115742164079,
18.));
#23151=CARTESIAN_POINT('Ctrl Pts',(-20.243500298383,-33.5463023319603,0.));
#23152=CARTESIAN_POINT('Ctrl Pts',(-20.243500298383,-33.5463023319603,18.));
#23153=CARTESIAN_POINT('Ctrl Pts',(-20.1723475154533,-33.480563024813,0.));
#23154=CARTESIAN_POINT('Ctrl Pts',(-20.1723475154533,-33.480563024813,18.));
#23155=CARTESIAN_POINT('Ctrl Pts',(-20.1017803986381,-33.4143643679979,
0.));
#23156=CARTESIAN_POINT('Ctrl Pts',(-20.1017803986381,-33.4143643679979,
18.));
#23157=CARTESIAN_POINT('Ctrl Pts',(-20.0318342617213,-33.3476854048385,
0.));
#23158=CARTESIAN_POINT('Ctrl Pts',(-20.0318342617213,-33.3476854048385,
18.));
#23159=CARTESIAN_POINT('Ctrl Pts',(-19.9626141625205,-33.2804560993213,
0.));
#23160=CARTESIAN_POINT('Ctrl Pts',(-19.9626141625205,-33.2804560993213,
18.));
#23161=CARTESIAN_POINT('Ctrl Pts',(-19.8942704458546,-33.2125746879471,
0.));
#23162=CARTESIAN_POINT('Ctrl Pts',(-19.8942704458546,-33.2125746879471,
18.));
#23163=CARTESIAN_POINT('Ctrl Pts',(-19.8269479776239,-33.1439436707661,
0.));
#23164=CARTESIAN_POINT('Ctrl Pts',(-19.8269479776239,-33.1439436707661,
18.));
#23165=CARTESIAN_POINT('Ctrl Pts',(-19.7607398248651,-33.0745026283418,
0.));
#23166=CARTESIAN_POINT('Ctrl Pts',(-19.7607398248651,-33.0745026283418,
18.));
#23167=CARTESIAN_POINT('Ctrl Pts',(-19.6956473461873,-33.004256563411,0.));
#23168=CARTESIAN_POINT('Ctrl Pts',(-19.6956473461873,-33.004256563411,18.));
#23169=CARTESIAN_POINT('Ctrl Pts',(-19.6315161742485,-32.9333211533788,
0.));
#23170=CARTESIAN_POINT('Ctrl Pts',(-19.6315161742485,-32.9333211533788,
18.));
#23171=CARTESIAN_POINT('Ctrl Pts',(-19.5681157030437,-32.8618672807884,
0.));
#23172=CARTESIAN_POINT('Ctrl Pts',(-19.5681157030437,-32.8618672807884,
18.));
#23173=CARTESIAN_POINT('Ctrl Pts',(-19.5052640847974,-32.7900335943248,
0.));
#23174=CARTESIAN_POINT('Ctrl Pts',(-19.5052640847974,-32.7900335943248,
18.));
#23175=CARTESIAN_POINT('Ctrl Pts',(-19.4429429601189,-32.7178463324062,
0.));
#23176=CARTESIAN_POINT('Ctrl Pts',(-19.4429429601189,-32.7178463324062,
18.));
#23177=CARTESIAN_POINT('Ctrl Pts',(-19.381405831319,-32.6451434870609,0.));
#23178=CARTESIAN_POINT('Ctrl Pts',(-19.381405831319,-32.6451434870609,18.));
#23179=CARTESIAN_POINT('Ctrl Pts',(-19.3213180490743,-32.5714771007861,
0.));
#23180=CARTESIAN_POINT('Ctrl Pts',(-19.3213180490743,-32.5714771007861,
18.));
#23181=CARTESIAN_POINT('Ctrl Pts',(-19.2635813403783,-32.4962340238036,
0.));
#23182=CARTESIAN_POINT('Ctrl Pts',(-19.2635813403783,-32.4962340238036,
18.));
#23183=CARTESIAN_POINT('Ctrl Pts',(-19.2200039764927,-32.4342791270009,
0.));
#23184=CARTESIAN_POINT('Ctrl Pts',(-19.2200039764927,-32.4342791270009,
18.));
#23185=CARTESIAN_POINT('Ctrl Pts',(-19.1891139208368,-32.3866012518553,
0.));
#23186=CARTESIAN_POINT('Ctrl Pts',(-19.1891139208368,-32.3866012518553,
18.));
#23187=CARTESIAN_POINT('Ctrl Pts',(-19.1693587749508,-32.3542491343753,
0.));
#23188=CARTESIAN_POINT('Ctrl Pts',(-19.1693587749508,-32.3542491343753,
18.));
#23189=CARTESIAN_POINT('Ctrl Pts',(-19.1596907609891,-32.3379313568208,
0.));
#23190=CARTESIAN_POINT('Ctrl Pts',(-19.1596907609891,-32.3379313568208,
18.));
#23191=CARTESIAN_POINT('',(-24.7254989094229,-36.3957374383337,0.));
#23192=CARTESIAN_POINT('Ctrl Pts',(-19.1596907609891,-32.3379313568208,
0.));
#23193=CARTESIAN_POINT('Ctrl Pts',(-19.1693587749508,-32.3542491343753,
0.));
#23194=CARTESIAN_POINT('Ctrl Pts',(-19.1891139208368,-32.3866012518553,
0.));
#23195=CARTESIAN_POINT('Ctrl Pts',(-19.2200039764927,-32.4342791270009,
0.));
#23196=CARTESIAN_POINT('Ctrl Pts',(-19.2635813403783,-32.4962340238036,
0.));
#23197=CARTESIAN_POINT('Ctrl Pts',(-19.3213180490743,-32.5714771007861,
0.));
#23198=CARTESIAN_POINT('Ctrl Pts',(-19.381405831319,-32.6451434870609,0.));
#23199=CARTESIAN_POINT('Ctrl Pts',(-19.4429429601189,-32.7178463324062,
0.));
#23200=CARTESIAN_POINT('Ctrl Pts',(-19.5052640847974,-32.7900335943248,
0.));
#23201=CARTESIAN_POINT('Ctrl Pts',(-19.5681157030437,-32.8618672807884,
0.));
#23202=CARTESIAN_POINT('Ctrl Pts',(-19.6315161742485,-32.9333211533788,
0.));
#23203=CARTESIAN_POINT('Ctrl Pts',(-19.6956473461873,-33.004256563411,0.));
#23204=CARTESIAN_POINT('Ctrl Pts',(-19.7607398248651,-33.0745026283418,
0.));
#23205=CARTESIAN_POINT('Ctrl Pts',(-19.8269479776239,-33.1439436707661,
0.));
#23206=CARTESIAN_POINT('Ctrl Pts',(-19.8942704458546,-33.2125746879471,
0.));
#23207=CARTESIAN_POINT('Ctrl Pts',(-19.9626141625205,-33.2804560993213,
0.));
#23208=CARTESIAN_POINT('Ctrl Pts',(-20.0318342617213,-33.3476854048385,
0.));
#23209=CARTESIAN_POINT('Ctrl Pts',(-20.1017803986381,-33.4143643679979,
0.));
#23210=CARTESIAN_POINT('Ctrl Pts',(-20.1723475154533,-33.480563024813,0.));
#23211=CARTESIAN_POINT('Ctrl Pts',(-20.243500298383,-33.5463023319603,0.));
#23212=CARTESIAN_POINT('Ctrl Pts',(-20.3152448035298,-33.6115742164079,
0.));
#23213=CARTESIAN_POINT('Ctrl Pts',(-20.3876111773341,-33.6763537716992,
0.));
#23214=CARTESIAN_POINT('Ctrl Pts',(-20.4606334536183,-33.7406135254082,
0.));
#23215=CARTESIAN_POINT('Ctrl Pts',(-20.5343269914034,-33.8043393734971,
0.));
#23216=CARTESIAN_POINT('Ctrl Pts',(-20.6086800574386,-33.8675365150454,
0.));
#23217=CARTESIAN_POINT('Ctrl Pts',(-20.683665762903,-33.9302209962425,0.));
#23218=CARTESIAN_POINT('Ctrl Pts',(-20.7592491770603,-33.9924146647395,
0.));
#23219=CARTESIAN_POINT('Ctrl Pts',(-20.8353957068415,-34.0541392299678,
0.));
#23220=CARTESIAN_POINT('Ctrl Pts',(-20.9120805673809,-34.1154095510973,
0.));
#23221=CARTESIAN_POINT('Ctrl Pts',(-20.9892914622612,-34.176231731809,0.));
#23222=CARTESIAN_POINT('Ctrl Pts',(-21.0670234747355,-34.2366067284279,
0.));
#23223=CARTESIAN_POINT('Ctrl Pts',(-21.1452759244399,-34.2965325673384,
0.));
#23224=CARTESIAN_POINT('Ctrl Pts',(-21.2240487218079,-34.3560069185815,
0.));
#23225=CARTESIAN_POINT('Ctrl Pts',(-21.3033382073239,-34.4150300340623,
0.));
#23226=CARTESIAN_POINT('Ctrl Pts',(-21.3831361300104,-34.4736054662052,
0.));
#23227=CARTESIAN_POINT('Ctrl Pts',(-21.4634317666005,-34.5317385658329,
0.));
#23228=CARTESIAN_POINT('Ctrl Pts',(-21.5442132160757,-34.5894355639081,
0.));
#23229=CARTESIAN_POINT('Ctrl Pts',(-21.6254689009796,-34.6467025072367,
0.));
#23230=CARTESIAN_POINT('Ctrl Pts',(-21.7071892844497,-34.7035440429025,
0.));
#23231=CARTESIAN_POINT('Ctrl Pts',(-21.7893672401137,-34.7599631530844,
0.));
#23232=CARTESIAN_POINT('Ctrl Pts',(-21.8719971302817,-34.8159618014436,
0.));
#23233=CARTESIAN_POINT('Ctrl Pts',(-21.9550742217675,-34.8715413418101,
0.));
#23234=CARTESIAN_POINT('Ctrl Pts',(-22.0385940162683,-34.9267029879922,
0.));
#23235=CARTESIAN_POINT('Ctrl Pts',(-22.1225514798584,-34.9814483545602,
0.));
#23236=CARTESIAN_POINT('Ctrl Pts',(-22.2069408519233,-35.0357795922459,
0.));
#23237=CARTESIAN_POINT('Ctrl Pts',(-22.2917560356803,-35.0896991159359,
0.));
#23238=CARTESIAN_POINT('Ctrl Pts',(-22.3769908340843,-35.1432094422642,
0.));
#23239=CARTESIAN_POINT('Ctrl Pts',(-22.4626392230023,-35.1963130003352,
0.));
#23240=CARTESIAN_POINT('Ctrl Pts',(-22.5486956608909,-35.2490119207975,
0.));
#23241=CARTESIAN_POINT('Ctrl Pts',(-22.635155167154,-35.3013079759252,0.));
#23242=CARTESIAN_POINT('Ctrl Pts',(-22.7220131336912,-35.3532026952313,
0.));
#23243=CARTESIAN_POINT('Ctrl Pts',(-22.8092652000706,-35.4046974393492,
0.));
#23244=CARTESIAN_POINT('Ctrl Pts',(-22.8969071125089,-35.4557934871468,
0.));
#23245=CARTESIAN_POINT('Ctrl Pts',(-22.9849345572033,-35.5064921357308,
0.));
#23246=CARTESIAN_POINT('Ctrl Pts',(-23.0733431097058,-35.5567947408311,
0.));
#23247=CARTESIAN_POINT('Ctrl Pts',(-23.1621283508111,-35.6067026687722,
0.));
#23248=CARTESIAN_POINT('Ctrl Pts',(-23.2512859425032,-35.6562172725207,
0.));
#23249=CARTESIAN_POINT('Ctrl Pts',(-23.3408117088762,-35.7053398620512,
0.));
#23250=CARTESIAN_POINT('Ctrl Pts',(-23.4307017328227,-35.7540716771372,
0.));
#23251=CARTESIAN_POINT('Ctrl Pts',(-23.5209523746427,-35.8024138716896,
0.));
#23252=CARTESIAN_POINT('Ctrl Pts',(-23.611560139948,-35.8503675222885,0.));
#23253=CARTESIAN_POINT('Ctrl Pts',(-23.7025215735353,-35.8979336336837,
0.));
#23254=CARTESIAN_POINT('Ctrl Pts',(-23.7938331508737,-35.9451131482488,
0.));
#23255=CARTESIAN_POINT('Ctrl Pts',(-23.8854911428946,-35.9919069565469,
0.));
#23256=CARTESIAN_POINT('Ctrl Pts',(-23.9774915680089,-36.0383159101253,
0.));
#23257=CARTESIAN_POINT('Ctrl Pts',(-24.0698304230588,-36.0843408347974,
0.));
#23258=CARTESIAN_POINT('Ctrl Pts',(-24.1625038657964,-36.1299825471271,
0.));
#23259=CARTESIAN_POINT('Ctrl Pts',(-24.2555084095332,-36.1752418704833,
0.));
#23260=CARTESIAN_POINT('Ctrl Pts',(-24.3488411214068,-36.2201196586696,
0.));
#23261=CARTESIAN_POINT('Ctrl Pts',(-24.4612315181512,-36.2735162352735,
0.));
#23262=CARTESIAN_POINT('Ctrl Pts',(-24.5552956307817,-36.3175386315528,
0.));
#23263=CARTESIAN_POINT('Ctrl Pts',(-24.630805301288,-36.3524534604648,0.));
#23264=CARTESIAN_POINT('Ctrl Pts',(-24.6875827477484,-36.3784692650901,
0.));
#23265=CARTESIAN_POINT('Ctrl Pts',(-24.725498909423,-36.3957374383337,0.));
#23266=CARTESIAN_POINT('',(-24.7254989094229,-36.3957374383337,15.));
#23267=CARTESIAN_POINT('Ctrl Pts',(-24.725498909423,-36.3957374383337,15.));
#23268=CARTESIAN_POINT('Ctrl Pts',(-24.7065408286023,-36.3871033517098,
15.));
#23269=CARTESIAN_POINT('Ctrl Pts',(-24.6686569322616,-36.369797330215,15.));
#23270=CARTESIAN_POINT('Ctrl Pts',(-24.6119278836614,-36.3437247532368,
15.));
#23271=CARTESIAN_POINT('Ctrl Pts',(-24.5364828082556,-36.3087341522969,
15.));
#23272=CARTESIAN_POINT('Ctrl Pts',(-24.4424997853605,-36.2646168058395,
15.));
#23273=CARTESIAN_POINT('Ctrl Pts',(-24.3488411214068,-36.2201196586696,
15.));
#23274=CARTESIAN_POINT('Ctrl Pts',(-24.2555084095332,-36.1752418704833,
15.));
#23275=CARTESIAN_POINT('Ctrl Pts',(-24.1625038657964,-36.1299825471271,
15.));
#23276=CARTESIAN_POINT('Ctrl Pts',(-24.0698304230588,-36.0843408347974,
15.));
#23277=CARTESIAN_POINT('Ctrl Pts',(-23.9774915680089,-36.0383159101253,
15.));
#23278=CARTESIAN_POINT('Ctrl Pts',(-23.8854911428946,-35.9919069565469,
15.));
#23279=CARTESIAN_POINT('Ctrl Pts',(-23.7938331508737,-35.9451131482488,
15.));
#23280=CARTESIAN_POINT('Ctrl Pts',(-23.7025215735353,-35.8979336336837,
15.));
#23281=CARTESIAN_POINT('Ctrl Pts',(-23.611560139948,-35.8503675222885,15.));
#23282=CARTESIAN_POINT('Ctrl Pts',(-23.5209523746427,-35.8024138716896,
15.));
#23283=CARTESIAN_POINT('Ctrl Pts',(-23.4307017328227,-35.7540716771372,
15.));
#23284=CARTESIAN_POINT('Ctrl Pts',(-23.3408117088762,-35.7053398620512,
15.));
#23285=CARTESIAN_POINT('Ctrl Pts',(-23.2512859425032,-35.6562172725207,
15.));
#23286=CARTESIAN_POINT('Ctrl Pts',(-23.1621283508111,-35.6067026687722,
15.));
#23287=CARTESIAN_POINT('Ctrl Pts',(-23.0733431097058,-35.5567947408311,
15.));
#23288=CARTESIAN_POINT('Ctrl Pts',(-22.9849345572033,-35.5064921357308,
15.));
#23289=CARTESIAN_POINT('Ctrl Pts',(-22.8969071125089,-35.4557934871468,
15.));
#23290=CARTESIAN_POINT('Ctrl Pts',(-22.8092652000706,-35.4046974393492,
15.));
#23291=CARTESIAN_POINT('Ctrl Pts',(-22.7220131336912,-35.3532026952313,
15.));
#23292=CARTESIAN_POINT('Ctrl Pts',(-22.635155167154,-35.3013079759252,15.));
#23293=CARTESIAN_POINT('Ctrl Pts',(-22.5486956608909,-35.2490119207975,
15.));
#23294=CARTESIAN_POINT('Ctrl Pts',(-22.4626392230023,-35.1963130003352,
15.));
#23295=CARTESIAN_POINT('Ctrl Pts',(-22.3769908340843,-35.1432094422642,
15.));
#23296=CARTESIAN_POINT('Ctrl Pts',(-22.2917560356803,-35.0896991159359,
15.));
#23297=CARTESIAN_POINT('Ctrl Pts',(-22.2069408519233,-35.0357795922459,
15.));
#23298=CARTESIAN_POINT('Ctrl Pts',(-22.1225514798584,-34.9814483545602,
15.));
#23299=CARTESIAN_POINT('Ctrl Pts',(-22.0385940162683,-34.9267029879922,
15.));
#23300=CARTESIAN_POINT('Ctrl Pts',(-21.9550742217675,-34.8715413418101,
15.));
#23301=CARTESIAN_POINT('Ctrl Pts',(-21.8719971302817,-34.8159618014436,
15.));
#23302=CARTESIAN_POINT('Ctrl Pts',(-21.7893672401137,-34.7599631530844,
15.));
#23303=CARTESIAN_POINT('Ctrl Pts',(-21.7071892844497,-34.7035440429025,
15.));
#23304=CARTESIAN_POINT('Ctrl Pts',(-21.6254689009796,-34.6467025072367,
15.));
#23305=CARTESIAN_POINT('Ctrl Pts',(-21.5442132160757,-34.5894355639081,
15.));
#23306=CARTESIAN_POINT('Ctrl Pts',(-21.4634317666005,-34.5317385658329,
15.));
#23307=CARTESIAN_POINT('Ctrl Pts',(-21.3831361300104,-34.4736054662052,
15.));
#23308=CARTESIAN_POINT('Ctrl Pts',(-21.3033382073239,-34.4150300340623,
15.));
#23309=CARTESIAN_POINT('Ctrl Pts',(-21.2240487218079,-34.3560069185815,
15.));
#23310=CARTESIAN_POINT('Ctrl Pts',(-21.1452759244399,-34.2965325673384,
15.));
#23311=CARTESIAN_POINT('Ctrl Pts',(-21.0670234747355,-34.2366067284279,
15.));
#23312=CARTESIAN_POINT('Ctrl Pts',(-20.9892914622612,-34.176231731809,15.));
#23313=CARTESIAN_POINT('Ctrl Pts',(-20.9120805673809,-34.1154095510973,
15.));
#23314=CARTESIAN_POINT('Ctrl Pts',(-20.8353957068415,-34.0541392299678,
15.));
#23315=CARTESIAN_POINT('Ctrl Pts',(-20.7592491770603,-33.9924146647395,
15.));
#23316=CARTESIAN_POINT('Ctrl Pts',(-20.683665762903,-33.9302209962425,15.));
#23317=CARTESIAN_POINT('Ctrl Pts',(-20.6086800574386,-33.8675365150454,
15.));
#23318=CARTESIAN_POINT('Ctrl Pts',(-20.5343269914034,-33.8043393734971,
15.));
#23319=CARTESIAN_POINT('Ctrl Pts',(-20.4606334536183,-33.7406135254082,
15.));
#23320=CARTESIAN_POINT('Ctrl Pts',(-20.3876111773341,-33.6763537716992,
15.));
#23321=CARTESIAN_POINT('Ctrl Pts',(-20.3152448035298,-33.6115742164079,
15.));
#23322=CARTESIAN_POINT('Ctrl Pts',(-20.243500298383,-33.5463023319603,15.));
#23323=CARTESIAN_POINT('Ctrl Pts',(-20.1723475154533,-33.480563024813,15.));
#23324=CARTESIAN_POINT('Ctrl Pts',(-20.1017803986381,-33.4143643679979,
15.));
#23325=CARTESIAN_POINT('Ctrl Pts',(-20.0318342617213,-33.3476854048385,
15.));
#23326=CARTESIAN_POINT('Ctrl Pts',(-19.9626141625205,-33.2804560993213,
15.));
#23327=CARTESIAN_POINT('Ctrl Pts',(-19.8942704458546,-33.2125746879471,
15.));
#23328=CARTESIAN_POINT('Ctrl Pts',(-19.8269479776239,-33.1439436707661,
15.));
#23329=CARTESIAN_POINT('Ctrl Pts',(-19.7607398248651,-33.0745026283418,
15.));
#23330=CARTESIAN_POINT('Ctrl Pts',(-19.6956473461873,-33.004256563411,15.));
#23331=CARTESIAN_POINT('Ctrl Pts',(-19.6315161742485,-32.9333211533788,
15.));
#23332=CARTESIAN_POINT('Ctrl Pts',(-19.5681157030437,-32.8618672807884,
15.));
#23333=CARTESIAN_POINT('Ctrl Pts',(-19.5052640847974,-32.7900335943248,
15.));
#23334=CARTESIAN_POINT('Ctrl Pts',(-19.4429429601189,-32.7178463324062,
15.));
#23335=CARTESIAN_POINT('Ctrl Pts',(-19.381405831319,-32.6451434870609,15.));
#23336=CARTESIAN_POINT('Ctrl Pts',(-19.3213180490743,-32.5714771007861,
15.));
#23337=CARTESIAN_POINT('Ctrl Pts',(-19.2635813403783,-32.4962340238036,
15.));
#23338=CARTESIAN_POINT('Ctrl Pts',(-19.2200039764927,-32.4342791270009,
15.));
#23339=CARTESIAN_POINT('Ctrl Pts',(-19.1891139208368,-32.3866012518553,
15.));
#23340=CARTESIAN_POINT('Ctrl Pts',(-19.1693587749508,-32.3542491343753,
15.));
#23341=CARTESIAN_POINT('Ctrl Pts',(-19.1596907609891,-32.3379313568208,
15.));
#23342=CARTESIAN_POINT('',(-24.7254989094229,-36.3957374383337,0.));
#23343=CARTESIAN_POINT('Origin',(-6.66146233219319E-12,-9.16871631793044E-12,
0.));
#23344=CARTESIAN_POINT('',(-26.9738038986838,-34.762248247709,0.));
#23345=CARTESIAN_POINT('Origin',(-6.66146233219319E-12,-9.16871631793044E-12,
0.));
#23346=CARTESIAN_POINT('',(-26.9738038986838,-34.762248247709,15.));
#23347=CARTESIAN_POINT('Origin',(-6.66146233219319E-12,-9.16871631793044E-12,
15.));
#23348=CARTESIAN_POINT('',(-26.9738038986838,-34.762248247709,0.));
#23349=CARTESIAN_POINT('Ctrl Pts',(-24.8345302882955,-28.2149191006268,
0.));
#23350=CARTESIAN_POINT('Ctrl Pts',(-24.8345302882955,-28.2149191006268,
18.));
#23351=CARTESIAN_POINT('Ctrl Pts',(-24.8470618363541,-28.2291563988795,
0.));
#23352=CARTESIAN_POINT('Ctrl Pts',(-24.8470618363541,-28.2291563988795,
18.));
#23353=CARTESIAN_POINT('Ctrl Pts',(-24.8717258526943,-28.2579420132101,
0.));
#23354=CARTESIAN_POINT('Ctrl Pts',(-24.8717258526943,-28.2579420132101,
18.));
#23355=CARTESIAN_POINT('Ctrl Pts',(-24.9075246543798,-28.302053475606,0.));
#23356=CARTESIAN_POINT('Ctrl Pts',(-24.9075246543798,-28.302053475606,18.));
#23357=CARTESIAN_POINT('Ctrl Pts',(-24.9529811166897,-28.3626431274892,
0.));
#23358=CARTESIAN_POINT('Ctrl Pts',(-24.9529811166897,-28.3626431274892,
18.));
#23359=CARTESIAN_POINT('Ctrl Pts',(-25.0066999111736,-28.4408053900206,
0.));
#23360=CARTESIAN_POINT('Ctrl Pts',(-25.0066999111736,-28.4408053900206,
18.));
#23361=CARTESIAN_POINT('Ctrl Pts',(-25.0581926620043,-28.5207164321473,
0.));
#23362=CARTESIAN_POINT('Ctrl Pts',(-25.0581926620043,-28.5207164321473,
18.));
#23363=CARTESIAN_POINT('Ctrl Pts',(-25.108321158239,-28.6017081342376,0.));
#23364=CARTESIAN_POINT('Ctrl Pts',(-25.108321158239,-28.6017081342376,18.));
#23365=CARTESIAN_POINT('Ctrl Pts',(-25.1577170374459,-28.6832861366762,
0.));
#23366=CARTESIAN_POINT('Ctrl Pts',(-25.1577170374459,-28.6832861366762,
18.));
#23367=CARTESIAN_POINT('Ctrl Pts',(-25.2066127148845,-28.7652594076549,
0.));
#23368=CARTESIAN_POINT('Ctrl Pts',(-25.2066127148845,-28.7652594076549,
18.));
#23369=CARTESIAN_POINT('Ctrl Pts',(-25.2549775629725,-28.8476372998748,
0.));
#23370=CARTESIAN_POINT('Ctrl Pts',(-25.2549775629725,-28.8476372998748,
18.));
#23371=CARTESIAN_POINT('Ctrl Pts',(-25.3026235249214,-28.9305499160476,
0.));
#23372=CARTESIAN_POINT('Ctrl Pts',(-25.3026235249214,-28.9305499160476,
18.));
#23373=CARTESIAN_POINT('Ctrl Pts',(-25.3493168206005,-29.0141637699076,
0.));
#23374=CARTESIAN_POINT('Ctrl Pts',(-25.3493168206005,-29.0141637699076,
18.));
#23375=CARTESIAN_POINT('Ctrl Pts',(-25.3948997321279,-29.098589927237,0.));
#23376=CARTESIAN_POINT('Ctrl Pts',(-25.3948997321279,-29.098589927237,18.));
#23377=CARTESIAN_POINT('Ctrl Pts',(-25.4393679214513,-29.183825549991,0.));
#23378=CARTESIAN_POINT('Ctrl Pts',(-25.4393679214513,-29.183825549991,18.));
#23379=CARTESIAN_POINT('Ctrl Pts',(-25.4828076101654,-29.2698007967907,
0.));
#23380=CARTESIAN_POINT('Ctrl Pts',(-25.4828076101654,-29.2698007967907,
18.));
#23381=CARTESIAN_POINT('Ctrl Pts',(-25.5253562922582,-29.356408021119,0.));
#23382=CARTESIAN_POINT('Ctrl Pts',(-25.5253562922582,-29.356408021119,18.));
#23383=CARTESIAN_POINT('Ctrl Pts',(-25.5671572096726,-29.443535683207,0.));
#23384=CARTESIAN_POINT('Ctrl Pts',(-25.5671572096726,-29.443535683207,18.));
#23385=CARTESIAN_POINT('Ctrl Pts',(-25.6083094352667,-29.5311055094509,
0.));
#23386=CARTESIAN_POINT('Ctrl Pts',(-25.6083094352667,-29.5311055094509,
18.));
#23387=CARTESIAN_POINT('Ctrl Pts',(-25.6488438125835,-29.6190903904157,
0.));
#23388=CARTESIAN_POINT('Ctrl Pts',(-25.6488438125835,-29.6190903904157,
18.));
#23389=CARTESIAN_POINT('Ctrl Pts',(-25.6887507922748,-29.7074935910931,
0.));
#23390=CARTESIAN_POINT('Ctrl Pts',(-25.6887507922748,-29.7074935910931,
18.));
#23391=CARTESIAN_POINT('Ctrl Pts',(-25.7279973711305,-29.7963360859334,
0.));
#23392=CARTESIAN_POINT('Ctrl Pts',(-25.7279973711305,-29.7963360859334,
18.));
#23393=CARTESIAN_POINT('Ctrl Pts',(-25.7665469042913,-29.8856417535786,
0.));
#23394=CARTESIAN_POINT('Ctrl Pts',(-25.7665469042913,-29.8856417535786,
18.));
#23395=CARTESIAN_POINT('Ctrl Pts',(-25.8043812318215,-29.9754208429384,
0.));
#23396=CARTESIAN_POINT('Ctrl Pts',(-25.8043812318215,-29.9754208429384,
18.));
#23397=CARTESIAN_POINT('Ctrl Pts',(-25.8415089241134,-30.0656638016321,
0.));
#23398=CARTESIAN_POINT('Ctrl Pts',(-25.8415089241134,-30.0656638016321,
18.));
#23399=CARTESIAN_POINT('Ctrl Pts',(-25.8779535511028,-30.1563500154165,
0.));
#23400=CARTESIAN_POINT('Ctrl Pts',(-25.8779535511028,-30.1563500154165,
18.));
#23401=CARTESIAN_POINT('Ctrl Pts',(-25.9137466853317,-30.2474530144827,
0.));
#23402=CARTESIAN_POINT('Ctrl Pts',(-25.9137466853317,-30.2474530144827,
18.));
#23403=CARTESIAN_POINT('Ctrl Pts',(-25.9489196635424,-30.3389466074503,
0.));
#23404=CARTESIAN_POINT('Ctrl Pts',(-25.9489196635424,-30.3389466074503,
18.));
#23405=CARTESIAN_POINT('Ctrl Pts',(-25.9834942765902,-30.4308118142473,
0.));
#23406=CARTESIAN_POINT('Ctrl Pts',(-25.9834942765902,-30.4308118142473,
18.));
#23407=CARTESIAN_POINT('Ctrl Pts',(-26.0174801292225,-30.5230388264271,
0.));
#23408=CARTESIAN_POINT('Ctrl Pts',(-26.0174801292225,-30.5230388264271,
18.));
#23409=CARTESIAN_POINT('Ctrl Pts',(-26.0508796503166,-30.6156232634061,
0.));
#23410=CARTESIAN_POINT('Ctrl Pts',(-26.0508796503166,-30.6156232634061,
18.));
#23411=CARTESIAN_POINT('Ctrl Pts',(-26.0836911730968,-30.7085638682391,
0.));
#23412=CARTESIAN_POINT('Ctrl Pts',(-26.0836911730968,-30.7085638682391,
18.));
#23413=CARTESIAN_POINT('Ctrl Pts',(-26.1159125093178,-30.8018598357461,
0.));
#23414=CARTESIAN_POINT('Ctrl Pts',(-26.1159125093178,-30.8018598357461,
18.));
#23415=CARTESIAN_POINT('Ctrl Pts',(-26.1475450294082,-30.8955077633644,
0.));
#23416=CARTESIAN_POINT('Ctrl Pts',(-26.1475450294082,-30.8955077633644,
18.));
#23417=CARTESIAN_POINT('Ctrl Pts',(-26.1785946616165,-30.9895009017073,
0.));
#23418=CARTESIAN_POINT('Ctrl Pts',(-26.1785946616165,-30.9895009017073,
18.));
#23419=CARTESIAN_POINT('Ctrl Pts',(-26.2090698085494,-31.0838307058369,
0.));
#23420=CARTESIAN_POINT('Ctrl Pts',(-26.2090698085494,-31.0838307058369,
18.));
#23421=CARTESIAN_POINT('Ctrl Pts',(-26.2389800738215,-31.1784877826858,
0.));
#23422=CARTESIAN_POINT('Ctrl Pts',(-26.2389800738215,-31.1784877826858,
18.));
#23423=CARTESIAN_POINT('Ctrl Pts',(-26.2683347859175,-31.2734629900041,
0.));
#23424=CARTESIAN_POINT('Ctrl Pts',(-26.2683347859175,-31.2734629900041,
18.));
#23425=CARTESIAN_POINT('Ctrl Pts',(-26.2971413115295,-31.3687486937246,
0.));
#23426=CARTESIAN_POINT('Ctrl Pts',(-26.2971413115295,-31.3687486937246,
18.));
#23427=CARTESIAN_POINT('Ctrl Pts',(-26.3254046890485,-31.4643390378084,
0.));
#23428=CARTESIAN_POINT('Ctrl Pts',(-26.3254046890485,-31.4643390378084,
18.));
#23429=CARTESIAN_POINT('Ctrl Pts',(-26.353128528169,-31.5602292672984,0.));
#23430=CARTESIAN_POINT('Ctrl Pts',(-26.353128528169,-31.5602292672984,18.));
#23431=CARTESIAN_POINT('Ctrl Pts',(-26.3803155790949,-31.6564152990236,
0.));
#23432=CARTESIAN_POINT('Ctrl Pts',(-26.3803155790949,-31.6564152990236,
18.));
#23433=CARTESIAN_POINT('Ctrl Pts',(-26.4069683862785,-31.7528932299312,
0.));
#23434=CARTESIAN_POINT('Ctrl Pts',(-26.4069683862785,-31.7528932299312,
18.));
#23435=CARTESIAN_POINT('Ctrl Pts',(-26.433090040836,-31.849658771403,0.));
#23436=CARTESIAN_POINT('Ctrl Pts',(-26.433090040836,-31.849658771403,18.));
#23437=CARTESIAN_POINT('Ctrl Pts',(-26.4586843683627,-31.9467071093816,
0.));
#23438=CARTESIAN_POINT('Ctrl Pts',(-26.4586843683627,-31.9467071093816,
18.));
#23439=CARTESIAN_POINT('Ctrl Pts',(-26.4837555495616,-32.0440331917233,
0.));
#23440=CARTESIAN_POINT('Ctrl Pts',(-26.4837555495616,-32.0440331917233,
18.));
#23441=CARTESIAN_POINT('Ctrl Pts',(-26.5083078928862,-32.1416319023705,
0.));
#23442=CARTESIAN_POINT('Ctrl Pts',(-26.5083078928862,-32.1416319023705,
18.));
#23443=CARTESIAN_POINT('Ctrl Pts',(-26.5323455701117,-32.2394982626669,
0.));
#23444=CARTESIAN_POINT('Ctrl Pts',(-26.5323455701117,-32.2394982626669,
18.));
#23445=CARTESIAN_POINT('Ctrl Pts',(-26.5558723200361,-32.3376276606981,
0.));
#23446=CARTESIAN_POINT('Ctrl Pts',(-26.5558723200361,-32.3376276606981,
18.));
#23447=CARTESIAN_POINT('Ctrl Pts',(-26.5788913672813,-32.4360159072985,
0.));
#23448=CARTESIAN_POINT('Ctrl Pts',(-26.5788913672813,-32.4360159072985,
18.));
#23449=CARTESIAN_POINT('Ctrl Pts',(-26.6014055904817,-32.5346590925498,
0.));
#23450=CARTESIAN_POINT('Ctrl Pts',(-26.6014055904817,-32.5346590925498,
18.));
#23451=CARTESIAN_POINT('Ctrl Pts',(-26.6234176311245,-32.6335534898935,
0.));
#23452=CARTESIAN_POINT('Ctrl Pts',(-26.6234176311245,-32.6335534898935,
18.));
#23453=CARTESIAN_POINT('Ctrl Pts',(-26.6449300199764,-32.7326954489334,
0.));
#23454=CARTESIAN_POINT('Ctrl Pts',(-26.6449300199764,-32.7326954489334,
18.));
#23455=CARTESIAN_POINT('Ctrl Pts',(-26.6659453236976,-32.8320812678271,
0.));
#23456=CARTESIAN_POINT('Ctrl Pts',(-26.6659453236976,-32.8320812678271,
18.));
#23457=CARTESIAN_POINT('Ctrl Pts',(-26.6864661988935,-32.9317071576181,
0.));
#23458=CARTESIAN_POINT('Ctrl Pts',(-26.6864661988935,-32.9317071576181,
18.));
#23459=CARTESIAN_POINT('Ctrl Pts',(-26.7064953106254,-33.03156933761,0.));
#23460=CARTESIAN_POINT('Ctrl Pts',(-26.7064953106254,-33.03156933761,18.));
#23461=CARTESIAN_POINT('Ctrl Pts',(-26.7260352861619,-33.131664100194,0.));
#23462=CARTESIAN_POINT('Ctrl Pts',(-26.7260352861619,-33.131664100194,18.));
#23463=CARTESIAN_POINT('Ctrl Pts',(-26.7450886617884,-33.2319878786519,
0.));
#23464=CARTESIAN_POINT('Ctrl Pts',(-26.7450886617884,-33.2319878786519,
18.));
#23465=CARTESIAN_POINT('Ctrl Pts',(-26.7636578270526,-33.3325373307046,
0.));
#23466=CARTESIAN_POINT('Ctrl Pts',(-26.7636578270526,-33.3325373307046,
18.));
#23467=CARTESIAN_POINT('Ctrl Pts',(-26.7817450041181,-33.4333093513694,
0.));
#23468=CARTESIAN_POINT('Ctrl Pts',(-26.7817450041181,-33.4333093513694,
18.));
#23469=CARTESIAN_POINT('Ctrl Pts',(-26.7993522966985,-33.5343009499673,
0.));
#23470=CARTESIAN_POINT('Ctrl Pts',(-26.7993522966985,-33.5343009499673,
18.));
#23471=CARTESIAN_POINT('Ctrl Pts',(-26.8164817280846,-33.6355091508895,
0.));
#23472=CARTESIAN_POINT('Ctrl Pts',(-26.8164817280846,-33.6355091508895,
18.));
#23473=CARTESIAN_POINT('Ctrl Pts',(-26.8331352836667,-33.7369308933173,
0.));
#23474=CARTESIAN_POINT('Ctrl Pts',(-26.8331352836667,-33.7369308933173,
18.));
#23475=CARTESIAN_POINT('Ctrl Pts',(-26.8493149627661,-33.838562905895,0.));
#23476=CARTESIAN_POINT('Ctrl Pts',(-26.8493149627661,-33.838562905895,18.));
#23477=CARTESIAN_POINT('Ctrl Pts',(-26.8650228056313,-33.9404016650487,
0.));
#23478=CARTESIAN_POINT('Ctrl Pts',(-26.8650228056313,-33.9404016650487,
18.));
#23479=CARTESIAN_POINT('Ctrl Pts',(-26.880260834701,-34.0424436187397,0.));
#23480=CARTESIAN_POINT('Ctrl Pts',(-26.880260834701,-34.0424436187397,18.));
#23481=CARTESIAN_POINT('Ctrl Pts',(-26.895031013894,-34.1446853651051,0.));
#23482=CARTESIAN_POINT('Ctrl Pts',(-26.895031013894,-34.1446853651051,18.));
#23483=CARTESIAN_POINT('Ctrl Pts',(-26.9093352037262,-34.2471238425419,
0.));
#23484=CARTESIAN_POINT('Ctrl Pts',(-26.9093352037262,-34.2471238425419,
18.));
#23485=CARTESIAN_POINT('Ctrl Pts',(-26.9231751225177,-34.3497565255724,
0.));
#23486=CARTESIAN_POINT('Ctrl Pts',(-26.9231751225177,-34.3497565255724,
18.));
#23487=CARTESIAN_POINT('Ctrl Pts',(-26.9365523054581,-34.4525815829097,
0.));
#23488=CARTESIAN_POINT('Ctrl Pts',(-26.9365523054581,-34.4525815829097,
18.));
#23489=CARTESIAN_POINT('Ctrl Pts',(-26.9494680440307,-34.5555977590573,
0.));
#23490=CARTESIAN_POINT('Ctrl Pts',(-26.9494680440307,-34.5555977590573,
18.));
#23491=CARTESIAN_POINT('Ctrl Pts',(-26.9594322726214,-34.6381629799782,
0.));
#23492=CARTESIAN_POINT('Ctrl Pts',(-26.9594322726214,-34.6381629799782,
18.));
#23493=CARTESIAN_POINT('Ctrl Pts',(-26.9666985267609,-34.700172380686,0.));
#23494=CARTESIAN_POINT('Ctrl Pts',(-26.9666985267609,-34.700172380686,18.));
#23495=CARTESIAN_POINT('Ctrl Pts',(-26.9714507634923,-34.7415499619104,
0.));
#23496=CARTESIAN_POINT('Ctrl Pts',(-26.9714507634923,-34.7415499619104,
18.));
#23497=CARTESIAN_POINT('Ctrl Pts',(-26.9738038986838,-34.7622482477091,
0.));
#23498=CARTESIAN_POINT('Ctrl Pts',(-26.9738038986838,-34.7622482477091,
18.));
#23499=CARTESIAN_POINT('Ctrl Pts',(-24.8345302882955,-28.2149191006268,
0.));
#23500=CARTESIAN_POINT('Ctrl Pts',(-24.8470618363541,-28.2291563988795,
0.));
#23501=CARTESIAN_POINT('Ctrl Pts',(-24.8717258526943,-28.2579420132101,
0.));
#23502=CARTESIAN_POINT('Ctrl Pts',(-24.9075246543798,-28.302053475606,0.));
#23503=CARTESIAN_POINT('Ctrl Pts',(-24.9529811166897,-28.3626431274892,
0.));
#23504=CARTESIAN_POINT('Ctrl Pts',(-25.0066999111736,-28.4408053900206,
0.));
#23505=CARTESIAN_POINT('Ctrl Pts',(-25.0581926620043,-28.5207164321473,
0.));
#23506=CARTESIAN_POINT('Ctrl Pts',(-25.108321158239,-28.6017081342376,0.));
#23507=CARTESIAN_POINT('Ctrl Pts',(-25.1577170374459,-28.6832861366762,
0.));
#23508=CARTESIAN_POINT('Ctrl Pts',(-25.2066127148845,-28.7652594076549,
0.));
#23509=CARTESIAN_POINT('Ctrl Pts',(-25.2549775629725,-28.8476372998748,
0.));
#23510=CARTESIAN_POINT('Ctrl Pts',(-25.3026235249214,-28.9305499160476,
0.));
#23511=CARTESIAN_POINT('Ctrl Pts',(-25.3493168206005,-29.0141637699076,
0.));
#23512=CARTESIAN_POINT('Ctrl Pts',(-25.3948997321279,-29.098589927237,0.));
#23513=CARTESIAN_POINT('Ctrl Pts',(-25.4393679214513,-29.183825549991,0.));
#23514=CARTESIAN_POINT('Ctrl Pts',(-25.4828076101654,-29.2698007967907,
0.));
#23515=CARTESIAN_POINT('Ctrl Pts',(-25.5253562922582,-29.356408021119,0.));
#23516=CARTESIAN_POINT('Ctrl Pts',(-25.5671572096726,-29.443535683207,0.));
#23517=CARTESIAN_POINT('Ctrl Pts',(-25.6083094352667,-29.5311055094509,
0.));
#23518=CARTESIAN_POINT('Ctrl Pts',(-25.6488438125835,-29.6190903904157,
0.));
#23519=CARTESIAN_POINT('Ctrl Pts',(-25.6887507922748,-29.7074935910931,
0.));
#23520=CARTESIAN_POINT('Ctrl Pts',(-25.7279973711305,-29.7963360859334,
0.));
#23521=CARTESIAN_POINT('Ctrl Pts',(-25.7665469042913,-29.8856417535786,
0.));
#23522=CARTESIAN_POINT('Ctrl Pts',(-25.8043812318215,-29.9754208429384,
0.));
#23523=CARTESIAN_POINT('Ctrl Pts',(-25.8415089241134,-30.0656638016321,
0.));
#23524=CARTESIAN_POINT('Ctrl Pts',(-25.8779535511028,-30.1563500154165,
0.));
#23525=CARTESIAN_POINT('Ctrl Pts',(-25.9137466853317,-30.2474530144827,
0.));
#23526=CARTESIAN_POINT('Ctrl Pts',(-25.9489196635424,-30.3389466074503,
0.));
#23527=CARTESIAN_POINT('Ctrl Pts',(-25.9834942765902,-30.4308118142473,
0.));
#23528=CARTESIAN_POINT('Ctrl Pts',(-26.0174801292225,-30.5230388264271,
0.));
#23529=CARTESIAN_POINT('Ctrl Pts',(-26.0508796503166,-30.6156232634061,
0.));
#23530=CARTESIAN_POINT('Ctrl Pts',(-26.0836911730968,-30.7085638682391,
0.));
#23531=CARTESIAN_POINT('Ctrl Pts',(-26.1159125093178,-30.8018598357461,
0.));
#23532=CARTESIAN_POINT('Ctrl Pts',(-26.1475450294082,-30.8955077633644,
0.));
#23533=CARTESIAN_POINT('Ctrl Pts',(-26.1785946616165,-30.9895009017073,
0.));
#23534=CARTESIAN_POINT('Ctrl Pts',(-26.2090698085494,-31.0838307058369,
0.));
#23535=CARTESIAN_POINT('Ctrl Pts',(-26.2389800738215,-31.1784877826858,
0.));
#23536=CARTESIAN_POINT('Ctrl Pts',(-26.2683347859175,-31.2734629900041,
0.));
#23537=CARTESIAN_POINT('Ctrl Pts',(-26.2971413115295,-31.3687486937246,
0.));
#23538=CARTESIAN_POINT('Ctrl Pts',(-26.3254046890485,-31.4643390378084,
0.));
#23539=CARTESIAN_POINT('Ctrl Pts',(-26.353128528169,-31.5602292672984,0.));
#23540=CARTESIAN_POINT('Ctrl Pts',(-26.3803155790949,-31.6564152990236,
0.));
#23541=CARTESIAN_POINT('Ctrl Pts',(-26.4069683862785,-31.7528932299312,
0.));
#23542=CARTESIAN_POINT('Ctrl Pts',(-26.433090040836,-31.849658771403,0.));
#23543=CARTESIAN_POINT('Ctrl Pts',(-26.4586843683627,-31.9467071093816,
0.));
#23544=CARTESIAN_POINT('Ctrl Pts',(-26.4837555495616,-32.0440331917233,
0.));
#23545=CARTESIAN_POINT('Ctrl Pts',(-26.5083078928862,-32.1416319023705,
0.));
#23546=CARTESIAN_POINT('Ctrl Pts',(-26.5323455701117,-32.2394982626669,
0.));
#23547=CARTESIAN_POINT('Ctrl Pts',(-26.5558723200361,-32.3376276606981,
0.));
#23548=CARTESIAN_POINT('Ctrl Pts',(-26.5788913672813,-32.4360159072985,
0.));
#23549=CARTESIAN_POINT('Ctrl Pts',(-26.6014055904817,-32.5346590925498,
0.));
#23550=CARTESIAN_POINT('Ctrl Pts',(-26.6234176311245,-32.6335534898935,
0.));
#23551=CARTESIAN_POINT('Ctrl Pts',(-26.6449300199764,-32.7326954489334,
0.));
#23552=CARTESIAN_POINT('Ctrl Pts',(-26.6659453236976,-32.8320812678271,
0.));
#23553=CARTESIAN_POINT('Ctrl Pts',(-26.6864661988935,-32.9317071576181,
0.));
#23554=CARTESIAN_POINT('Ctrl Pts',(-26.7064953106254,-33.03156933761,0.));
#23555=CARTESIAN_POINT('Ctrl Pts',(-26.7260352861619,-33.131664100194,0.));
#23556=CARTESIAN_POINT('Ctrl Pts',(-26.7450886617884,-33.2319878786519,
0.));
#23557=CARTESIAN_POINT('Ctrl Pts',(-26.7636578270526,-33.3325373307046,
0.));
#23558=CARTESIAN_POINT('Ctrl Pts',(-26.7817450041181,-33.4333093513694,
0.));
#23559=CARTESIAN_POINT('Ctrl Pts',(-26.7993522966985,-33.5343009499673,
0.));
#23560=CARTESIAN_POINT('Ctrl Pts',(-26.8164817280846,-33.6355091508895,
0.));
#23561=CARTESIAN_POINT('Ctrl Pts',(-26.8331352836667,-33.7369308933173,
0.));
#23562=CARTESIAN_POINT('Ctrl Pts',(-26.8493149627661,-33.838562905895,0.));
#23563=CARTESIAN_POINT('Ctrl Pts',(-26.8650228056313,-33.9404016650487,
0.));
#23564=CARTESIAN_POINT('Ctrl Pts',(-26.880260834701,-34.0424436187397,0.));
#23565=CARTESIAN_POINT('Ctrl Pts',(-26.895031013894,-34.1446853651051,0.));
#23566=CARTESIAN_POINT('Ctrl Pts',(-26.9093352037262,-34.2471238425419,
0.));
#23567=CARTESIAN_POINT('Ctrl Pts',(-26.9231751225177,-34.3497565255724,
0.));
#23568=CARTESIAN_POINT('Ctrl Pts',(-26.9392277420462,-34.4731465943772,
0.));
#23569=CARTESIAN_POINT('Ctrl Pts',(-26.9520281195268,-34.5762105502273,
0.));
#23570=CARTESIAN_POINT('Ctrl Pts',(-26.9619003236529,-34.6588137898952,
0.));
#23571=CARTESIAN_POINT('Ctrl Pts',(-26.9690976283149,-34.7208516760814,
0.));
#23572=CARTESIAN_POINT('Ctrl Pts',(-26.9738038986838,-34.7622482477091,
0.));
#23573=CARTESIAN_POINT('Ctrl Pts',(-24.8345302882955,-28.2149191006268,
15.));
#23574=CARTESIAN_POINT('Ctrl Pts',(-24.8470618363541,-28.2291563988795,
15.));
#23575=CARTESIAN_POINT('Ctrl Pts',(-24.8717258526943,-28.2579420132101,
15.));
#23576=CARTESIAN_POINT('Ctrl Pts',(-24.9075246543798,-28.302053475606,15.));
#23577=CARTESIAN_POINT('Ctrl Pts',(-24.9529811166897,-28.3626431274892,
15.));
#23578=CARTESIAN_POINT('Ctrl Pts',(-25.0066999111736,-28.4408053900206,
15.));
#23579=CARTESIAN_POINT('Ctrl Pts',(-25.0581926620043,-28.5207164321473,
15.));
#23580=CARTESIAN_POINT('Ctrl Pts',(-25.108321158239,-28.6017081342376,15.));
#23581=CARTESIAN_POINT('Ctrl Pts',(-25.1577170374459,-28.6832861366762,
15.));
#23582=CARTESIAN_POINT('Ctrl Pts',(-25.2066127148845,-28.7652594076549,
15.));
#23583=CARTESIAN_POINT('Ctrl Pts',(-25.2549775629725,-28.8476372998748,
15.));
#23584=CARTESIAN_POINT('Ctrl Pts',(-25.3026235249214,-28.9305499160476,
15.));
#23585=CARTESIAN_POINT('Ctrl Pts',(-25.3493168206005,-29.0141637699076,
15.));
#23586=CARTESIAN_POINT('Ctrl Pts',(-25.3948997321279,-29.098589927237,15.));
#23587=CARTESIAN_POINT('Ctrl Pts',(-25.4393679214513,-29.183825549991,15.));
#23588=CARTESIAN_POINT('Ctrl Pts',(-25.4828076101654,-29.2698007967907,
15.));
#23589=CARTESIAN_POINT('Ctrl Pts',(-25.5253562922582,-29.356408021119,15.));
#23590=CARTESIAN_POINT('Ctrl Pts',(-25.5671572096726,-29.443535683207,15.));
#23591=CARTESIAN_POINT('Ctrl Pts',(-25.6083094352667,-29.5311055094509,
15.));
#23592=CARTESIAN_POINT('Ctrl Pts',(-25.6488438125835,-29.6190903904157,
15.));
#23593=CARTESIAN_POINT('Ctrl Pts',(-25.6887507922748,-29.7074935910931,
15.));
#23594=CARTESIAN_POINT('Ctrl Pts',(-25.7279973711305,-29.7963360859334,
15.));
#23595=CARTESIAN_POINT('Ctrl Pts',(-25.7665469042913,-29.8856417535786,
15.));
#23596=CARTESIAN_POINT('Ctrl Pts',(-25.8043812318215,-29.9754208429384,
15.));
#23597=CARTESIAN_POINT('Ctrl Pts',(-25.8415089241134,-30.0656638016321,
15.));
#23598=CARTESIAN_POINT('Ctrl Pts',(-25.8779535511028,-30.1563500154165,
15.));
#23599=CARTESIAN_POINT('Ctrl Pts',(-25.9137466853317,-30.2474530144827,
15.));
#23600=CARTESIAN_POINT('Ctrl Pts',(-25.9489196635424,-30.3389466074503,
15.));
#23601=CARTESIAN_POINT('Ctrl Pts',(-25.9834942765902,-30.4308118142473,
15.));
#23602=CARTESIAN_POINT('Ctrl Pts',(-26.0174801292225,-30.5230388264271,
15.));
#23603=CARTESIAN_POINT('Ctrl Pts',(-26.0508796503166,-30.6156232634061,
15.));
#23604=CARTESIAN_POINT('Ctrl Pts',(-26.0836911730968,-30.7085638682391,
15.));
#23605=CARTESIAN_POINT('Ctrl Pts',(-26.1159125093178,-30.8018598357461,
15.));
#23606=CARTESIAN_POINT('Ctrl Pts',(-26.1475450294082,-30.8955077633644,
15.));
#23607=CARTESIAN_POINT('Ctrl Pts',(-26.1785946616165,-30.9895009017073,
15.));
#23608=CARTESIAN_POINT('Ctrl Pts',(-26.2090698085494,-31.0838307058369,
15.));
#23609=CARTESIAN_POINT('Ctrl Pts',(-26.2389800738215,-31.1784877826858,
15.));
#23610=CARTESIAN_POINT('Ctrl Pts',(-26.2683347859175,-31.2734629900041,
15.));
#23611=CARTESIAN_POINT('Ctrl Pts',(-26.2971413115295,-31.3687486937246,
15.));
#23612=CARTESIAN_POINT('Ctrl Pts',(-26.3254046890485,-31.4643390378084,
15.));
#23613=CARTESIAN_POINT('Ctrl Pts',(-26.353128528169,-31.5602292672984,15.));
#23614=CARTESIAN_POINT('Ctrl Pts',(-26.3803155790949,-31.6564152990236,
15.));
#23615=CARTESIAN_POINT('Ctrl Pts',(-26.4069683862785,-31.7528932299312,
15.));
#23616=CARTESIAN_POINT('Ctrl Pts',(-26.433090040836,-31.849658771403,15.));
#23617=CARTESIAN_POINT('Ctrl Pts',(-26.4586843683627,-31.9467071093816,
15.));
#23618=CARTESIAN_POINT('Ctrl Pts',(-26.4837555495616,-32.0440331917233,
15.));
#23619=CARTESIAN_POINT('Ctrl Pts',(-26.5083078928862,-32.1416319023705,
15.));
#23620=CARTESIAN_POINT('Ctrl Pts',(-26.5323455701117,-32.2394982626669,
15.));
#23621=CARTESIAN_POINT('Ctrl Pts',(-26.5558723200361,-32.3376276606981,
15.));
#23622=CARTESIAN_POINT('Ctrl Pts',(-26.5788913672813,-32.4360159072985,
15.));
#23623=CARTESIAN_POINT('Ctrl Pts',(-26.6014055904817,-32.5346590925498,
15.));
#23624=CARTESIAN_POINT('Ctrl Pts',(-26.6234176311245,-32.6335534898935,
15.));
#23625=CARTESIAN_POINT('Ctrl Pts',(-26.6449300199764,-32.7326954489334,
15.));
#23626=CARTESIAN_POINT('Ctrl Pts',(-26.6659453236976,-32.8320812678271,
15.));
#23627=CARTESIAN_POINT('Ctrl Pts',(-26.6864661988935,-32.9317071576181,
15.));
#23628=CARTESIAN_POINT('Ctrl Pts',(-26.7064953106254,-33.03156933761,15.));
#23629=CARTESIAN_POINT('Ctrl Pts',(-26.7260352861619,-33.131664100194,15.));
#23630=CARTESIAN_POINT('Ctrl Pts',(-26.7450886617884,-33.2319878786519,
15.));
#23631=CARTESIAN_POINT('Ctrl Pts',(-26.7636578270526,-33.3325373307046,
15.));
#23632=CARTESIAN_POINT('Ctrl Pts',(-26.7817450041181,-33.4333093513694,
15.));
#23633=CARTESIAN_POINT('Ctrl Pts',(-26.7993522966985,-33.5343009499673,
15.));
#23634=CARTESIAN_POINT('Ctrl Pts',(-26.8164817280846,-33.6355091508895,
15.));
#23635=CARTESIAN_POINT('Ctrl Pts',(-26.8331352836667,-33.7369308933173,
15.));
#23636=CARTESIAN_POINT('Ctrl Pts',(-26.8493149627661,-33.838562905895,15.));
#23637=CARTESIAN_POINT('Ctrl Pts',(-26.8650228056313,-33.9404016650487,
15.));
#23638=CARTESIAN_POINT('Ctrl Pts',(-26.880260834701,-34.0424436187397,15.));
#23639=CARTESIAN_POINT('Ctrl Pts',(-26.895031013894,-34.1446853651051,15.));
#23640=CARTESIAN_POINT('Ctrl Pts',(-26.9093352037262,-34.2471238425419,
15.));
#23641=CARTESIAN_POINT('Ctrl Pts',(-26.9231751225177,-34.3497565255724,
15.));
#23642=CARTESIAN_POINT('Ctrl Pts',(-26.9392277420462,-34.4731465943772,
15.));
#23643=CARTESIAN_POINT('Ctrl Pts',(-26.9520281195268,-34.5762105502273,
15.));
#23644=CARTESIAN_POINT('Ctrl Pts',(-26.9619003236529,-34.6588137898952,
15.));
#23645=CARTESIAN_POINT('Ctrl Pts',(-26.9690976283149,-34.7208516760814,
15.));
#23646=CARTESIAN_POINT('Ctrl Pts',(-26.9738038986838,-34.7622482477091,
15.));
#23647=CARTESIAN_POINT('Ctrl Pts',(-34.7622482477091,-26.9738038986838,
0.));
#23648=CARTESIAN_POINT('Ctrl Pts',(-34.7622482477091,-26.9738038986838,
18.));
#23649=CARTESIAN_POINT('Ctrl Pts',(-34.7415499619104,-26.9714507634923,
0.));
#23650=CARTESIAN_POINT('Ctrl Pts',(-34.7415499619104,-26.9714507634923,
18.));
#23651=CARTESIAN_POINT('Ctrl Pts',(-34.700172380686,-26.9666985267608,0.));
#23652=CARTESIAN_POINT('Ctrl Pts',(-34.700172380686,-26.9666985267608,18.));
#23653=CARTESIAN_POINT('Ctrl Pts',(-34.6381629799782,-26.9594322726214,
0.));
#23654=CARTESIAN_POINT('Ctrl Pts',(-34.6381629799782,-26.9594322726214,
18.));
#23655=CARTESIAN_POINT('Ctrl Pts',(-34.5555977590573,-26.9494680440307,
0.));
#23656=CARTESIAN_POINT('Ctrl Pts',(-34.5555977590573,-26.9494680440307,
18.));
#23657=CARTESIAN_POINT('Ctrl Pts',(-34.4525815829097,-26.9365523054581,
0.));
#23658=CARTESIAN_POINT('Ctrl Pts',(-34.4525815829097,-26.9365523054581,
18.));
#23659=CARTESIAN_POINT('Ctrl Pts',(-34.3497565255724,-26.9231751225177,
0.));
#23660=CARTESIAN_POINT('Ctrl Pts',(-34.3497565255724,-26.9231751225177,
18.));
#23661=CARTESIAN_POINT('Ctrl Pts',(-34.2471238425419,-26.9093352037262,
0.));
#23662=CARTESIAN_POINT('Ctrl Pts',(-34.2471238425419,-26.9093352037262,
18.));
#23663=CARTESIAN_POINT('Ctrl Pts',(-34.1446853651051,-26.8950310138939,
0.));
#23664=CARTESIAN_POINT('Ctrl Pts',(-34.1446853651051,-26.8950310138939,
18.));
#23665=CARTESIAN_POINT('Ctrl Pts',(-34.0424436187397,-26.880260834701,0.));
#23666=CARTESIAN_POINT('Ctrl Pts',(-34.0424436187397,-26.880260834701,18.));
#23667=CARTESIAN_POINT('Ctrl Pts',(-33.9404016650487,-26.8650228056313,
0.));
#23668=CARTESIAN_POINT('Ctrl Pts',(-33.9404016650487,-26.8650228056313,
18.));
#23669=CARTESIAN_POINT('Ctrl Pts',(-33.838562905895,-26.8493149627661,0.));
#23670=CARTESIAN_POINT('Ctrl Pts',(-33.838562905895,-26.8493149627661,18.));
#23671=CARTESIAN_POINT('Ctrl Pts',(-33.7369308933173,-26.8331352836666,
0.));
#23672=CARTESIAN_POINT('Ctrl Pts',(-33.7369308933173,-26.8331352836666,
18.));
#23673=CARTESIAN_POINT('Ctrl Pts',(-33.6355091508895,-26.8164817280846,
0.));
#23674=CARTESIAN_POINT('Ctrl Pts',(-33.6355091508895,-26.8164817280846,
18.));
#23675=CARTESIAN_POINT('Ctrl Pts',(-33.5343009499673,-26.7993522966985,
0.));
#23676=CARTESIAN_POINT('Ctrl Pts',(-33.5343009499673,-26.7993522966985,
18.));
#23677=CARTESIAN_POINT('Ctrl Pts',(-33.4333093513694,-26.7817450041181,
0.));
#23678=CARTESIAN_POINT('Ctrl Pts',(-33.4333093513694,-26.7817450041181,
18.));
#23679=CARTESIAN_POINT('Ctrl Pts',(-33.3325373307046,-26.7636578270526,
0.));
#23680=CARTESIAN_POINT('Ctrl Pts',(-33.3325373307046,-26.7636578270526,
18.));
#23681=CARTESIAN_POINT('Ctrl Pts',(-33.2319878786519,-26.7450886617884,
0.));
#23682=CARTESIAN_POINT('Ctrl Pts',(-33.2319878786519,-26.7450886617884,
18.));
#23683=CARTESIAN_POINT('Ctrl Pts',(-33.131664100194,-26.7260352861619,0.));
#23684=CARTESIAN_POINT('Ctrl Pts',(-33.131664100194,-26.7260352861619,18.));
#23685=CARTESIAN_POINT('Ctrl Pts',(-33.03156933761,-26.7064953106254,0.));
#23686=CARTESIAN_POINT('Ctrl Pts',(-33.03156933761,-26.7064953106254,18.));
#23687=CARTESIAN_POINT('Ctrl Pts',(-32.9317071576181,-26.6864661988935,
0.));
#23688=CARTESIAN_POINT('Ctrl Pts',(-32.9317071576181,-26.6864661988935,
18.));
#23689=CARTESIAN_POINT('Ctrl Pts',(-32.8320812678271,-26.6659453236976,
0.));
#23690=CARTESIAN_POINT('Ctrl Pts',(-32.8320812678271,-26.6659453236976,
18.));
#23691=CARTESIAN_POINT('Ctrl Pts',(-32.7326954489334,-26.6449300199763,
0.));
#23692=CARTESIAN_POINT('Ctrl Pts',(-32.7326954489334,-26.6449300199763,
18.));
#23693=CARTESIAN_POINT('Ctrl Pts',(-32.6335534898936,-26.6234176311245,
0.));
#23694=CARTESIAN_POINT('Ctrl Pts',(-32.6335534898936,-26.6234176311245,
18.));
#23695=CARTESIAN_POINT('Ctrl Pts',(-32.5346590925498,-26.6014055904817,
0.));
#23696=CARTESIAN_POINT('Ctrl Pts',(-32.5346590925498,-26.6014055904817,
18.));
#23697=CARTESIAN_POINT('Ctrl Pts',(-32.4360159072985,-26.5788913672813,
0.));
#23698=CARTESIAN_POINT('Ctrl Pts',(-32.4360159072985,-26.5788913672813,
18.));
#23699=CARTESIAN_POINT('Ctrl Pts',(-32.3376276606981,-26.5558723200361,
0.));
#23700=CARTESIAN_POINT('Ctrl Pts',(-32.3376276606981,-26.5558723200361,
18.));
#23701=CARTESIAN_POINT('Ctrl Pts',(-32.2394982626669,-26.5323455701117,
0.));
#23702=CARTESIAN_POINT('Ctrl Pts',(-32.2394982626669,-26.5323455701117,
18.));
#23703=CARTESIAN_POINT('Ctrl Pts',(-32.1416319023705,-26.5083078928862,
0.));
#23704=CARTESIAN_POINT('Ctrl Pts',(-32.1416319023705,-26.5083078928862,
18.));
#23705=CARTESIAN_POINT('Ctrl Pts',(-32.0440331917233,-26.4837555495616,
0.));
#23706=CARTESIAN_POINT('Ctrl Pts',(-32.0440331917233,-26.4837555495616,
18.));
#23707=CARTESIAN_POINT('Ctrl Pts',(-31.9467071093816,-26.4586843683627,
0.));
#23708=CARTESIAN_POINT('Ctrl Pts',(-31.9467071093816,-26.4586843683627,
18.));
#23709=CARTESIAN_POINT('Ctrl Pts',(-31.849658771403,-26.433090040836,0.));
#23710=CARTESIAN_POINT('Ctrl Pts',(-31.849658771403,-26.433090040836,18.));
#23711=CARTESIAN_POINT('Ctrl Pts',(-31.7528932299312,-26.4069683862784,
0.));
#23712=CARTESIAN_POINT('Ctrl Pts',(-31.7528932299312,-26.4069683862784,
18.));
#23713=CARTESIAN_POINT('Ctrl Pts',(-31.6564152990236,-26.3803155790949,
0.));
#23714=CARTESIAN_POINT('Ctrl Pts',(-31.6564152990236,-26.3803155790949,
18.));
#23715=CARTESIAN_POINT('Ctrl Pts',(-31.5602292672984,-26.353128528169,0.));
#23716=CARTESIAN_POINT('Ctrl Pts',(-31.5602292672984,-26.353128528169,18.));
#23717=CARTESIAN_POINT('Ctrl Pts',(-31.4643390378084,-26.3254046890485,
0.));
#23718=CARTESIAN_POINT('Ctrl Pts',(-31.4643390378084,-26.3254046890485,
18.));
#23719=CARTESIAN_POINT('Ctrl Pts',(-31.3687486937246,-26.2971413115295,
0.));
#23720=CARTESIAN_POINT('Ctrl Pts',(-31.3687486937246,-26.2971413115295,
18.));
#23721=CARTESIAN_POINT('Ctrl Pts',(-31.2734629900041,-26.2683347859175,
0.));
#23722=CARTESIAN_POINT('Ctrl Pts',(-31.2734629900041,-26.2683347859175,
18.));
#23723=CARTESIAN_POINT('Ctrl Pts',(-31.1784877826858,-26.2389800738215,
0.));
#23724=CARTESIAN_POINT('Ctrl Pts',(-31.1784877826858,-26.2389800738215,
18.));
#23725=CARTESIAN_POINT('Ctrl Pts',(-31.0838307058369,-26.2090698085494,
0.));
#23726=CARTESIAN_POINT('Ctrl Pts',(-31.0838307058369,-26.2090698085494,
18.));
#23727=CARTESIAN_POINT('Ctrl Pts',(-30.9895009017073,-26.1785946616165,
0.));
#23728=CARTESIAN_POINT('Ctrl Pts',(-30.9895009017073,-26.1785946616165,
18.));
#23729=CARTESIAN_POINT('Ctrl Pts',(-30.8955077633644,-26.1475450294082,
0.));
#23730=CARTESIAN_POINT('Ctrl Pts',(-30.8955077633644,-26.1475450294082,
18.));
#23731=CARTESIAN_POINT('Ctrl Pts',(-30.8018598357461,-26.1159125093178,
0.));
#23732=CARTESIAN_POINT('Ctrl Pts',(-30.8018598357461,-26.1159125093178,
18.));
#23733=CARTESIAN_POINT('Ctrl Pts',(-30.7085638682391,-26.0836911730968,
0.));
#23734=CARTESIAN_POINT('Ctrl Pts',(-30.7085638682391,-26.0836911730968,
18.));
#23735=CARTESIAN_POINT('Ctrl Pts',(-30.6156232634061,-26.0508796503166,
0.));
#23736=CARTESIAN_POINT('Ctrl Pts',(-30.6156232634061,-26.0508796503166,
18.));
#23737=CARTESIAN_POINT('Ctrl Pts',(-30.5230388264271,-26.0174801292225,
0.));
#23738=CARTESIAN_POINT('Ctrl Pts',(-30.5230388264271,-26.0174801292225,
18.));
#23739=CARTESIAN_POINT('Ctrl Pts',(-30.4308118142473,-25.9834942765902,
0.));
#23740=CARTESIAN_POINT('Ctrl Pts',(-30.4308118142473,-25.9834942765902,
18.));
#23741=CARTESIAN_POINT('Ctrl Pts',(-30.3389466074503,-25.9489196635424,
0.));
#23742=CARTESIAN_POINT('Ctrl Pts',(-30.3389466074503,-25.9489196635424,
18.));
#23743=CARTESIAN_POINT('Ctrl Pts',(-30.2474530144827,-25.9137466853317,
0.));
#23744=CARTESIAN_POINT('Ctrl Pts',(-30.2474530144827,-25.9137466853317,
18.));
#23745=CARTESIAN_POINT('Ctrl Pts',(-30.1563500154165,-25.8779535511027,
0.));
#23746=CARTESIAN_POINT('Ctrl Pts',(-30.1563500154165,-25.8779535511027,
18.));
#23747=CARTESIAN_POINT('Ctrl Pts',(-30.0656638016321,-25.8415089241134,
0.));
#23748=CARTESIAN_POINT('Ctrl Pts',(-30.0656638016321,-25.8415089241134,
18.));
#23749=CARTESIAN_POINT('Ctrl Pts',(-29.9754208429384,-25.8043812318214,
0.));
#23750=CARTESIAN_POINT('Ctrl Pts',(-29.9754208429384,-25.8043812318214,
18.));
#23751=CARTESIAN_POINT('Ctrl Pts',(-29.8856417535786,-25.7665469042913,
0.));
#23752=CARTESIAN_POINT('Ctrl Pts',(-29.8856417535786,-25.7665469042913,
18.));
#23753=CARTESIAN_POINT('Ctrl Pts',(-29.7963360859334,-25.7279973711305,
0.));
#23754=CARTESIAN_POINT('Ctrl Pts',(-29.7963360859334,-25.7279973711305,
18.));
#23755=CARTESIAN_POINT('Ctrl Pts',(-29.7074935910931,-25.6887507922748,
0.));
#23756=CARTESIAN_POINT('Ctrl Pts',(-29.7074935910931,-25.6887507922748,
18.));
#23757=CARTESIAN_POINT('Ctrl Pts',(-29.6190903904157,-25.6488438125835,
0.));
#23758=CARTESIAN_POINT('Ctrl Pts',(-29.6190903904157,-25.6488438125835,
18.));
#23759=CARTESIAN_POINT('Ctrl Pts',(-29.5311055094509,-25.6083094352667,
0.));
#23760=CARTESIAN_POINT('Ctrl Pts',(-29.5311055094509,-25.6083094352667,
18.));
#23761=CARTESIAN_POINT('Ctrl Pts',(-29.443535683207,-25.5671572096726,0.));
#23762=CARTESIAN_POINT('Ctrl Pts',(-29.443535683207,-25.5671572096726,18.));
#23763=CARTESIAN_POINT('Ctrl Pts',(-29.356408021119,-25.5253562922582,0.));
#23764=CARTESIAN_POINT('Ctrl Pts',(-29.356408021119,-25.5253562922582,18.));
#23765=CARTESIAN_POINT('Ctrl Pts',(-29.2698007967907,-25.4828076101654,
0.));
#23766=CARTESIAN_POINT('Ctrl Pts',(-29.2698007967907,-25.4828076101654,
18.));
#23767=CARTESIAN_POINT('Ctrl Pts',(-29.183825549991,-25.4393679214513,0.));
#23768=CARTESIAN_POINT('Ctrl Pts',(-29.183825549991,-25.4393679214513,18.));
#23769=CARTESIAN_POINT('Ctrl Pts',(-29.098589927237,-25.3948997321279,0.));
#23770=CARTESIAN_POINT('Ctrl Pts',(-29.098589927237,-25.3948997321279,18.));
#23771=CARTESIAN_POINT('Ctrl Pts',(-29.0141637699076,-25.3493168206005,
0.));
#23772=CARTESIAN_POINT('Ctrl Pts',(-29.0141637699076,-25.3493168206005,
18.));
#23773=CARTESIAN_POINT('Ctrl Pts',(-28.9305499160476,-25.3026235249214,
0.));
#23774=CARTESIAN_POINT('Ctrl Pts',(-28.9305499160476,-25.3026235249214,
18.));
#23775=CARTESIAN_POINT('Ctrl Pts',(-28.8476372998748,-25.2549775629725,
0.));
#23776=CARTESIAN_POINT('Ctrl Pts',(-28.8476372998748,-25.2549775629725,
18.));
#23777=CARTESIAN_POINT('Ctrl Pts',(-28.7652594076549,-25.2066127148845,
0.));
#23778=CARTESIAN_POINT('Ctrl Pts',(-28.7652594076549,-25.2066127148845,
18.));
#23779=CARTESIAN_POINT('Ctrl Pts',(-28.6832861366762,-25.1577170374459,
0.));
#23780=CARTESIAN_POINT('Ctrl Pts',(-28.6832861366762,-25.1577170374459,
18.));
#23781=CARTESIAN_POINT('Ctrl Pts',(-28.6017081342376,-25.108321158239,0.));
#23782=CARTESIAN_POINT('Ctrl Pts',(-28.6017081342376,-25.108321158239,18.));
#23783=CARTESIAN_POINT('Ctrl Pts',(-28.5207164321473,-25.0581926620043,
0.));
#23784=CARTESIAN_POINT('Ctrl Pts',(-28.5207164321473,-25.0581926620043,
18.));
#23785=CARTESIAN_POINT('Ctrl Pts',(-28.4408053900206,-25.0066999111736,
0.));
#23786=CARTESIAN_POINT('Ctrl Pts',(-28.4408053900206,-25.0066999111736,
18.));
#23787=CARTESIAN_POINT('Ctrl Pts',(-28.3626431274892,-24.9529811166897,
0.));
#23788=CARTESIAN_POINT('Ctrl Pts',(-28.3626431274892,-24.9529811166897,
18.));
#23789=CARTESIAN_POINT('Ctrl Pts',(-28.3020534756061,-24.9075246543798,
0.));
#23790=CARTESIAN_POINT('Ctrl Pts',(-28.3020534756061,-24.9075246543798,
18.));
#23791=CARTESIAN_POINT('Ctrl Pts',(-28.2579420132101,-24.8717258526943,
0.));
#23792=CARTESIAN_POINT('Ctrl Pts',(-28.2579420132101,-24.8717258526943,
18.));
#23793=CARTESIAN_POINT('Ctrl Pts',(-28.2291563988796,-24.8470618363541,
0.));
#23794=CARTESIAN_POINT('Ctrl Pts',(-28.2291563988796,-24.8470618363541,
18.));
#23795=CARTESIAN_POINT('Ctrl Pts',(-28.2149191006269,-24.8345302882955,
0.));
#23796=CARTESIAN_POINT('Ctrl Pts',(-28.2149191006269,-24.8345302882955,
18.));
#23797=CARTESIAN_POINT('',(-34.762248247709,-26.9738038986839,0.));
#23798=CARTESIAN_POINT('Ctrl Pts',(-28.2149191006269,-24.8345302882955,
0.));
#23799=CARTESIAN_POINT('Ctrl Pts',(-28.2291563988796,-24.8470618363541,
0.));
#23800=CARTESIAN_POINT('Ctrl Pts',(-28.2579420132101,-24.8717258526943,
0.));
#23801=CARTESIAN_POINT('Ctrl Pts',(-28.3020534756061,-24.9075246543798,
0.));
#23802=CARTESIAN_POINT('Ctrl Pts',(-28.3626431274892,-24.9529811166897,
0.));
#23803=CARTESIAN_POINT('Ctrl Pts',(-28.4408053900206,-25.0066999111736,
0.));
#23804=CARTESIAN_POINT('Ctrl Pts',(-28.5207164321473,-25.0581926620043,
0.));
#23805=CARTESIAN_POINT('Ctrl Pts',(-28.6017081342376,-25.108321158239,0.));
#23806=CARTESIAN_POINT('Ctrl Pts',(-28.6832861366762,-25.1577170374459,
0.));
#23807=CARTESIAN_POINT('Ctrl Pts',(-28.7652594076549,-25.2066127148845,
0.));
#23808=CARTESIAN_POINT('Ctrl Pts',(-28.8476372998748,-25.2549775629725,
0.));
#23809=CARTESIAN_POINT('Ctrl Pts',(-28.9305499160476,-25.3026235249214,
0.));
#23810=CARTESIAN_POINT('Ctrl Pts',(-29.0141637699076,-25.3493168206005,
0.));
#23811=CARTESIAN_POINT('Ctrl Pts',(-29.098589927237,-25.3948997321279,0.));
#23812=CARTESIAN_POINT('Ctrl Pts',(-29.183825549991,-25.4393679214513,0.));
#23813=CARTESIAN_POINT('Ctrl Pts',(-29.2698007967907,-25.4828076101654,
0.));
#23814=CARTESIAN_POINT('Ctrl Pts',(-29.356408021119,-25.5253562922582,0.));
#23815=CARTESIAN_POINT('Ctrl Pts',(-29.443535683207,-25.5671572096726,0.));
#23816=CARTESIAN_POINT('Ctrl Pts',(-29.5311055094509,-25.6083094352667,
0.));
#23817=CARTESIAN_POINT('Ctrl Pts',(-29.6190903904157,-25.6488438125835,
0.));
#23818=CARTESIAN_POINT('Ctrl Pts',(-29.7074935910931,-25.6887507922748,
0.));
#23819=CARTESIAN_POINT('Ctrl Pts',(-29.7963360859334,-25.7279973711305,
0.));
#23820=CARTESIAN_POINT('Ctrl Pts',(-29.8856417535786,-25.7665469042913,
0.));
#23821=CARTESIAN_POINT('Ctrl Pts',(-29.9754208429384,-25.8043812318214,
0.));
#23822=CARTESIAN_POINT('Ctrl Pts',(-30.0656638016321,-25.8415089241134,
0.));
#23823=CARTESIAN_POINT('Ctrl Pts',(-30.1563500154165,-25.8779535511027,
0.));
#23824=CARTESIAN_POINT('Ctrl Pts',(-30.2474530144827,-25.9137466853317,
0.));
#23825=CARTESIAN_POINT('Ctrl Pts',(-30.3389466074503,-25.9489196635424,
0.));
#23826=CARTESIAN_POINT('Ctrl Pts',(-30.4308118142473,-25.9834942765902,
0.));
#23827=CARTESIAN_POINT('Ctrl Pts',(-30.5230388264271,-26.0174801292225,
0.));
#23828=CARTESIAN_POINT('Ctrl Pts',(-30.6156232634061,-26.0508796503166,
0.));
#23829=CARTESIAN_POINT('Ctrl Pts',(-30.7085638682391,-26.0836911730968,
0.));
#23830=CARTESIAN_POINT('Ctrl Pts',(-30.8018598357461,-26.1159125093178,
0.));
#23831=CARTESIAN_POINT('Ctrl Pts',(-30.8955077633644,-26.1475450294082,
0.));
#23832=CARTESIAN_POINT('Ctrl Pts',(-30.9895009017073,-26.1785946616165,
0.));
#23833=CARTESIAN_POINT('Ctrl Pts',(-31.0838307058369,-26.2090698085494,
0.));
#23834=CARTESIAN_POINT('Ctrl Pts',(-31.1784877826858,-26.2389800738215,
0.));
#23835=CARTESIAN_POINT('Ctrl Pts',(-31.2734629900041,-26.2683347859175,
0.));
#23836=CARTESIAN_POINT('Ctrl Pts',(-31.3687486937246,-26.2971413115295,
0.));
#23837=CARTESIAN_POINT('Ctrl Pts',(-31.4643390378084,-26.3254046890485,
0.));
#23838=CARTESIAN_POINT('Ctrl Pts',(-31.5602292672984,-26.353128528169,0.));
#23839=CARTESIAN_POINT('Ctrl Pts',(-31.6564152990236,-26.3803155790949,
0.));
#23840=CARTESIAN_POINT('Ctrl Pts',(-31.7528932299312,-26.4069683862784,
0.));
#23841=CARTESIAN_POINT('Ctrl Pts',(-31.849658771403,-26.433090040836,0.));
#23842=CARTESIAN_POINT('Ctrl Pts',(-31.9467071093816,-26.4586843683627,
0.));
#23843=CARTESIAN_POINT('Ctrl Pts',(-32.0440331917233,-26.4837555495616,
0.));
#23844=CARTESIAN_POINT('Ctrl Pts',(-32.1416319023705,-26.5083078928862,
0.));
#23845=CARTESIAN_POINT('Ctrl Pts',(-32.2394982626669,-26.5323455701117,
0.));
#23846=CARTESIAN_POINT('Ctrl Pts',(-32.3376276606981,-26.5558723200361,
0.));
#23847=CARTESIAN_POINT('Ctrl Pts',(-32.4360159072985,-26.5788913672813,
0.));
#23848=CARTESIAN_POINT('Ctrl Pts',(-32.5346590925498,-26.6014055904817,
0.));
#23849=CARTESIAN_POINT('Ctrl Pts',(-32.6335534898936,-26.6234176311245,
0.));
#23850=CARTESIAN_POINT('Ctrl Pts',(-32.7326954489334,-26.6449300199763,
0.));
#23851=CARTESIAN_POINT('Ctrl Pts',(-32.8320812678271,-26.6659453236976,
0.));
#23852=CARTESIAN_POINT('Ctrl Pts',(-32.9317071576181,-26.6864661988935,
0.));
#23853=CARTESIAN_POINT('Ctrl Pts',(-33.03156933761,-26.7064953106254,0.));
#23854=CARTESIAN_POINT('Ctrl Pts',(-33.131664100194,-26.7260352861619,0.));
#23855=CARTESIAN_POINT('Ctrl Pts',(-33.2319878786519,-26.7450886617884,
0.));
#23856=CARTESIAN_POINT('Ctrl Pts',(-33.3325373307046,-26.7636578270526,
0.));
#23857=CARTESIAN_POINT('Ctrl Pts',(-33.4333093513694,-26.7817450041181,
0.));
#23858=CARTESIAN_POINT('Ctrl Pts',(-33.5343009499673,-26.7993522966985,
0.));
#23859=CARTESIAN_POINT('Ctrl Pts',(-33.6355091508895,-26.8164817280846,
0.));
#23860=CARTESIAN_POINT('Ctrl Pts',(-33.7369308933173,-26.8331352836666,
0.));
#23861=CARTESIAN_POINT('Ctrl Pts',(-33.838562905895,-26.8493149627661,0.));
#23862=CARTESIAN_POINT('Ctrl Pts',(-33.9404016650487,-26.8650228056313,
0.));
#23863=CARTESIAN_POINT('Ctrl Pts',(-34.0424436187397,-26.880260834701,0.));
#23864=CARTESIAN_POINT('Ctrl Pts',(-34.1446853651051,-26.8950310138939,
0.));
#23865=CARTESIAN_POINT('Ctrl Pts',(-34.2471238425419,-26.9093352037262,
0.));
#23866=CARTESIAN_POINT('Ctrl Pts',(-34.3497565255724,-26.9231751225177,
0.));
#23867=CARTESIAN_POINT('Ctrl Pts',(-34.4731465943772,-26.9392277420462,
0.));
#23868=CARTESIAN_POINT('Ctrl Pts',(-34.5762105502273,-26.9520281195268,
0.));
#23869=CARTESIAN_POINT('Ctrl Pts',(-34.6588137898952,-26.9619003236529,
0.));
#23870=CARTESIAN_POINT('Ctrl Pts',(-34.7208516760814,-26.9690976283147,
0.));
#23871=CARTESIAN_POINT('Ctrl Pts',(-34.7622482477091,-26.9738038986838,
0.));
#23872=CARTESIAN_POINT('',(-34.762248247709,-26.9738038986839,15.));
#23873=CARTESIAN_POINT('Ctrl Pts',(-34.7622482477091,-26.9738038986838,
15.));
#23874=CARTESIAN_POINT('Ctrl Pts',(-34.7415499619104,-26.9714507634923,
15.));
#23875=CARTESIAN_POINT('Ctrl Pts',(-34.700172380686,-26.9666985267608,15.));
#23876=CARTESIAN_POINT('Ctrl Pts',(-34.6381629799782,-26.9594322726214,
15.));
#23877=CARTESIAN_POINT('Ctrl Pts',(-34.5555977590573,-26.9494680440307,
15.));
#23878=CARTESIAN_POINT('Ctrl Pts',(-34.4525815829097,-26.9365523054581,
15.));
#23879=CARTESIAN_POINT('Ctrl Pts',(-34.3497565255724,-26.9231751225177,
15.));
#23880=CARTESIAN_POINT('Ctrl Pts',(-34.2471238425419,-26.9093352037262,
15.));
#23881=CARTESIAN_POINT('Ctrl Pts',(-34.1446853651051,-26.8950310138939,
15.));
#23882=CARTESIAN_POINT('Ctrl Pts',(-34.0424436187397,-26.880260834701,15.));
#23883=CARTESIAN_POINT('Ctrl Pts',(-33.9404016650487,-26.8650228056313,
15.));
#23884=CARTESIAN_POINT('Ctrl Pts',(-33.838562905895,-26.8493149627661,15.));
#23885=CARTESIAN_POINT('Ctrl Pts',(-33.7369308933173,-26.8331352836666,
15.));
#23886=CARTESIAN_POINT('Ctrl Pts',(-33.6355091508895,-26.8164817280846,
15.));
#23887=CARTESIAN_POINT('Ctrl Pts',(-33.5343009499673,-26.7993522966985,
15.));
#23888=CARTESIAN_POINT('Ctrl Pts',(-33.4333093513694,-26.7817450041181,
15.));
#23889=CARTESIAN_POINT('Ctrl Pts',(-33.3325373307046,-26.7636578270526,
15.));
#23890=CARTESIAN_POINT('Ctrl Pts',(-33.2319878786519,-26.7450886617884,
15.));
#23891=CARTESIAN_POINT('Ctrl Pts',(-33.131664100194,-26.7260352861619,15.));
#23892=CARTESIAN_POINT('Ctrl Pts',(-33.03156933761,-26.7064953106254,15.));
#23893=CARTESIAN_POINT('Ctrl Pts',(-32.9317071576181,-26.6864661988935,
15.));
#23894=CARTESIAN_POINT('Ctrl Pts',(-32.8320812678271,-26.6659453236976,
15.));
#23895=CARTESIAN_POINT('Ctrl Pts',(-32.7326954489334,-26.6449300199763,
15.));
#23896=CARTESIAN_POINT('Ctrl Pts',(-32.6335534898936,-26.6234176311245,
15.));
#23897=CARTESIAN_POINT('Ctrl Pts',(-32.5346590925498,-26.6014055904817,
15.));
#23898=CARTESIAN_POINT('Ctrl Pts',(-32.4360159072985,-26.5788913672813,
15.));
#23899=CARTESIAN_POINT('Ctrl Pts',(-32.3376276606981,-26.5558723200361,
15.));
#23900=CARTESIAN_POINT('Ctrl Pts',(-32.2394982626669,-26.5323455701117,
15.));
#23901=CARTESIAN_POINT('Ctrl Pts',(-32.1416319023705,-26.5083078928862,
15.));
#23902=CARTESIAN_POINT('Ctrl Pts',(-32.0440331917233,-26.4837555495616,
15.));
#23903=CARTESIAN_POINT('Ctrl Pts',(-31.9467071093816,-26.4586843683627,
15.));
#23904=CARTESIAN_POINT('Ctrl Pts',(-31.849658771403,-26.433090040836,15.));
#23905=CARTESIAN_POINT('Ctrl Pts',(-31.7528932299312,-26.4069683862784,
15.));
#23906=CARTESIAN_POINT('Ctrl Pts',(-31.6564152990236,-26.3803155790949,
15.));
#23907=CARTESIAN_POINT('Ctrl Pts',(-31.5602292672984,-26.353128528169,15.));
#23908=CARTESIAN_POINT('Ctrl Pts',(-31.4643390378084,-26.3254046890485,
15.));
#23909=CARTESIAN_POINT('Ctrl Pts',(-31.3687486937246,-26.2971413115295,
15.));
#23910=CARTESIAN_POINT('Ctrl Pts',(-31.2734629900041,-26.2683347859175,
15.));
#23911=CARTESIAN_POINT('Ctrl Pts',(-31.1784877826858,-26.2389800738215,
15.));
#23912=CARTESIAN_POINT('Ctrl Pts',(-31.0838307058369,-26.2090698085494,
15.));
#23913=CARTESIAN_POINT('Ctrl Pts',(-30.9895009017073,-26.1785946616165,
15.));
#23914=CARTESIAN_POINT('Ctrl Pts',(-30.8955077633644,-26.1475450294082,
15.));
#23915=CARTESIAN_POINT('Ctrl Pts',(-30.8018598357461,-26.1159125093178,
15.));
#23916=CARTESIAN_POINT('Ctrl Pts',(-30.7085638682391,-26.0836911730968,
15.));
#23917=CARTESIAN_POINT('Ctrl Pts',(-30.6156232634061,-26.0508796503166,
15.));
#23918=CARTESIAN_POINT('Ctrl Pts',(-30.5230388264271,-26.0174801292225,
15.));
#23919=CARTESIAN_POINT('Ctrl Pts',(-30.4308118142473,-25.9834942765902,
15.));
#23920=CARTESIAN_POINT('Ctrl Pts',(-30.3389466074503,-25.9489196635424,
15.));
#23921=CARTESIAN_POINT('Ctrl Pts',(-30.2474530144827,-25.9137466853317,
15.));
#23922=CARTESIAN_POINT('Ctrl Pts',(-30.1563500154165,-25.8779535511027,
15.));
#23923=CARTESIAN_POINT('Ctrl Pts',(-30.0656638016321,-25.8415089241134,
15.));
#23924=CARTESIAN_POINT('Ctrl Pts',(-29.9754208429384,-25.8043812318214,
15.));
#23925=CARTESIAN_POINT('Ctrl Pts',(-29.8856417535786,-25.7665469042913,
15.));
#23926=CARTESIAN_POINT('Ctrl Pts',(-29.7963360859334,-25.7279973711305,
15.));
#23927=CARTESIAN_POINT('Ctrl Pts',(-29.7074935910931,-25.6887507922748,
15.));
#23928=CARTESIAN_POINT('Ctrl Pts',(-29.6190903904157,-25.6488438125835,
15.));
#23929=CARTESIAN_POINT('Ctrl Pts',(-29.5311055094509,-25.6083094352667,
15.));
#23930=CARTESIAN_POINT('Ctrl Pts',(-29.443535683207,-25.5671572096726,15.));
#23931=CARTESIAN_POINT('Ctrl Pts',(-29.356408021119,-25.5253562922582,15.));
#23932=CARTESIAN_POINT('Ctrl Pts',(-29.2698007967907,-25.4828076101654,
15.));
#23933=CARTESIAN_POINT('Ctrl Pts',(-29.183825549991,-25.4393679214513,15.));
#23934=CARTESIAN_POINT('Ctrl Pts',(-29.098589927237,-25.3948997321279,15.));
#23935=CARTESIAN_POINT('Ctrl Pts',(-29.0141637699076,-25.3493168206005,
15.));
#23936=CARTESIAN_POINT('Ctrl Pts',(-28.9305499160476,-25.3026235249214,
15.));
#23937=CARTESIAN_POINT('Ctrl Pts',(-28.8476372998748,-25.2549775629725,
15.));
#23938=CARTESIAN_POINT('Ctrl Pts',(-28.7652594076549,-25.2066127148845,
15.));
#23939=CARTESIAN_POINT('Ctrl Pts',(-28.6832861366762,-25.1577170374459,
15.));
#23940=CARTESIAN_POINT('Ctrl Pts',(-28.6017081342376,-25.108321158239,15.));
#23941=CARTESIAN_POINT('Ctrl Pts',(-28.5207164321473,-25.0581926620043,
15.));
#23942=CARTESIAN_POINT('Ctrl Pts',(-28.4408053900206,-25.0066999111736,
15.));
#23943=CARTESIAN_POINT('Ctrl Pts',(-28.3626431274892,-24.9529811166897,
15.));
#23944=CARTESIAN_POINT('Ctrl Pts',(-28.3020534756061,-24.9075246543798,
15.));
#23945=CARTESIAN_POINT('Ctrl Pts',(-28.2579420132101,-24.8717258526943,
15.));
#23946=CARTESIAN_POINT('Ctrl Pts',(-28.2291563988796,-24.8470618363541,
15.));
#23947=CARTESIAN_POINT('Ctrl Pts',(-28.2149191006269,-24.8345302882955,
15.));
#23948=CARTESIAN_POINT('',(-34.762248247709,-26.9738038986839,0.));
#23949=CARTESIAN_POINT('Origin',(-9.16871631793044E-12,-6.66146233219319E-12,
0.));
#23950=CARTESIAN_POINT('',(-36.3957374383337,-24.725498909423,0.));
#23951=CARTESIAN_POINT('Origin',(-9.16871631793044E-12,-6.66146233219319E-12,
0.));
#23952=CARTESIAN_POINT('',(-36.3957374383337,-24.725498909423,15.));
#23953=CARTESIAN_POINT('Origin',(-9.16871631793044E-12,-6.66146233219319E-12,
15.));
#23954=CARTESIAN_POINT('',(-36.3957374383337,-24.725498909423,0.));
#23955=CARTESIAN_POINT('Ctrl Pts',(-32.3379313568208,-19.1596907609891,
0.));
#23956=CARTESIAN_POINT('Ctrl Pts',(-32.3379313568208,-19.1596907609891,
18.));
#23957=CARTESIAN_POINT('Ctrl Pts',(-32.3542491343753,-19.1693587749508,
0.));
#23958=CARTESIAN_POINT('Ctrl Pts',(-32.3542491343753,-19.1693587749508,
18.));
#23959=CARTESIAN_POINT('Ctrl Pts',(-32.3866012518553,-19.1891139208368,
0.));
#23960=CARTESIAN_POINT('Ctrl Pts',(-32.3866012518553,-19.1891139208368,
18.));
#23961=CARTESIAN_POINT('Ctrl Pts',(-32.4342791270009,-19.2200039764927,
0.));
#23962=CARTESIAN_POINT('Ctrl Pts',(-32.4342791270009,-19.2200039764927,
18.));
#23963=CARTESIAN_POINT('Ctrl Pts',(-32.4962340238036,-19.2635813403783,
0.));
#23964=CARTESIAN_POINT('Ctrl Pts',(-32.4962340238036,-19.2635813403783,
18.));
#23965=CARTESIAN_POINT('Ctrl Pts',(-32.5714771007861,-19.3213180490743,
0.));
#23966=CARTESIAN_POINT('Ctrl Pts',(-32.5714771007861,-19.3213180490743,
18.));
#23967=CARTESIAN_POINT('Ctrl Pts',(-32.6451434870609,-19.381405831319,0.));
#23968=CARTESIAN_POINT('Ctrl Pts',(-32.6451434870609,-19.381405831319,18.));
#23969=CARTESIAN_POINT('Ctrl Pts',(-32.7178463324062,-19.4429429601189,
0.));
#23970=CARTESIAN_POINT('Ctrl Pts',(-32.7178463324062,-19.4429429601189,
18.));
#23971=CARTESIAN_POINT('Ctrl Pts',(-32.7900335943248,-19.5052640847974,
0.));
#23972=CARTESIAN_POINT('Ctrl Pts',(-32.7900335943248,-19.5052640847974,
18.));
#23973=CARTESIAN_POINT('Ctrl Pts',(-32.8618672807884,-19.5681157030437,
0.));
#23974=CARTESIAN_POINT('Ctrl Pts',(-32.8618672807884,-19.5681157030437,
18.));
#23975=CARTESIAN_POINT('Ctrl Pts',(-32.9333211533788,-19.6315161742485,
0.));
#23976=CARTESIAN_POINT('Ctrl Pts',(-32.9333211533788,-19.6315161742485,
18.));
#23977=CARTESIAN_POINT('Ctrl Pts',(-33.004256563411,-19.6956473461873,0.));
#23978=CARTESIAN_POINT('Ctrl Pts',(-33.004256563411,-19.6956473461873,18.));
#23979=CARTESIAN_POINT('Ctrl Pts',(-33.0745026283418,-19.7607398248651,
0.));
#23980=CARTESIAN_POINT('Ctrl Pts',(-33.0745026283418,-19.7607398248651,
18.));
#23981=CARTESIAN_POINT('Ctrl Pts',(-33.1439436707661,-19.8269479776239,
0.));
#23982=CARTESIAN_POINT('Ctrl Pts',(-33.1439436707661,-19.8269479776239,
18.));
#23983=CARTESIAN_POINT('Ctrl Pts',(-33.2125746879472,-19.8942704458546,
0.));
#23984=CARTESIAN_POINT('Ctrl Pts',(-33.2125746879472,-19.8942704458546,
18.));
#23985=CARTESIAN_POINT('Ctrl Pts',(-33.2804560993213,-19.9626141625205,
0.));
#23986=CARTESIAN_POINT('Ctrl Pts',(-33.2804560993213,-19.9626141625205,
18.));
#23987=CARTESIAN_POINT('Ctrl Pts',(-33.3476854048385,-20.0318342617212,
0.));
#23988=CARTESIAN_POINT('Ctrl Pts',(-33.3476854048385,-20.0318342617212,
18.));
#23989=CARTESIAN_POINT('Ctrl Pts',(-33.4143643679979,-20.1017803986381,
0.));
#23990=CARTESIAN_POINT('Ctrl Pts',(-33.4143643679979,-20.1017803986381,
18.));
#23991=CARTESIAN_POINT('Ctrl Pts',(-33.480563024813,-20.1723475154533,0.));
#23992=CARTESIAN_POINT('Ctrl Pts',(-33.480563024813,-20.1723475154533,18.));
#23993=CARTESIAN_POINT('Ctrl Pts',(-33.5463023319603,-20.243500298383,0.));
#23994=CARTESIAN_POINT('Ctrl Pts',(-33.5463023319603,-20.243500298383,18.));
#23995=CARTESIAN_POINT('Ctrl Pts',(-33.6115742164079,-20.3152448035298,
0.));
#23996=CARTESIAN_POINT('Ctrl Pts',(-33.6115742164079,-20.3152448035298,
18.));
#23997=CARTESIAN_POINT('Ctrl Pts',(-33.6763537716992,-20.3876111773341,
0.));
#23998=CARTESIAN_POINT('Ctrl Pts',(-33.6763537716992,-20.3876111773341,
18.));
#23999=CARTESIAN_POINT('Ctrl Pts',(-33.7406135254083,-20.4606334536183,
0.));
#24000=CARTESIAN_POINT('Ctrl Pts',(-33.7406135254083,-20.4606334536183,
18.));
#24001=CARTESIAN_POINT('Ctrl Pts',(-33.8043393734971,-20.5343269914034,
0.));
#24002=CARTESIAN_POINT('Ctrl Pts',(-33.8043393734971,-20.5343269914034,
18.));
#24003=CARTESIAN_POINT('Ctrl Pts',(-33.8675365150454,-20.6086800574386,
0.));
#24004=CARTESIAN_POINT('Ctrl Pts',(-33.8675365150454,-20.6086800574386,
18.));
#24005=CARTESIAN_POINT('Ctrl Pts',(-33.9302209962425,-20.683665762903,0.));
#24006=CARTESIAN_POINT('Ctrl Pts',(-33.9302209962425,-20.683665762903,18.));
#24007=CARTESIAN_POINT('Ctrl Pts',(-33.9924146647395,-20.7592491770603,
0.));
#24008=CARTESIAN_POINT('Ctrl Pts',(-33.9924146647395,-20.7592491770603,
18.));
#24009=CARTESIAN_POINT('Ctrl Pts',(-34.0541392299678,-20.8353957068415,
0.));
#24010=CARTESIAN_POINT('Ctrl Pts',(-34.0541392299678,-20.8353957068415,
18.));
#24011=CARTESIAN_POINT('Ctrl Pts',(-34.1154095510973,-20.9120805673809,
0.));
#24012=CARTESIAN_POINT('Ctrl Pts',(-34.1154095510973,-20.9120805673809,
18.));
#24013=CARTESIAN_POINT('Ctrl Pts',(-34.176231731809,-20.9892914622612,0.));
#24014=CARTESIAN_POINT('Ctrl Pts',(-34.176231731809,-20.9892914622612,18.));
#24015=CARTESIAN_POINT('Ctrl Pts',(-34.2366067284279,-21.0670234747355,
0.));
#24016=CARTESIAN_POINT('Ctrl Pts',(-34.2366067284279,-21.0670234747355,
18.));
#24017=CARTESIAN_POINT('Ctrl Pts',(-34.2965325673384,-21.1452759244399,
0.));
#24018=CARTESIAN_POINT('Ctrl Pts',(-34.2965325673384,-21.1452759244399,
18.));
#24019=CARTESIAN_POINT('Ctrl Pts',(-34.3560069185815,-21.2240487218079,
0.));
#24020=CARTESIAN_POINT('Ctrl Pts',(-34.3560069185815,-21.2240487218079,
18.));
#24021=CARTESIAN_POINT('Ctrl Pts',(-34.4150300340623,-21.3033382073239,
0.));
#24022=CARTESIAN_POINT('Ctrl Pts',(-34.4150300340623,-21.3033382073239,
18.));
#24023=CARTESIAN_POINT('Ctrl Pts',(-34.4736054662052,-21.3831361300104,
0.));
#24024=CARTESIAN_POINT('Ctrl Pts',(-34.4736054662052,-21.3831361300104,
18.));
#24025=CARTESIAN_POINT('Ctrl Pts',(-34.5317385658329,-21.4634317666005,
0.));
#24026=CARTESIAN_POINT('Ctrl Pts',(-34.5317385658329,-21.4634317666005,
18.));
#24027=CARTESIAN_POINT('Ctrl Pts',(-34.5894355639082,-21.5442132160757,
0.));
#24028=CARTESIAN_POINT('Ctrl Pts',(-34.5894355639082,-21.5442132160757,
18.));
#24029=CARTESIAN_POINT('Ctrl Pts',(-34.6467025072367,-21.6254689009796,
0.));
#24030=CARTESIAN_POINT('Ctrl Pts',(-34.6467025072367,-21.6254689009796,
18.));
#24031=CARTESIAN_POINT('Ctrl Pts',(-34.7035440429025,-21.7071892844497,
0.));
#24032=CARTESIAN_POINT('Ctrl Pts',(-34.7035440429025,-21.7071892844497,
18.));
#24033=CARTESIAN_POINT('Ctrl Pts',(-34.7599631530844,-21.7893672401137,
0.));
#24034=CARTESIAN_POINT('Ctrl Pts',(-34.7599631530844,-21.7893672401137,
18.));
#24035=CARTESIAN_POINT('Ctrl Pts',(-34.8159618014436,-21.8719971302817,
0.));
#24036=CARTESIAN_POINT('Ctrl Pts',(-34.8159618014436,-21.8719971302817,
18.));
#24037=CARTESIAN_POINT('Ctrl Pts',(-34.8715413418101,-21.9550742217675,
0.));
#24038=CARTESIAN_POINT('Ctrl Pts',(-34.8715413418101,-21.9550742217675,
18.));
#24039=CARTESIAN_POINT('Ctrl Pts',(-34.9267029879922,-22.0385940162683,
0.));
#24040=CARTESIAN_POINT('Ctrl Pts',(-34.9267029879922,-22.0385940162683,
18.));
#24041=CARTESIAN_POINT('Ctrl Pts',(-34.9814483545602,-22.1225514798584,
0.));
#24042=CARTESIAN_POINT('Ctrl Pts',(-34.9814483545602,-22.1225514798584,
18.));
#24043=CARTESIAN_POINT('Ctrl Pts',(-35.0357795922459,-22.2069408519232,
0.));
#24044=CARTESIAN_POINT('Ctrl Pts',(-35.0357795922459,-22.2069408519232,
18.));
#24045=CARTESIAN_POINT('Ctrl Pts',(-35.0896991159359,-22.2917560356803,
0.));
#24046=CARTESIAN_POINT('Ctrl Pts',(-35.0896991159359,-22.2917560356803,
18.));
#24047=CARTESIAN_POINT('Ctrl Pts',(-35.1432094422642,-22.3769908340843,
0.));
#24048=CARTESIAN_POINT('Ctrl Pts',(-35.1432094422642,-22.3769908340843,
18.));
#24049=CARTESIAN_POINT('Ctrl Pts',(-35.1963130003352,-22.4626392230023,
0.));
#24050=CARTESIAN_POINT('Ctrl Pts',(-35.1963130003352,-22.4626392230023,
18.));
#24051=CARTESIAN_POINT('Ctrl Pts',(-35.2490119207975,-22.5486956608909,
0.));
#24052=CARTESIAN_POINT('Ctrl Pts',(-35.2490119207975,-22.5486956608909,
18.));
#24053=CARTESIAN_POINT('Ctrl Pts',(-35.3013079759252,-22.635155167154,0.));
#24054=CARTESIAN_POINT('Ctrl Pts',(-35.3013079759252,-22.635155167154,18.));
#24055=CARTESIAN_POINT('Ctrl Pts',(-35.3532026952313,-22.7220131336912,
0.));
#24056=CARTESIAN_POINT('Ctrl Pts',(-35.3532026952313,-22.7220131336912,
18.));
#24057=CARTESIAN_POINT('Ctrl Pts',(-35.4046974393492,-22.8092652000706,
0.));
#24058=CARTESIAN_POINT('Ctrl Pts',(-35.4046974393492,-22.8092652000706,
18.));
#24059=CARTESIAN_POINT('Ctrl Pts',(-35.4557934871468,-22.8969071125089,
0.));
#24060=CARTESIAN_POINT('Ctrl Pts',(-35.4557934871468,-22.8969071125089,
18.));
#24061=CARTESIAN_POINT('Ctrl Pts',(-35.5064921357308,-22.9849345572033,
0.));
#24062=CARTESIAN_POINT('Ctrl Pts',(-35.5064921357308,-22.9849345572033,
18.));
#24063=CARTESIAN_POINT('Ctrl Pts',(-35.5567947408311,-23.0733431097058,
0.));
#24064=CARTESIAN_POINT('Ctrl Pts',(-35.5567947408311,-23.0733431097058,
18.));
#24065=CARTESIAN_POINT('Ctrl Pts',(-35.6067026687722,-23.1621283508111,
0.));
#24066=CARTESIAN_POINT('Ctrl Pts',(-35.6067026687722,-23.1621283508111,
18.));
#24067=CARTESIAN_POINT('Ctrl Pts',(-35.6562172725207,-23.2512859425032,
0.));
#24068=CARTESIAN_POINT('Ctrl Pts',(-35.6562172725207,-23.2512859425032,
18.));
#24069=CARTESIAN_POINT('Ctrl Pts',(-35.7053398620512,-23.3408117088761,
0.));
#24070=CARTESIAN_POINT('Ctrl Pts',(-35.7053398620512,-23.3408117088761,
18.));
#24071=CARTESIAN_POINT('Ctrl Pts',(-35.7540716771372,-23.4307017328227,
0.));
#24072=CARTESIAN_POINT('Ctrl Pts',(-35.7540716771372,-23.4307017328227,
18.));
#24073=CARTESIAN_POINT('Ctrl Pts',(-35.8024138716897,-23.5209523746427,
0.));
#24074=CARTESIAN_POINT('Ctrl Pts',(-35.8024138716897,-23.5209523746427,
18.));
#24075=CARTESIAN_POINT('Ctrl Pts',(-35.8503675222885,-23.611560139948,0.));
#24076=CARTESIAN_POINT('Ctrl Pts',(-35.8503675222885,-23.611560139948,18.));
#24077=CARTESIAN_POINT('Ctrl Pts',(-35.8979336336837,-23.7025215735353,
0.));
#24078=CARTESIAN_POINT('Ctrl Pts',(-35.8979336336837,-23.7025215735353,
18.));
#24079=CARTESIAN_POINT('Ctrl Pts',(-35.9451131482488,-23.7938331508737,
0.));
#24080=CARTESIAN_POINT('Ctrl Pts',(-35.9451131482488,-23.7938331508737,
18.));
#24081=CARTESIAN_POINT('Ctrl Pts',(-35.991906956547,-23.8854911428946,0.));
#24082=CARTESIAN_POINT('Ctrl Pts',(-35.991906956547,-23.8854911428946,18.));
#24083=CARTESIAN_POINT('Ctrl Pts',(-36.0383159101254,-23.9774915680089,
0.));
#24084=CARTESIAN_POINT('Ctrl Pts',(-36.0383159101254,-23.9774915680089,
18.));
#24085=CARTESIAN_POINT('Ctrl Pts',(-36.0843408347974,-24.0698304230588,
0.));
#24086=CARTESIAN_POINT('Ctrl Pts',(-36.0843408347974,-24.0698304230588,
18.));
#24087=CARTESIAN_POINT('Ctrl Pts',(-36.1299825471271,-24.1625038657964,
0.));
#24088=CARTESIAN_POINT('Ctrl Pts',(-36.1299825471271,-24.1625038657964,
18.));
#24089=CARTESIAN_POINT('Ctrl Pts',(-36.1752418704833,-24.2555084095332,
0.));
#24090=CARTESIAN_POINT('Ctrl Pts',(-36.1752418704833,-24.2555084095332,
18.));
#24091=CARTESIAN_POINT('Ctrl Pts',(-36.2201196586697,-24.3488411214068,
0.));
#24092=CARTESIAN_POINT('Ctrl Pts',(-36.2201196586697,-24.3488411214068,
18.));
#24093=CARTESIAN_POINT('Ctrl Pts',(-36.2646168058396,-24.4424997853605,
0.));
#24094=CARTESIAN_POINT('Ctrl Pts',(-36.2646168058396,-24.4424997853605,
18.));
#24095=CARTESIAN_POINT('Ctrl Pts',(-36.308734152297,-24.5364828082556,0.));
#24096=CARTESIAN_POINT('Ctrl Pts',(-36.308734152297,-24.5364828082556,18.));
#24097=CARTESIAN_POINT('Ctrl Pts',(-36.3437247532369,-24.6119278836614,
0.));
#24098=CARTESIAN_POINT('Ctrl Pts',(-36.3437247532369,-24.6119278836614,
18.));
#24099=CARTESIAN_POINT('Ctrl Pts',(-36.369797330215,-24.6686569322616,0.));
#24100=CARTESIAN_POINT('Ctrl Pts',(-36.369797330215,-24.6686569322616,18.));
#24101=CARTESIAN_POINT('Ctrl Pts',(-36.3871033517098,-24.7065408286023,
0.));
#24102=CARTESIAN_POINT('Ctrl Pts',(-36.3871033517098,-24.7065408286023,
18.));
#24103=CARTESIAN_POINT('Ctrl Pts',(-36.3957374383337,-24.725498909423,0.));
#24104=CARTESIAN_POINT('Ctrl Pts',(-36.3957374383337,-24.725498909423,18.));
#24105=CARTESIAN_POINT('Ctrl Pts',(-32.3379313568208,-19.1596907609891,
0.));
#24106=CARTESIAN_POINT('Ctrl Pts',(-32.3542491343753,-19.1693587749508,
0.));
#24107=CARTESIAN_POINT('Ctrl Pts',(-32.3866012518553,-19.1891139208368,
0.));
#24108=CARTESIAN_POINT('Ctrl Pts',(-32.4342791270009,-19.2200039764927,
0.));
#24109=CARTESIAN_POINT('Ctrl Pts',(-32.4962340238036,-19.2635813403783,
0.));
#24110=CARTESIAN_POINT('Ctrl Pts',(-32.5714771007861,-19.3213180490743,
0.));
#24111=CARTESIAN_POINT('Ctrl Pts',(-32.6451434870609,-19.381405831319,0.));
#24112=CARTESIAN_POINT('Ctrl Pts',(-32.7178463324062,-19.4429429601189,
0.));
#24113=CARTESIAN_POINT('Ctrl Pts',(-32.7900335943248,-19.5052640847974,
0.));
#24114=CARTESIAN_POINT('Ctrl Pts',(-32.8618672807884,-19.5681157030437,
0.));
#24115=CARTESIAN_POINT('Ctrl Pts',(-32.9333211533788,-19.6315161742485,
0.));
#24116=CARTESIAN_POINT('Ctrl Pts',(-33.004256563411,-19.6956473461873,0.));
#24117=CARTESIAN_POINT('Ctrl Pts',(-33.0745026283418,-19.7607398248651,
0.));
#24118=CARTESIAN_POINT('Ctrl Pts',(-33.1439436707661,-19.8269479776239,
0.));
#24119=CARTESIAN_POINT('Ctrl Pts',(-33.2125746879472,-19.8942704458546,
0.));
#24120=CARTESIAN_POINT('Ctrl Pts',(-33.2804560993213,-19.9626141625205,
0.));
#24121=CARTESIAN_POINT('Ctrl Pts',(-33.3476854048385,-20.0318342617212,
0.));
#24122=CARTESIAN_POINT('Ctrl Pts',(-33.4143643679979,-20.1017803986381,
0.));
#24123=CARTESIAN_POINT('Ctrl Pts',(-33.480563024813,-20.1723475154533,0.));
#24124=CARTESIAN_POINT('Ctrl Pts',(-33.5463023319603,-20.243500298383,0.));
#24125=CARTESIAN_POINT('Ctrl Pts',(-33.6115742164079,-20.3152448035298,
0.));
#24126=CARTESIAN_POINT('Ctrl Pts',(-33.6763537716992,-20.3876111773341,
0.));
#24127=CARTESIAN_POINT('Ctrl Pts',(-33.7406135254083,-20.4606334536183,
0.));
#24128=CARTESIAN_POINT('Ctrl Pts',(-33.8043393734971,-20.5343269914034,
0.));
#24129=CARTESIAN_POINT('Ctrl Pts',(-33.8675365150454,-20.6086800574386,
0.));
#24130=CARTESIAN_POINT('Ctrl Pts',(-33.9302209962425,-20.683665762903,0.));
#24131=CARTESIAN_POINT('Ctrl Pts',(-33.9924146647395,-20.7592491770603,
0.));
#24132=CARTESIAN_POINT('Ctrl Pts',(-34.0541392299678,-20.8353957068415,
0.));
#24133=CARTESIAN_POINT('Ctrl Pts',(-34.1154095510973,-20.9120805673809,
0.));
#24134=CARTESIAN_POINT('Ctrl Pts',(-34.176231731809,-20.9892914622612,0.));
#24135=CARTESIAN_POINT('Ctrl Pts',(-34.2366067284279,-21.0670234747355,
0.));
#24136=CARTESIAN_POINT('Ctrl Pts',(-34.2965325673384,-21.1452759244399,
0.));
#24137=CARTESIAN_POINT('Ctrl Pts',(-34.3560069185815,-21.2240487218079,
0.));
#24138=CARTESIAN_POINT('Ctrl Pts',(-34.4150300340623,-21.3033382073239,
0.));
#24139=CARTESIAN_POINT('Ctrl Pts',(-34.4736054662052,-21.3831361300104,
0.));
#24140=CARTESIAN_POINT('Ctrl Pts',(-34.5317385658329,-21.4634317666005,
0.));
#24141=CARTESIAN_POINT('Ctrl Pts',(-34.5894355639082,-21.5442132160757,
0.));
#24142=CARTESIAN_POINT('Ctrl Pts',(-34.6467025072367,-21.6254689009796,
0.));
#24143=CARTESIAN_POINT('Ctrl Pts',(-34.7035440429025,-21.7071892844497,
0.));
#24144=CARTESIAN_POINT('Ctrl Pts',(-34.7599631530844,-21.7893672401137,
0.));
#24145=CARTESIAN_POINT('Ctrl Pts',(-34.8159618014436,-21.8719971302817,
0.));
#24146=CARTESIAN_POINT('Ctrl Pts',(-34.8715413418101,-21.9550742217675,
0.));
#24147=CARTESIAN_POINT('Ctrl Pts',(-34.9267029879922,-22.0385940162683,
0.));
#24148=CARTESIAN_POINT('Ctrl Pts',(-34.9814483545602,-22.1225514798584,
0.));
#24149=CARTESIAN_POINT('Ctrl Pts',(-35.0357795922459,-22.2069408519232,
0.));
#24150=CARTESIAN_POINT('Ctrl Pts',(-35.0896991159359,-22.2917560356803,
0.));
#24151=CARTESIAN_POINT('Ctrl Pts',(-35.1432094422642,-22.3769908340843,
0.));
#24152=CARTESIAN_POINT('Ctrl Pts',(-35.1963130003352,-22.4626392230023,
0.));
#24153=CARTESIAN_POINT('Ctrl Pts',(-35.2490119207975,-22.5486956608909,
0.));
#24154=CARTESIAN_POINT('Ctrl Pts',(-35.3013079759252,-22.635155167154,0.));
#24155=CARTESIAN_POINT('Ctrl Pts',(-35.3532026952313,-22.7220131336912,
0.));
#24156=CARTESIAN_POINT('Ctrl Pts',(-35.4046974393492,-22.8092652000706,
0.));
#24157=CARTESIAN_POINT('Ctrl Pts',(-35.4557934871468,-22.8969071125089,
0.));
#24158=CARTESIAN_POINT('Ctrl Pts',(-35.5064921357308,-22.9849345572033,
0.));
#24159=CARTESIAN_POINT('Ctrl Pts',(-35.5567947408311,-23.0733431097058,
0.));
#24160=CARTESIAN_POINT('Ctrl Pts',(-35.6067026687722,-23.1621283508111,
0.));
#24161=CARTESIAN_POINT('Ctrl Pts',(-35.6562172725207,-23.2512859425032,
0.));
#24162=CARTESIAN_POINT('Ctrl Pts',(-35.7053398620512,-23.3408117088761,
0.));
#24163=CARTESIAN_POINT('Ctrl Pts',(-35.7540716771372,-23.4307017328227,
0.));
#24164=CARTESIAN_POINT('Ctrl Pts',(-35.8024138716897,-23.5209523746427,
0.));
#24165=CARTESIAN_POINT('Ctrl Pts',(-35.8503675222885,-23.611560139948,0.));
#24166=CARTESIAN_POINT('Ctrl Pts',(-35.8979336336837,-23.7025215735353,
0.));
#24167=CARTESIAN_POINT('Ctrl Pts',(-35.9451131482488,-23.7938331508737,
0.));
#24168=CARTESIAN_POINT('Ctrl Pts',(-35.991906956547,-23.8854911428946,0.));
#24169=CARTESIAN_POINT('Ctrl Pts',(-36.0383159101254,-23.9774915680089,
0.));
#24170=CARTESIAN_POINT('Ctrl Pts',(-36.0843408347974,-24.0698304230588,
0.));
#24171=CARTESIAN_POINT('Ctrl Pts',(-36.1299825471271,-24.1625038657964,
0.));
#24172=CARTESIAN_POINT('Ctrl Pts',(-36.1752418704833,-24.2555084095332,
0.));
#24173=CARTESIAN_POINT('Ctrl Pts',(-36.2201196586697,-24.3488411214068,
0.));
#24174=CARTESIAN_POINT('Ctrl Pts',(-36.2735162352736,-24.4612315181512,
0.));
#24175=CARTESIAN_POINT('Ctrl Pts',(-36.3175386315529,-24.5552956307817,
0.));
#24176=CARTESIAN_POINT('Ctrl Pts',(-36.3524534604649,-24.630805301288,0.));
#24177=CARTESIAN_POINT('Ctrl Pts',(-36.37846926509,-24.6875827477484,0.));
#24178=CARTESIAN_POINT('Ctrl Pts',(-36.3957374383337,-24.725498909423,0.));
#24179=CARTESIAN_POINT('Ctrl Pts',(-32.3379313568208,-19.1596907609891,
15.));
#24180=CARTESIAN_POINT('Ctrl Pts',(-32.3542491343753,-19.1693587749508,
15.));
#24181=CARTESIAN_POINT('Ctrl Pts',(-32.3866012518553,-19.1891139208368,
15.));
#24182=CARTESIAN_POINT('Ctrl Pts',(-32.4342791270009,-19.2200039764927,
15.));
#24183=CARTESIAN_POINT('Ctrl Pts',(-32.4962340238036,-19.2635813403783,
15.));
#24184=CARTESIAN_POINT('Ctrl Pts',(-32.5714771007861,-19.3213180490743,
15.));
#24185=CARTESIAN_POINT('Ctrl Pts',(-32.6451434870609,-19.381405831319,15.));
#24186=CARTESIAN_POINT('Ctrl Pts',(-32.7178463324062,-19.4429429601189,
15.));
#24187=CARTESIAN_POINT('Ctrl Pts',(-32.7900335943248,-19.5052640847974,
15.));
#24188=CARTESIAN_POINT('Ctrl Pts',(-32.8618672807884,-19.5681157030437,
15.));
#24189=CARTESIAN_POINT('Ctrl Pts',(-32.9333211533788,-19.6315161742485,
15.));
#24190=CARTESIAN_POINT('Ctrl Pts',(-33.004256563411,-19.6956473461873,15.));
#24191=CARTESIAN_POINT('Ctrl Pts',(-33.0745026283418,-19.7607398248651,
15.));
#24192=CARTESIAN_POINT('Ctrl Pts',(-33.1439436707661,-19.8269479776239,
15.));
#24193=CARTESIAN_POINT('Ctrl Pts',(-33.2125746879472,-19.8942704458546,
15.));
#24194=CARTESIAN_POINT('Ctrl Pts',(-33.2804560993213,-19.9626141625205,
15.));
#24195=CARTESIAN_POINT('Ctrl Pts',(-33.3476854048385,-20.0318342617212,
15.));
#24196=CARTESIAN_POINT('Ctrl Pts',(-33.4143643679979,-20.1017803986381,
15.));
#24197=CARTESIAN_POINT('Ctrl Pts',(-33.480563024813,-20.1723475154533,15.));
#24198=CARTESIAN_POINT('Ctrl Pts',(-33.5463023319603,-20.243500298383,15.));
#24199=CARTESIAN_POINT('Ctrl Pts',(-33.6115742164079,-20.3152448035298,
15.));
#24200=CARTESIAN_POINT('Ctrl Pts',(-33.6763537716992,-20.3876111773341,
15.));
#24201=CARTESIAN_POINT('Ctrl Pts',(-33.7406135254083,-20.4606334536183,
15.));
#24202=CARTESIAN_POINT('Ctrl Pts',(-33.8043393734971,-20.5343269914034,
15.));
#24203=CARTESIAN_POINT('Ctrl Pts',(-33.8675365150454,-20.6086800574386,
15.));
#24204=CARTESIAN_POINT('Ctrl Pts',(-33.9302209962425,-20.683665762903,15.));
#24205=CARTESIAN_POINT('Ctrl Pts',(-33.9924146647395,-20.7592491770603,
15.));
#24206=CARTESIAN_POINT('Ctrl Pts',(-34.0541392299678,-20.8353957068415,
15.));
#24207=CARTESIAN_POINT('Ctrl Pts',(-34.1154095510973,-20.9120805673809,
15.));
#24208=CARTESIAN_POINT('Ctrl Pts',(-34.176231731809,-20.9892914622612,15.));
#24209=CARTESIAN_POINT('Ctrl Pts',(-34.2366067284279,-21.0670234747355,
15.));
#24210=CARTESIAN_POINT('Ctrl Pts',(-34.2965325673384,-21.1452759244399,
15.));
#24211=CARTESIAN_POINT('Ctrl Pts',(-34.3560069185815,-21.2240487218079,
15.));
#24212=CARTESIAN_POINT('Ctrl Pts',(-34.4150300340623,-21.3033382073239,
15.));
#24213=CARTESIAN_POINT('Ctrl Pts',(-34.4736054662052,-21.3831361300104,
15.));
#24214=CARTESIAN_POINT('Ctrl Pts',(-34.5317385658329,-21.4634317666005,
15.));
#24215=CARTESIAN_POINT('Ctrl Pts',(-34.5894355639082,-21.5442132160757,
15.));
#24216=CARTESIAN_POINT('Ctrl Pts',(-34.6467025072367,-21.6254689009796,
15.));
#24217=CARTESIAN_POINT('Ctrl Pts',(-34.7035440429025,-21.7071892844497,
15.));
#24218=CARTESIAN_POINT('Ctrl Pts',(-34.7599631530844,-21.7893672401137,
15.));
#24219=CARTESIAN_POINT('Ctrl Pts',(-34.8159618014436,-21.8719971302817,
15.));
#24220=CARTESIAN_POINT('Ctrl Pts',(-34.8715413418101,-21.9550742217675,
15.));
#24221=CARTESIAN_POINT('Ctrl Pts',(-34.9267029879922,-22.0385940162683,
15.));
#24222=CARTESIAN_POINT('Ctrl Pts',(-34.9814483545602,-22.1225514798584,
15.));
#24223=CARTESIAN_POINT('Ctrl Pts',(-35.0357795922459,-22.2069408519232,
15.));
#24224=CARTESIAN_POINT('Ctrl Pts',(-35.0896991159359,-22.2917560356803,
15.));
#24225=CARTESIAN_POINT('Ctrl Pts',(-35.1432094422642,-22.3769908340843,
15.));
#24226=CARTESIAN_POINT('Ctrl Pts',(-35.1963130003352,-22.4626392230023,
15.));
#24227=CARTESIAN_POINT('Ctrl Pts',(-35.2490119207975,-22.5486956608909,
15.));
#24228=CARTESIAN_POINT('Ctrl Pts',(-35.3013079759252,-22.635155167154,15.));
#24229=CARTESIAN_POINT('Ctrl Pts',(-35.3532026952313,-22.7220131336912,
15.));
#24230=CARTESIAN_POINT('Ctrl Pts',(-35.4046974393492,-22.8092652000706,
15.));
#24231=CARTESIAN_POINT('Ctrl Pts',(-35.4557934871468,-22.8969071125089,
15.));
#24232=CARTESIAN_POINT('Ctrl Pts',(-35.5064921357308,-22.9849345572033,
15.));
#24233=CARTESIAN_POINT('Ctrl Pts',(-35.5567947408311,-23.0733431097058,
15.));
#24234=CARTESIAN_POINT('Ctrl Pts',(-35.6067026687722,-23.1621283508111,
15.));
#24235=CARTESIAN_POINT('Ctrl Pts',(-35.6562172725207,-23.2512859425032,
15.));
#24236=CARTESIAN_POINT('Ctrl Pts',(-35.7053398620512,-23.3408117088761,
15.));
#24237=CARTESIAN_POINT('Ctrl Pts',(-35.7540716771372,-23.4307017328227,
15.));
#24238=CARTESIAN_POINT('Ctrl Pts',(-35.8024138716897,-23.5209523746427,
15.));
#24239=CARTESIAN_POINT('Ctrl Pts',(-35.8503675222885,-23.611560139948,15.));
#24240=CARTESIAN_POINT('Ctrl Pts',(-35.8979336336837,-23.7025215735353,
15.));
#24241=CARTESIAN_POINT('Ctrl Pts',(-35.9451131482488,-23.7938331508737,
15.));
#24242=CARTESIAN_POINT('Ctrl Pts',(-35.991906956547,-23.8854911428946,15.));
#24243=CARTESIAN_POINT('Ctrl Pts',(-36.0383159101254,-23.9774915680089,
15.));
#24244=CARTESIAN_POINT('Ctrl Pts',(-36.0843408347974,-24.0698304230588,
15.));
#24245=CARTESIAN_POINT('Ctrl Pts',(-36.1299825471271,-24.1625038657964,
15.));
#24246=CARTESIAN_POINT('Ctrl Pts',(-36.1752418704833,-24.2555084095332,
15.));
#24247=CARTESIAN_POINT('Ctrl Pts',(-36.2201196586697,-24.3488411214068,
15.));
#24248=CARTESIAN_POINT('Ctrl Pts',(-36.2735162352736,-24.4612315181512,
15.));
#24249=CARTESIAN_POINT('Ctrl Pts',(-36.3175386315529,-24.5552956307817,
15.));
#24250=CARTESIAN_POINT('Ctrl Pts',(-36.3524534604649,-24.630805301288,15.));
#24251=CARTESIAN_POINT('Ctrl Pts',(-36.37846926509,-24.6875827477484,15.));
#24252=CARTESIAN_POINT('Ctrl Pts',(-36.3957374383337,-24.725498909423,15.));
#24253=CARTESIAN_POINT('Ctrl Pts',(-41.396226524684,-14.911486495888,0.));
#24254=CARTESIAN_POINT('Ctrl Pts',(-41.396226524684,-14.911486495888,18.));
#24255=CARTESIAN_POINT('Ctrl Pts',(-41.3758141263348,-14.9156446533966,
0.));
#24256=CARTESIAN_POINT('Ctrl Pts',(-41.3758141263348,-14.9156446533966,
18.));
#24257=CARTESIAN_POINT('Ctrl Pts',(-41.3349931861715,-14.9239113834707,
0.));
#24258=CARTESIAN_POINT('Ctrl Pts',(-41.3349931861715,-14.9239113834707,
18.));
#24259=CARTESIAN_POINT('Ctrl Pts',(-41.2737733455422,-14.936162723752,0.));
#24260=CARTESIAN_POINT('Ctrl Pts',(-41.2737733455422,-14.936162723752,18.));
#24261=CARTESIAN_POINT('Ctrl Pts',(-41.1921700381957,-14.9522002356298,
0.));
#24262=CARTESIAN_POINT('Ctrl Pts',(-41.1921700381957,-14.9522002356298,
18.));
#24263=CARTESIAN_POINT('Ctrl Pts',(-41.0902046498729,-14.9717503874227,
0.));
#24264=CARTESIAN_POINT('Ctrl Pts',(-41.0902046498729,-14.9717503874227,
18.));
#24265=CARTESIAN_POINT('Ctrl Pts',(-40.9882784321884,-14.9908026205824,
0.));
#24266=CARTESIAN_POINT('Ctrl Pts',(-40.9882784321884,-14.9908026205824,
18.));
#24267=CARTESIAN_POINT('Ctrl Pts',(-40.8863921801,-15.0093553188655,0.));
#24268=CARTESIAN_POINT('Ctrl Pts',(-40.8863921801,-15.0093553188655,18.));
#24269=CARTESIAN_POINT('Ctrl Pts',(-40.7845471608654,-15.0274064563211,
0.));
#24270=CARTESIAN_POINT('Ctrl Pts',(-40.7845471608654,-15.0274064563211,
18.));
#24271=CARTESIAN_POINT('Ctrl Pts',(-40.6827452453667,-15.0449536183143,
0.));
#24272=CARTESIAN_POINT('Ctrl Pts',(-40.6827452453667,-15.0449536183143,
18.));
#24273=CARTESIAN_POINT('Ctrl Pts',(-40.58098877043,-15.0619940893017,0.));
#24274=CARTESIAN_POINT('Ctrl Pts',(-40.58098877043,-15.0619940893017,18.));
#24275=CARTESIAN_POINT('Ctrl Pts',(-40.4792803645352,-15.0785249502524,
0.));
#24276=CARTESIAN_POINT('Ctrl Pts',(-40.4792803645352,-15.0785249502524,
18.));
#24277=CARTESIAN_POINT('Ctrl Pts',(-40.3776227809037,-15.0945431800723,
0.));
#24278=CARTESIAN_POINT('Ctrl Pts',(-40.3776227809037,-15.0945431800723,
18.));
#24279=CARTESIAN_POINT('Ctrl Pts',(-40.2760187401821,-15.1100457495259,
0.));
#24280=CARTESIAN_POINT('Ctrl Pts',(-40.2760187401821,-15.1100457495259,
18.));
#24281=CARTESIAN_POINT('Ctrl Pts',(-40.1744707357902,-15.1250297462408,
0.));
#24282=CARTESIAN_POINT('Ctrl Pts',(-40.1744707357902,-15.1250297462408,
18.));
#24283=CARTESIAN_POINT('Ctrl Pts',(-40.0729810652204,-15.1394923361537,
0.));
#24284=CARTESIAN_POINT('Ctrl Pts',(-40.0729810652204,-15.1394923361537,
18.));
#24285=CARTESIAN_POINT('Ctrl Pts',(-39.9715519332134,-15.1534306754871,
0.));
#24286=CARTESIAN_POINT('Ctrl Pts',(-39.9715519332134,-15.1534306754871,
18.));
#24287=CARTESIAN_POINT('Ctrl Pts',(-39.8701855339908,-15.1668418393198,
0.));
#24288=CARTESIAN_POINT('Ctrl Pts',(-39.8701855339908,-15.1668418393198,
18.));
#24289=CARTESIAN_POINT('Ctrl Pts',(-39.7688841338802,-15.1797227547561,
0.));
#24290=CARTESIAN_POINT('Ctrl Pts',(-39.7688841338802,-15.1797227547561,
18.));
#24291=CARTESIAN_POINT('Ctrl Pts',(-39.6676501731673,-15.1920701163803,
0.));
#24292=CARTESIAN_POINT('Ctrl Pts',(-39.6676501731673,-15.1920701163803,
18.));
#24293=CARTESIAN_POINT('Ctrl Pts',(-39.5664862602472,-15.2038804098649,
0.));
#24294=CARTESIAN_POINT('Ctrl Pts',(-39.5664862602472,-15.2038804098649,
18.));
#24295=CARTESIAN_POINT('Ctrl Pts',(-39.4653951093947,-15.2151499908149,
0.));
#24296=CARTESIAN_POINT('Ctrl Pts',(-39.4653951093947,-15.2151499908149,
18.));
#24297=CARTESIAN_POINT('Ctrl Pts',(-39.3643794927167,-15.2258751563069,
0.));
#24298=CARTESIAN_POINT('Ctrl Pts',(-39.3643794927167,-15.2258751563069,
18.));
#24299=CARTESIAN_POINT('Ctrl Pts',(-39.2634421927888,-15.2360522089072,
0.));
#24300=CARTESIAN_POINT('Ctrl Pts',(-39.2634421927888,-15.2360522089072,
18.));
#24301=CARTESIAN_POINT('Ctrl Pts',(-39.1625859371304,-15.2456775636447,
0.));
#24302=CARTESIAN_POINT('Ctrl Pts',(-39.1625859371304,-15.2456775636447,
18.));
#24303=CARTESIAN_POINT('Ctrl Pts',(-39.061813415425,-15.2547476855825,0.));
#24304=CARTESIAN_POINT('Ctrl Pts',(-39.061813415425,-15.2547476855825,18.));
#24305=CARTESIAN_POINT('Ctrl Pts',(-38.9611273555758,-15.2632589109473,
0.));
#24306=CARTESIAN_POINT('Ctrl Pts',(-38.9611273555758,-15.2632589109473,
18.));
#24307=CARTESIAN_POINT('Ctrl Pts',(-38.860530586589,-15.2712072937639,0.));
#24308=CARTESIAN_POINT('Ctrl Pts',(-38.860530586589,-15.2712072937639,18.));
#24309=CARTESIAN_POINT('Ctrl Pts',(-38.7600260961351,-15.2785884727112,
0.));
#24310=CARTESIAN_POINT('Ctrl Pts',(-38.7600260961351,-15.2785884727112,
18.));
#24311=CARTESIAN_POINT('Ctrl Pts',(-38.659617115053,-15.2853974668211,0.));
#24312=CARTESIAN_POINT('Ctrl Pts',(-38.659617115053,-15.2853974668211,18.));
#24313=CARTESIAN_POINT('Ctrl Pts',(-38.5593070891769,-15.2916287700102,
0.));
#24314=CARTESIAN_POINT('Ctrl Pts',(-38.5593070891769,-15.2916287700102,
18.));
#24315=CARTESIAN_POINT('Ctrl Pts',(-38.4590995527814,-15.2972767037469,
0.));
#24316=CARTESIAN_POINT('Ctrl Pts',(-38.4590995527814,-15.2972767037469,
18.));
#24317=CARTESIAN_POINT('Ctrl Pts',(-38.3589980188324,-15.3023357307483,
0.));
#24318=CARTESIAN_POINT('Ctrl Pts',(-38.3589980188324,-15.3023357307483,
18.));
#24319=CARTESIAN_POINT('Ctrl Pts',(-38.2590058835965,-15.3068007250314,
0.));
#24320=CARTESIAN_POINT('Ctrl Pts',(-38.2590058835965,-15.3068007250314,
18.));
#24321=CARTESIAN_POINT('Ctrl Pts',(-38.1591262705847,-15.310667421514,0.));
#24322=CARTESIAN_POINT('Ctrl Pts',(-38.1591262705847,-15.310667421514,18.));
#24323=CARTESIAN_POINT('Ctrl Pts',(-38.0593621055415,-15.3139321941687,
0.));
#24324=CARTESIAN_POINT('Ctrl Pts',(-38.0593621055415,-15.3139321941687,
18.));
#24325=CARTESIAN_POINT('Ctrl Pts',(-37.959716421934,-15.3165911656268,0.));
#24326=CARTESIAN_POINT('Ctrl Pts',(-37.959716421934,-15.3165911656268,18.));
#24327=CARTESIAN_POINT('Ctrl Pts',(-37.8601926265378,-15.3186394335023,
0.));
#24328=CARTESIAN_POINT('Ctrl Pts',(-37.8601926265378,-15.3186394335023,
18.));
#24329=CARTESIAN_POINT('Ctrl Pts',(-37.7607947318286,-15.320070396385,0.));
#24330=CARTESIAN_POINT('Ctrl Pts',(-37.7607947318286,-15.320070396385,18.));
#24331=CARTESIAN_POINT('Ctrl Pts',(-37.6615277218027,-15.320874689078,0.));
#24332=CARTESIAN_POINT('Ctrl Pts',(-37.6615277218027,-15.320874689078,18.));
#24333=CARTESIAN_POINT('Ctrl Pts',(-37.562397408596,-15.3210406145546,0.));
#24334=CARTESIAN_POINT('Ctrl Pts',(-37.562397408596,-15.3210406145546,18.));
#24335=CARTESIAN_POINT('Ctrl Pts',(-37.4634097578665,-15.3205561366169,
0.));
#24336=CARTESIAN_POINT('Ctrl Pts',(-37.4634097578665,-15.3205561366169,
18.));
#24337=CARTESIAN_POINT('Ctrl Pts',(-37.3645702997848,-15.3194106233801,
0.));
#24338=CARTESIAN_POINT('Ctrl Pts',(-37.3645702997848,-15.3194106233801,
18.));
#24339=CARTESIAN_POINT('Ctrl Pts',(-37.2658836214694,-15.3175963510697,
0.));
#24340=CARTESIAN_POINT('Ctrl Pts',(-37.2658836214694,-15.3175963510697,
18.));
#24341=CARTESIAN_POINT('Ctrl Pts',(-37.1673525354642,-15.3151109648809,
0.));
#24342=CARTESIAN_POINT('Ctrl Pts',(-37.1673525354642,-15.3151109648809,
18.));
#24343=CARTESIAN_POINT('Ctrl Pts',(-37.0689784837457,-15.3119562971444,
0.));
#24344=CARTESIAN_POINT('Ctrl Pts',(-37.0689784837457,-15.3119562971444,
18.));
#24345=CARTESIAN_POINT('Ctrl Pts',(-36.970763176802,-15.3081335446406,0.));
#24346=CARTESIAN_POINT('Ctrl Pts',(-36.970763176802,-15.3081335446406,18.));
#24347=CARTESIAN_POINT('Ctrl Pts',(-36.8727100302512,-15.3036390436952,
0.));
#24348=CARTESIAN_POINT('Ctrl Pts',(-36.8727100302512,-15.3036390436952,
18.));
#24349=CARTESIAN_POINT('Ctrl Pts',(-36.7748254044502,-15.2984606286737,
0.));
#24350=CARTESIAN_POINT('Ctrl Pts',(-36.7748254044502,-15.2984606286737,
18.));
#24351=CARTESIAN_POINT('Ctrl Pts',(-36.6771206167756,-15.2925717100767,
0.));
#24352=CARTESIAN_POINT('Ctrl Pts',(-36.6771206167756,-15.2925717100767,
18.));
#24353=CARTESIAN_POINT('Ctrl Pts',(-36.5796108931244,-15.2859343913094,
0.));
#24354=CARTESIAN_POINT('Ctrl Pts',(-36.5796108931244,-15.2859343913094,
18.));
#24355=CARTESIAN_POINT('Ctrl Pts',(-36.4823116513289,-15.2785104654792,
0.));
#24356=CARTESIAN_POINT('Ctrl Pts',(-36.4823116513289,-15.2785104654792,
18.));
#24357=CARTESIAN_POINT('Ctrl Pts',(-36.3852352131887,-15.2702711460937,
0.));
#24358=CARTESIAN_POINT('Ctrl Pts',(-36.3852352131887,-15.2702711460937,
18.));
#24359=CARTESIAN_POINT('Ctrl Pts',(-36.2883880151607,-15.2612053303773,
0.));
#24360=CARTESIAN_POINT('Ctrl Pts',(-36.2883880151607,-15.2612053303773,
18.));
#24361=CARTESIAN_POINT('Ctrl Pts',(-36.1917659216814,-15.2513334565427,
0.));
#24362=CARTESIAN_POINT('Ctrl Pts',(-36.1917659216814,-15.2513334565427,
18.));
#24363=CARTESIAN_POINT('Ctrl Pts',(-36.095357546697,-15.240697754828,0.));
#24364=CARTESIAN_POINT('Ctrl Pts',(-36.095357546697,-15.240697754828,18.));
#24365=CARTESIAN_POINT('Ctrl Pts',(-35.9991531408727,-15.2293360946131,
0.));
#24366=CARTESIAN_POINT('Ctrl Pts',(-35.9991531408727,-15.2293360946131,
18.));
#24367=CARTESIAN_POINT('Ctrl Pts',(-35.9031525499277,-15.2172585668056,
0.));
#24368=CARTESIAN_POINT('Ctrl Pts',(-35.9031525499277,-15.2172585668056,
18.));
#24369=CARTESIAN_POINT('Ctrl Pts',(-35.8073720252878,-15.2044274601769,
0.));
#24370=CARTESIAN_POINT('Ctrl Pts',(-35.8073720252878,-15.2044274601769,
18.));
#24371=CARTESIAN_POINT('Ctrl Pts',(-35.7118553943773,-15.1907243629658,
0.));
#24372=CARTESIAN_POINT('Ctrl Pts',(-35.7118553943773,-15.1907243629658,
18.));
#24373=CARTESIAN_POINT('Ctrl Pts',(-35.6166644736253,-15.1759785763051,
0.));
#24374=CARTESIAN_POINT('Ctrl Pts',(-35.6166644736253,-15.1759785763051,
18.));
#24375=CARTESIAN_POINT('Ctrl Pts',(-35.5218591529745,-15.1600260710383,
0.));
#24376=CARTESIAN_POINT('Ctrl Pts',(-35.5218591529745,-15.1600260710383,
18.));
#24377=CARTESIAN_POINT('Ctrl Pts',(-35.4274792115856,-15.1427632633831,
0.));
#24378=CARTESIAN_POINT('Ctrl Pts',(-35.4274792115856,-15.1427632633831,
18.));
#24379=CARTESIAN_POINT('Ctrl Pts',(-35.3335286891314,-15.1241934020681,
0.));
#24380=CARTESIAN_POINT('Ctrl Pts',(-35.3335286891314,-15.1241934020681,
18.));
#24381=CARTESIAN_POINT('Ctrl Pts',(-35.2399506932815,-15.104500806927,0.));
#24382=CARTESIAN_POINT('Ctrl Pts',(-35.2399506932815,-15.104500806927,18.));
#24383=CARTESIAN_POINT('Ctrl Pts',(-35.1466591020976,-15.08395927165,0.));
#24384=CARTESIAN_POINT('Ctrl Pts',(-35.1466591020976,-15.08395927165,18.));
#24385=CARTESIAN_POINT('Ctrl Pts',(-35.0535882932913,-15.0627878528202,
0.));
#24386=CARTESIAN_POINT('Ctrl Pts',(-35.0535882932913,-15.0627878528202,
18.));
#24387=CARTESIAN_POINT('Ctrl Pts',(-34.9607388363587,-15.041018569143,0.));
#24388=CARTESIAN_POINT('Ctrl Pts',(-34.9607388363587,-15.041018569143,18.));
#24389=CARTESIAN_POINT('Ctrl Pts',(-34.8682205930809,-15.0183713484962,
0.));
#24390=CARTESIAN_POINT('Ctrl Pts',(-34.8682205930809,-15.0183713484962,
18.));
#24391=CARTESIAN_POINT('Ctrl Pts',(-34.7763085406486,-14.9940927023321,
0.));
#24392=CARTESIAN_POINT('Ctrl Pts',(-34.7763085406486,-14.9940927023321,
18.));
#24393=CARTESIAN_POINT('Ctrl Pts',(-34.6853717911268,-14.9671565602316,
0.));
#24394=CARTESIAN_POINT('Ctrl Pts',(-34.6853717911268,-14.9671565602316,
18.));
#24395=CARTESIAN_POINT('Ctrl Pts',(-34.6137007885254,-14.9426481276593,
0.));
#24396=CARTESIAN_POINT('Ctrl Pts',(-34.6137007885254,-14.9426481276593,
18.));
#24397=CARTESIAN_POINT('Ctrl Pts',(-34.5606858566713,-14.9222326355678,
0.));
#24398=CARTESIAN_POINT('Ctrl Pts',(-34.5606858566713,-14.9222326355678,
18.));
#24399=CARTESIAN_POINT('Ctrl Pts',(-34.525687510388,-14.9076710061311,0.));
#24400=CARTESIAN_POINT('Ctrl Pts',(-34.525687510388,-14.9076710061311,18.));
#24401=CARTESIAN_POINT('Ctrl Pts',(-34.5082745737944,-14.9001523628048,
0.));
#24402=CARTESIAN_POINT('Ctrl Pts',(-34.5082745737944,-14.9001523628048,
18.));
#24403=CARTESIAN_POINT('',(-41.3962265246839,-14.9114864958881,0.));
#24404=CARTESIAN_POINT('Ctrl Pts',(-34.5082745737944,-14.9001523628048,
0.));
#24405=CARTESIAN_POINT('Ctrl Pts',(-34.525687510388,-14.9076710061311,0.));
#24406=CARTESIAN_POINT('Ctrl Pts',(-34.5606858566713,-14.9222326355678,
0.));
#24407=CARTESIAN_POINT('Ctrl Pts',(-34.6137007885254,-14.9426481276593,
0.));
#24408=CARTESIAN_POINT('Ctrl Pts',(-34.6853717911268,-14.9671565602316,
0.));
#24409=CARTESIAN_POINT('Ctrl Pts',(-34.7763085406486,-14.9940927023321,
0.));
#24410=CARTESIAN_POINT('Ctrl Pts',(-34.8682205930809,-15.0183713484962,
0.));
#24411=CARTESIAN_POINT('Ctrl Pts',(-34.9607388363587,-15.041018569143,0.));
#24412=CARTESIAN_POINT('Ctrl Pts',(-35.0535882932913,-15.0627878528202,
0.));
#24413=CARTESIAN_POINT('Ctrl Pts',(-35.1466591020976,-15.08395927165,0.));
#24414=CARTESIAN_POINT('Ctrl Pts',(-35.2399506932815,-15.104500806927,0.));
#24415=CARTESIAN_POINT('Ctrl Pts',(-35.3335286891314,-15.1241934020681,
0.));
#24416=CARTESIAN_POINT('Ctrl Pts',(-35.4274792115856,-15.1427632633831,
0.));
#24417=CARTESIAN_POINT('Ctrl Pts',(-35.5218591529745,-15.1600260710383,
0.));
#24418=CARTESIAN_POINT('Ctrl Pts',(-35.6166644736253,-15.1759785763051,
0.));
#24419=CARTESIAN_POINT('Ctrl Pts',(-35.7118553943773,-15.1907243629658,
0.));
#24420=CARTESIAN_POINT('Ctrl Pts',(-35.8073720252878,-15.2044274601769,
0.));
#24421=CARTESIAN_POINT('Ctrl Pts',(-35.9031525499277,-15.2172585668056,
0.));
#24422=CARTESIAN_POINT('Ctrl Pts',(-35.9991531408727,-15.2293360946131,
0.));
#24423=CARTESIAN_POINT('Ctrl Pts',(-36.095357546697,-15.240697754828,0.));
#24424=CARTESIAN_POINT('Ctrl Pts',(-36.1917659216814,-15.2513334565427,
0.));
#24425=CARTESIAN_POINT('Ctrl Pts',(-36.2883880151607,-15.2612053303773,
0.));
#24426=CARTESIAN_POINT('Ctrl Pts',(-36.3852352131887,-15.2702711460937,
0.));
#24427=CARTESIAN_POINT('Ctrl Pts',(-36.4823116513289,-15.2785104654792,
0.));
#24428=CARTESIAN_POINT('Ctrl Pts',(-36.5796108931244,-15.2859343913094,
0.));
#24429=CARTESIAN_POINT('Ctrl Pts',(-36.6771206167756,-15.2925717100767,
0.));
#24430=CARTESIAN_POINT('Ctrl Pts',(-36.7748254044502,-15.2984606286737,
0.));
#24431=CARTESIAN_POINT('Ctrl Pts',(-36.8727100302512,-15.3036390436952,
0.));
#24432=CARTESIAN_POINT('Ctrl Pts',(-36.970763176802,-15.3081335446406,0.));
#24433=CARTESIAN_POINT('Ctrl Pts',(-37.0689784837457,-15.3119562971444,
0.));
#24434=CARTESIAN_POINT('Ctrl Pts',(-37.1673525354642,-15.3151109648809,
0.));
#24435=CARTESIAN_POINT('Ctrl Pts',(-37.2658836214694,-15.3175963510697,
0.));
#24436=CARTESIAN_POINT('Ctrl Pts',(-37.3645702997848,-15.3194106233801,
0.));
#24437=CARTESIAN_POINT('Ctrl Pts',(-37.4634097578665,-15.3205561366169,
0.));
#24438=CARTESIAN_POINT('Ctrl Pts',(-37.562397408596,-15.3210406145546,0.));
#24439=CARTESIAN_POINT('Ctrl Pts',(-37.6615277218027,-15.320874689078,0.));
#24440=CARTESIAN_POINT('Ctrl Pts',(-37.7607947318286,-15.320070396385,0.));
#24441=CARTESIAN_POINT('Ctrl Pts',(-37.8601926265378,-15.3186394335023,
0.));
#24442=CARTESIAN_POINT('Ctrl Pts',(-37.959716421934,-15.3165911656268,0.));
#24443=CARTESIAN_POINT('Ctrl Pts',(-38.0593621055415,-15.3139321941687,
0.));
#24444=CARTESIAN_POINT('Ctrl Pts',(-38.1591262705847,-15.310667421514,0.));
#24445=CARTESIAN_POINT('Ctrl Pts',(-38.2590058835965,-15.3068007250314,
0.));
#24446=CARTESIAN_POINT('Ctrl Pts',(-38.3589980188324,-15.3023357307483,
0.));
#24447=CARTESIAN_POINT('Ctrl Pts',(-38.4590995527814,-15.2972767037469,
0.));
#24448=CARTESIAN_POINT('Ctrl Pts',(-38.5593070891769,-15.2916287700102,
0.));
#24449=CARTESIAN_POINT('Ctrl Pts',(-38.659617115053,-15.2853974668211,0.));
#24450=CARTESIAN_POINT('Ctrl Pts',(-38.7600260961351,-15.2785884727112,
0.));
#24451=CARTESIAN_POINT('Ctrl Pts',(-38.860530586589,-15.2712072937639,0.));
#24452=CARTESIAN_POINT('Ctrl Pts',(-38.9611273555758,-15.2632589109473,
0.));
#24453=CARTESIAN_POINT('Ctrl Pts',(-39.061813415425,-15.2547476855825,0.));
#24454=CARTESIAN_POINT('Ctrl Pts',(-39.1625859371304,-15.2456775636447,
0.));
#24455=CARTESIAN_POINT('Ctrl Pts',(-39.2634421927888,-15.2360522089072,
0.));
#24456=CARTESIAN_POINT('Ctrl Pts',(-39.3643794927167,-15.2258751563069,
0.));
#24457=CARTESIAN_POINT('Ctrl Pts',(-39.4653951093947,-15.2151499908149,
0.));
#24458=CARTESIAN_POINT('Ctrl Pts',(-39.5664862602472,-15.2038804098649,
0.));
#24459=CARTESIAN_POINT('Ctrl Pts',(-39.6676501731673,-15.1920701163803,
0.));
#24460=CARTESIAN_POINT('Ctrl Pts',(-39.7688841338802,-15.1797227547561,
0.));
#24461=CARTESIAN_POINT('Ctrl Pts',(-39.8701855339908,-15.1668418393198,
0.));
#24462=CARTESIAN_POINT('Ctrl Pts',(-39.9715519332134,-15.1534306754871,
0.));
#24463=CARTESIAN_POINT('Ctrl Pts',(-40.0729810652204,-15.1394923361537,
0.));
#24464=CARTESIAN_POINT('Ctrl Pts',(-40.1744707357902,-15.1250297462408,
0.));
#24465=CARTESIAN_POINT('Ctrl Pts',(-40.2760187401821,-15.1100457495259,
0.));
#24466=CARTESIAN_POINT('Ctrl Pts',(-40.3776227809037,-15.0945431800723,
0.));
#24467=CARTESIAN_POINT('Ctrl Pts',(-40.4792803645352,-15.0785249502524,
0.));
#24468=CARTESIAN_POINT('Ctrl Pts',(-40.58098877043,-15.0619940893017,0.));
#24469=CARTESIAN_POINT('Ctrl Pts',(-40.6827452453667,-15.0449536183143,
0.));
#24470=CARTESIAN_POINT('Ctrl Pts',(-40.7845471608654,-15.0274064563211,
0.));
#24471=CARTESIAN_POINT('Ctrl Pts',(-40.8863921801,-15.0093553188655,0.));
#24472=CARTESIAN_POINT('Ctrl Pts',(-40.9882784321884,-14.9908026205824,
0.));
#24473=CARTESIAN_POINT('Ctrl Pts',(-41.1105898934098,-14.9679399407908,
0.));
#24474=CARTESIAN_POINT('Ctrl Pts',(-41.2125650743922,-14.9482653093396,
0.));
#24475=CARTESIAN_POINT('Ctrl Pts',(-41.2941761025922,-14.9321285285561,
0.));
#24476=CARTESIAN_POINT('Ctrl Pts',(-41.3554017279611,-14.919802810928,0.));
#24477=CARTESIAN_POINT('Ctrl Pts',(-41.396226524684,-14.911486495888,0.));
#24478=CARTESIAN_POINT('',(-41.3962265246839,-14.9114864958881,15.));
#24479=CARTESIAN_POINT('Ctrl Pts',(-41.396226524684,-14.911486495888,15.));
#24480=CARTESIAN_POINT('Ctrl Pts',(-41.3758141263348,-14.9156446533966,
15.));
#24481=CARTESIAN_POINT('Ctrl Pts',(-41.3349931861715,-14.9239113834707,
15.));
#24482=CARTESIAN_POINT('Ctrl Pts',(-41.2737733455422,-14.936162723752,15.));
#24483=CARTESIAN_POINT('Ctrl Pts',(-41.1921700381957,-14.9522002356298,
15.));
#24484=CARTESIAN_POINT('Ctrl Pts',(-41.0902046498729,-14.9717503874227,
15.));
#24485=CARTESIAN_POINT('Ctrl Pts',(-40.9882784321884,-14.9908026205824,
15.));
#24486=CARTESIAN_POINT('Ctrl Pts',(-40.8863921801,-15.0093553188655,15.));
#24487=CARTESIAN_POINT('Ctrl Pts',(-40.7845471608654,-15.0274064563211,
15.));
#24488=CARTESIAN_POINT('Ctrl Pts',(-40.6827452453667,-15.0449536183143,
15.));
#24489=CARTESIAN_POINT('Ctrl Pts',(-40.58098877043,-15.0619940893017,15.));
#24490=CARTESIAN_POINT('Ctrl Pts',(-40.4792803645352,-15.0785249502524,
15.));
#24491=CARTESIAN_POINT('Ctrl Pts',(-40.3776227809037,-15.0945431800723,
15.));
#24492=CARTESIAN_POINT('Ctrl Pts',(-40.2760187401821,-15.1100457495259,
15.));
#24493=CARTESIAN_POINT('Ctrl Pts',(-40.1744707357902,-15.1250297462408,
15.));
#24494=CARTESIAN_POINT('Ctrl Pts',(-40.0729810652204,-15.1394923361537,
15.));
#24495=CARTESIAN_POINT('Ctrl Pts',(-39.9715519332134,-15.1534306754871,
15.));
#24496=CARTESIAN_POINT('Ctrl Pts',(-39.8701855339908,-15.1668418393198,
15.));
#24497=CARTESIAN_POINT('Ctrl Pts',(-39.7688841338802,-15.1797227547561,
15.));
#24498=CARTESIAN_POINT('Ctrl Pts',(-39.6676501731673,-15.1920701163803,
15.));
#24499=CARTESIAN_POINT('Ctrl Pts',(-39.5664862602472,-15.2038804098649,
15.));
#24500=CARTESIAN_POINT('Ctrl Pts',(-39.4653951093947,-15.2151499908149,
15.));
#24501=CARTESIAN_POINT('Ctrl Pts',(-39.3643794927167,-15.2258751563069,
15.));
#24502=CARTESIAN_POINT('Ctrl Pts',(-39.2634421927888,-15.2360522089072,
15.));
#24503=CARTESIAN_POINT('Ctrl Pts',(-39.1625859371304,-15.2456775636447,
15.));
#24504=CARTESIAN_POINT('Ctrl Pts',(-39.061813415425,-15.2547476855825,15.));
#24505=CARTESIAN_POINT('Ctrl Pts',(-38.9611273555758,-15.2632589109473,
15.));
#24506=CARTESIAN_POINT('Ctrl Pts',(-38.860530586589,-15.2712072937639,15.));
#24507=CARTESIAN_POINT('Ctrl Pts',(-38.7600260961351,-15.2785884727112,
15.));
#24508=CARTESIAN_POINT('Ctrl Pts',(-38.659617115053,-15.2853974668211,15.));
#24509=CARTESIAN_POINT('Ctrl Pts',(-38.5593070891769,-15.2916287700102,
15.));
#24510=CARTESIAN_POINT('Ctrl Pts',(-38.4590995527814,-15.2972767037469,
15.));
#24511=CARTESIAN_POINT('Ctrl Pts',(-38.3589980188324,-15.3023357307483,
15.));
#24512=CARTESIAN_POINT('Ctrl Pts',(-38.2590058835965,-15.3068007250314,
15.));
#24513=CARTESIAN_POINT('Ctrl Pts',(-38.1591262705847,-15.310667421514,15.));
#24514=CARTESIAN_POINT('Ctrl Pts',(-38.0593621055415,-15.3139321941687,
15.));
#24515=CARTESIAN_POINT('Ctrl Pts',(-37.959716421934,-15.3165911656268,15.));
#24516=CARTESIAN_POINT('Ctrl Pts',(-37.8601926265378,-15.3186394335023,
15.));
#24517=CARTESIAN_POINT('Ctrl Pts',(-37.7607947318286,-15.320070396385,15.));
#24518=CARTESIAN_POINT('Ctrl Pts',(-37.6615277218027,-15.320874689078,15.));
#24519=CARTESIAN_POINT('Ctrl Pts',(-37.562397408596,-15.3210406145546,15.));
#24520=CARTESIAN_POINT('Ctrl Pts',(-37.4634097578665,-15.3205561366169,
15.));
#24521=CARTESIAN_POINT('Ctrl Pts',(-37.3645702997848,-15.3194106233801,
15.));
#24522=CARTESIAN_POINT('Ctrl Pts',(-37.2658836214694,-15.3175963510697,
15.));
#24523=CARTESIAN_POINT('Ctrl Pts',(-37.1673525354642,-15.3151109648809,
15.));
#24524=CARTESIAN_POINT('Ctrl Pts',(-37.0689784837457,-15.3119562971444,
15.));
#24525=CARTESIAN_POINT('Ctrl Pts',(-36.970763176802,-15.3081335446406,15.));
#24526=CARTESIAN_POINT('Ctrl Pts',(-36.8727100302512,-15.3036390436952,
15.));
#24527=CARTESIAN_POINT('Ctrl Pts',(-36.7748254044502,-15.2984606286737,
15.));
#24528=CARTESIAN_POINT('Ctrl Pts',(-36.6771206167756,-15.2925717100767,
15.));
#24529=CARTESIAN_POINT('Ctrl Pts',(-36.5796108931244,-15.2859343913094,
15.));
#24530=CARTESIAN_POINT('Ctrl Pts',(-36.4823116513289,-15.2785104654792,
15.));
#24531=CARTESIAN_POINT('Ctrl Pts',(-36.3852352131887,-15.2702711460937,
15.));
#24532=CARTESIAN_POINT('Ctrl Pts',(-36.2883880151607,-15.2612053303773,
15.));
#24533=CARTESIAN_POINT('Ctrl Pts',(-36.1917659216814,-15.2513334565427,
15.));
#24534=CARTESIAN_POINT('Ctrl Pts',(-36.095357546697,-15.240697754828,15.));
#24535=CARTESIAN_POINT('Ctrl Pts',(-35.9991531408727,-15.2293360946131,
15.));
#24536=CARTESIAN_POINT('Ctrl Pts',(-35.9031525499277,-15.2172585668056,
15.));
#24537=CARTESIAN_POINT('Ctrl Pts',(-35.8073720252878,-15.2044274601769,
15.));
#24538=CARTESIAN_POINT('Ctrl Pts',(-35.7118553943773,-15.1907243629658,
15.));
#24539=CARTESIAN_POINT('Ctrl Pts',(-35.6166644736253,-15.1759785763051,
15.));
#24540=CARTESIAN_POINT('Ctrl Pts',(-35.5218591529745,-15.1600260710383,
15.));
#24541=CARTESIAN_POINT('Ctrl Pts',(-35.4274792115856,-15.1427632633831,
15.));
#24542=CARTESIAN_POINT('Ctrl Pts',(-35.3335286891314,-15.1241934020681,
15.));
#24543=CARTESIAN_POINT('Ctrl Pts',(-35.2399506932815,-15.104500806927,15.));
#24544=CARTESIAN_POINT('Ctrl Pts',(-35.1466591020976,-15.08395927165,15.));
#24545=CARTESIAN_POINT('Ctrl Pts',(-35.0535882932913,-15.0627878528202,
15.));
#24546=CARTESIAN_POINT('Ctrl Pts',(-34.9607388363587,-15.041018569143,15.));
#24547=CARTESIAN_POINT('Ctrl Pts',(-34.8682205930809,-15.0183713484962,
15.));
#24548=CARTESIAN_POINT('Ctrl Pts',(-34.7763085406486,-14.9940927023321,
15.));
#24549=CARTESIAN_POINT('Ctrl Pts',(-34.6853717911268,-14.9671565602316,
15.));
#24550=CARTESIAN_POINT('Ctrl Pts',(-34.6137007885254,-14.9426481276593,
15.));
#24551=CARTESIAN_POINT('Ctrl Pts',(-34.5606858566713,-14.9222326355678,
15.));
#24552=CARTESIAN_POINT('Ctrl Pts',(-34.525687510388,-14.9076710061311,15.));
#24553=CARTESIAN_POINT('Ctrl Pts',(-34.5082745737944,-14.9001523628048,
15.));
#24554=CARTESIAN_POINT('',(-41.3962265246839,-14.9114864958881,0.));
#24555=CARTESIAN_POINT('Origin',(-1.07784724682657E-11,-3.50213800024364E-12,
0.));
#24556=CARTESIAN_POINT('',(-42.2550026135057,-12.2684454652018,0.));
#24557=CARTESIAN_POINT('Origin',(-1.07784724682657E-11,-3.50213800024364E-12,
0.));
#24558=CARTESIAN_POINT('',(-42.2550026135057,-12.2684454652018,15.));
#24559=CARTESIAN_POINT('Origin',(-1.07784724682657E-11,-3.50213800024364E-12,
15.));
#24560=CARTESIAN_POINT('',(-42.2550026135057,-12.2684454652018,0.));
#24561=CARTESIAN_POINT('Ctrl Pts',(-36.6758703925241,-8.2289783962506,0.));
#24562=CARTESIAN_POINT('Ctrl Pts',(-36.6758703925241,-8.2289783962506,18.));
#24563=CARTESIAN_POINT('Ctrl Pts',(-36.6943771018148,-8.23313075335376,
0.));
#24564=CARTESIAN_POINT('Ctrl Pts',(-36.6943771018148,-8.23313075335376,
18.));
#24565=CARTESIAN_POINT('Ctrl Pts',(-36.7312504697652,-8.24192165947367,
0.));
#24566=CARTESIAN_POINT('Ctrl Pts',(-36.7312504697652,-8.24192165947367,
18.));
#24567=CARTESIAN_POINT('Ctrl Pts',(-36.7861403757604,-8.2565665745182,0.));
#24568=CARTESIAN_POINT('Ctrl Pts',(-36.7861403757604,-8.2565665745182,18.));
#24569=CARTESIAN_POINT('Ctrl Pts',(-36.8585291300917,-8.27886599440784,
0.));
#24570=CARTESIAN_POINT('Ctrl Pts',(-36.8585291300917,-8.27886599440784,
18.));
#24571=CARTESIAN_POINT('Ctrl Pts',(-36.9479311729484,-8.31052547794591,
0.));
#24572=CARTESIAN_POINT('Ctrl Pts',(-36.9479311729484,-8.31052547794591,
18.));
#24573=CARTESIAN_POINT('Ctrl Pts',(-37.0365602155148,-8.34490818952639,
0.));
#24574=CARTESIAN_POINT('Ctrl Pts',(-37.0365602155148,-8.34490818952639,
18.));
#24575=CARTESIAN_POINT('Ctrl Pts',(-37.1247207489179,-8.38096706211447,
0.));
#24576=CARTESIAN_POINT('Ctrl Pts',(-37.1247207489179,-8.38096706211447,
18.));
#24577=CARTESIAN_POINT('Ctrl Pts',(-37.2126332013933,-8.41793088313259,
0.));
#24578=CARTESIAN_POINT('Ctrl Pts',(-37.2126332013933,-8.41793088313259,
18.));
#24579=CARTESIAN_POINT('Ctrl Pts',(-37.3003733151561,-8.45550849433959,
0.));
#24580=CARTESIAN_POINT('Ctrl Pts',(-37.3003733151561,-8.45550849433959,
18.));
#24581=CARTESIAN_POINT('Ctrl Pts',(-37.3879218093514,-8.49372546467075,
0.));
#24582=CARTESIAN_POINT('Ctrl Pts',(-37.3879218093514,-8.49372546467075,
18.));
#24583=CARTESIAN_POINT('Ctrl Pts',(-37.4752030152968,-8.53279758643783,
0.));
#24584=CARTESIAN_POINT('Ctrl Pts',(-37.4752030152968,-8.53279758643783,
18.));
#24585=CARTESIAN_POINT('Ctrl Pts',(-37.5621256752108,-8.57299698459465,
0.));
#24586=CARTESIAN_POINT('Ctrl Pts',(-37.5621256752108,-8.57299698459465,
18.));
#24587=CARTESIAN_POINT('Ctrl Pts',(-37.6486274754754,-8.61450621749154,
0.));
#24588=CARTESIAN_POINT('Ctrl Pts',(-37.6486274754754,-8.61450621749154,
18.));
#24589=CARTESIAN_POINT('Ctrl Pts',(-37.7347032383719,-8.65732553894524,
0.));
#24590=CARTESIAN_POINT('Ctrl Pts',(-37.7347032383719,-8.65732553894524,
18.));
#24591=CARTESIAN_POINT('Ctrl Pts',(-37.8203816669031,-8.70134776631143,
0.));
#24592=CARTESIAN_POINT('Ctrl Pts',(-37.8203816669031,-8.70134776631143,
18.));
#24593=CARTESIAN_POINT('Ctrl Pts',(-37.9057107230066,-8.74640499479002,
0.));
#24594=CARTESIAN_POINT('Ctrl Pts',(-37.9057107230066,-8.74640499479002,
18.));
#24595=CARTESIAN_POINT('Ctrl Pts',(-37.9907407304174,-8.79232279131091,
0.));
#24596=CARTESIAN_POINT('Ctrl Pts',(-37.9907407304174,-8.79232279131091,
18.));
#24597=CARTESIAN_POINT('Ctrl Pts',(-38.0755058326913,-8.83897959763348,
0.));
#24598=CARTESIAN_POINT('Ctrl Pts',(-38.0755058326913,-8.83897959763348,
18.));
#24599=CARTESIAN_POINT('Ctrl Pts',(-38.1600150482528,-8.88633535238434,
0.));
#24600=CARTESIAN_POINT('Ctrl Pts',(-38.1600150482528,-8.88633535238434,
18.));
#24601=CARTESIAN_POINT('Ctrl Pts',(-38.2442625706309,-8.93439830996338,
0.));
#24602=CARTESIAN_POINT('Ctrl Pts',(-38.2442625706309,-8.93439830996338,
18.));
#24603=CARTESIAN_POINT('Ctrl Pts',(-38.3282340281403,-8.98320483785759,
0.));
#24604=CARTESIAN_POINT('Ctrl Pts',(-38.3282340281403,-8.98320483785759,
18.));
#24605=CARTESIAN_POINT('Ctrl Pts',(-38.4119138099805,-9.0327957936019,0.));
#24606=CARTESIAN_POINT('Ctrl Pts',(-38.4119138099805,-9.0327957936019,18.));
#24607=CARTESIAN_POINT('Ctrl Pts',(-38.4952932486131,-9.08319014288085,
0.));
#24608=CARTESIAN_POINT('Ctrl Pts',(-38.4952932486131,-9.08319014288085,
18.));
#24609=CARTESIAN_POINT('Ctrl Pts',(-38.5783736628826,-9.13437512010585,
0.));
#24610=CARTESIAN_POINT('Ctrl Pts',(-38.5783736628826,-9.13437512010585,
18.));
#24611=CARTESIAN_POINT('Ctrl Pts',(-38.6611620045193,-9.18632019394329,
0.));
#24612=CARTESIAN_POINT('Ctrl Pts',(-38.6611620045193,-9.18632019394329,
18.));
#24613=CARTESIAN_POINT('Ctrl Pts',(-38.7436682576832,-9.23898539199331,
0.));
#24614=CARTESIAN_POINT('Ctrl Pts',(-38.7436682576832,-9.23898539199331,
18.));
#24615=CARTESIAN_POINT('Ctrl Pts',(-38.8259023794241,-9.29233110570902,
0.));
#24616=CARTESIAN_POINT('Ctrl Pts',(-38.8259023794241,-9.29233110570902,
18.));
#24617=CARTESIAN_POINT('Ctrl Pts',(-38.9078708427078,-9.34632917154636,
0.));
#24618=CARTESIAN_POINT('Ctrl Pts',(-38.9078708427078,-9.34632917154636,
18.));
#24619=CARTESIAN_POINT('Ctrl Pts',(-38.9895756526779,-9.40096600877643,
0.));
#24620=CARTESIAN_POINT('Ctrl Pts',(-38.9895756526779,-9.40096600877643,
18.));
#24621=CARTESIAN_POINT('Ctrl Pts',(-39.0710161994951,-9.45623664577431,
0.));
#24622=CARTESIAN_POINT('Ctrl Pts',(-39.0710161994951,-9.45623664577431,
18.));
#24623=CARTESIAN_POINT('Ctrl Pts',(-39.1521903958955,-9.5121410453562,0.));
#24624=CARTESIAN_POINT('Ctrl Pts',(-39.1521903958955,-9.5121410453562,18.));
#24625=CARTESIAN_POINT('Ctrl Pts',(-39.2330959982788,-9.56867984233622,
0.));
#24626=CARTESIAN_POINT('Ctrl Pts',(-39.2330959982788,-9.56867984233622,
18.));
#24627=CARTESIAN_POINT('Ctrl Pts',(-39.3137321153686,-9.62584947846543,
0.));
#24628=CARTESIAN_POINT('Ctrl Pts',(-39.3137321153686,-9.62584947846543,
18.));
#24629=CARTESIAN_POINT('Ctrl Pts',(-39.3940995760289,-9.68364100883826,
0.));
#24630=CARTESIAN_POINT('Ctrl Pts',(-39.3940995760289,-9.68364100883826,
18.));
#24631=CARTESIAN_POINT('Ctrl Pts',(-39.4742001555227,-9.74204258152662,
0.));
#24632=CARTESIAN_POINT('Ctrl Pts',(-39.4742001555227,-9.74204258152662,
18.));
#24633=CARTESIAN_POINT('Ctrl Pts',(-39.5540361022309,-9.80104095251613,
0.));
#24634=CARTESIAN_POINT('Ctrl Pts',(-39.5540361022309,-9.80104095251613,
18.));
#24635=CARTESIAN_POINT('Ctrl Pts',(-39.6336095893767,-9.86062324242559,
0.));
#24636=CARTESIAN_POINT('Ctrl Pts',(-39.6336095893767,-9.86062324242559,
18.));
#24637=CARTESIAN_POINT('Ctrl Pts',(-39.712922089547,-9.92077894513191,0.));
#24638=CARTESIAN_POINT('Ctrl Pts',(-39.712922089547,-9.92077894513191,18.));
#24639=CARTESIAN_POINT('Ctrl Pts',(-39.7919742367922,-9.98150036150822,
0.));
#24640=CARTESIAN_POINT('Ctrl Pts',(-39.7919742367922,-9.98150036150822,
18.));
#24641=CARTESIAN_POINT('Ctrl Pts',(-39.8707661565233,-10.0427815229883,
0.));
#24642=CARTESIAN_POINT('Ctrl Pts',(-39.8707661565233,-10.0427815229883,
18.));
#24643=CARTESIAN_POINT('Ctrl Pts',(-39.9492976736738,-10.1046175096878,
0.));
#24644=CARTESIAN_POINT('Ctrl Pts',(-39.9492976736738,-10.1046175096878,
18.));
#24645=CARTESIAN_POINT('Ctrl Pts',(-40.0275685525923,-10.1670036683795,
0.));
#24646=CARTESIAN_POINT('Ctrl Pts',(-40.0275685525923,-10.1670036683795,
18.));
#24647=CARTESIAN_POINT('Ctrl Pts',(-40.1055787732578,-10.2299347125857,
0.));
#24648=CARTESIAN_POINT('Ctrl Pts',(-40.1055787732578,-10.2299347125857,
18.));
#24649=CARTESIAN_POINT('Ctrl Pts',(-40.1833286010098,-10.2934044990237,
0.));
#24650=CARTESIAN_POINT('Ctrl Pts',(-40.1833286010098,-10.2934044990237,
18.));
#24651=CARTESIAN_POINT('Ctrl Pts',(-40.2608184485326,-10.3574064830678,
0.));
#24652=CARTESIAN_POINT('Ctrl Pts',(-40.2608184485326,-10.3574064830678,
18.));
#24653=CARTESIAN_POINT('Ctrl Pts',(-40.3380487942952,-10.421933993295,0.));
#24654=CARTESIAN_POINT('Ctrl Pts',(-40.3380487942952,-10.421933993295,18.));
#24655=CARTESIAN_POINT('Ctrl Pts',(-40.4150200869536,-10.48698054978,0.));
#24656=CARTESIAN_POINT('Ctrl Pts',(-40.4150200869536,-10.48698054978,18.));
#24657=CARTESIAN_POINT('Ctrl Pts',(-40.4917326404439,-10.5525402237951,
0.));
#24658=CARTESIAN_POINT('Ctrl Pts',(-40.4917326404439,-10.5525402237951,
18.));
#24659=CARTESIAN_POINT('Ctrl Pts',(-40.5681866012103,-10.618607730849,0.));
#24660=CARTESIAN_POINT('Ctrl Pts',(-40.5681866012103,-10.618607730849,18.));
#24661=CARTESIAN_POINT('Ctrl Pts',(-40.6443819999244,-10.6851782157325,
0.));
#24662=CARTESIAN_POINT('Ctrl Pts',(-40.6443819999244,-10.6851782157325,
18.));
#24663=CARTESIAN_POINT('Ctrl Pts',(-40.7203187831783,-10.7522471109694,
0.));
#24664=CARTESIAN_POINT('Ctrl Pts',(-40.7203187831783,-10.7522471109694,
18.));
#24665=CARTESIAN_POINT('Ctrl Pts',(-40.7959968527561,-10.8198099757795,
0.));
#24666=CARTESIAN_POINT('Ctrl Pts',(-40.7959968527561,-10.8198099757795,
18.));
#24667=CARTESIAN_POINT('Ctrl Pts',(-40.8714161092412,-10.8878623066646,
0.));
#24668=CARTESIAN_POINT('Ctrl Pts',(-40.8714161092412,-10.8878623066646,
18.));
#24669=CARTESIAN_POINT('Ctrl Pts',(-40.9465764747798,-10.956399476781,0.));
#24670=CARTESIAN_POINT('Ctrl Pts',(-40.9465764747798,-10.956399476781,18.));
#24671=CARTESIAN_POINT('Ctrl Pts',(-41.0214778832142,-11.0254168609972,
0.));
#24672=CARTESIAN_POINT('Ctrl Pts',(-41.0214778832142,-11.0254168609972,
18.));
#24673=CARTESIAN_POINT('Ctrl Pts',(-41.0961202807715,-11.0949099155251,
0.));
#24674=CARTESIAN_POINT('Ctrl Pts',(-41.0961202807715,-11.0949099155251,
18.));
#24675=CARTESIAN_POINT('Ctrl Pts',(-41.1705036228854,-11.1648742640378,
0.));
#24676=CARTESIAN_POINT('Ctrl Pts',(-41.1705036228854,-11.1648742640378,
18.));
#24677=CARTESIAN_POINT('Ctrl Pts',(-41.2446278781981,-11.2353057980338,
0.));
#24678=CARTESIAN_POINT('Ctrl Pts',(-41.2446278781981,-11.2353057980338,
18.));
#24679=CARTESIAN_POINT('Ctrl Pts',(-41.3184930194148,-11.3062006993745,
0.));
#24680=CARTESIAN_POINT('Ctrl Pts',(-41.3184930194148,-11.3062006993745,
18.));
#24681=CARTESIAN_POINT('Ctrl Pts',(-41.3920989905986,-11.3775553120176,
0.));
#24682=CARTESIAN_POINT('Ctrl Pts',(-41.3920989905986,-11.3775553120176,
18.));
#24683=CARTESIAN_POINT('Ctrl Pts',(-41.4654456796071,-11.4493660393849,
0.));
#24684=CARTESIAN_POINT('Ctrl Pts',(-41.4654456796071,-11.4493660393849,
18.));
#24685=CARTESIAN_POINT('Ctrl Pts',(-41.5385328935506,-11.5216292382388,
0.));
#24686=CARTESIAN_POINT('Ctrl Pts',(-41.5385328935506,-11.5216292382388,
18.));
#24687=CARTESIAN_POINT('Ctrl Pts',(-41.6113603270596,-11.5943410868252,
0.));
#24688=CARTESIAN_POINT('Ctrl Pts',(-41.6113603270596,-11.5943410868252,
18.));
#24689=CARTESIAN_POINT('Ctrl Pts',(-41.6839275596248,-11.6674975352851,
0.));
#24690=CARTESIAN_POINT('Ctrl Pts',(-41.6839275596248,-11.6674975352851,
18.));
#24691=CARTESIAN_POINT('Ctrl Pts',(-41.7562341395977,-11.7410945211992,
0.));
#24692=CARTESIAN_POINT('Ctrl Pts',(-41.7562341395977,-11.7410945211992,
18.));
#24693=CARTESIAN_POINT('Ctrl Pts',(-41.8282796562569,-11.81512813804,0.));
#24694=CARTESIAN_POINT('Ctrl Pts',(-41.8282796562569,-11.81512813804,18.));
#24695=CARTESIAN_POINT('Ctrl Pts',(-41.9000638152266,-11.8895948153349,
0.));
#24696=CARTESIAN_POINT('Ctrl Pts',(-41.9000638152266,-11.8895948153349,
18.));
#24697=CARTESIAN_POINT('Ctrl Pts',(-41.9715865222182,-11.9644914999263,
0.));
#24698=CARTESIAN_POINT('Ctrl Pts',(-41.9715865222182,-11.9644914999263,
18.));
#24699=CARTESIAN_POINT('Ctrl Pts',(-42.0428479428228,-12.0398158079102,
0.));
#24700=CARTESIAN_POINT('Ctrl Pts',(-42.0428479428228,-12.0398158079102,
18.));
#24701=CARTESIAN_POINT('Ctrl Pts',(-42.1138483839101,-12.1155659644537,
0.));
#24702=CARTESIAN_POINT('Ctrl Pts',(-42.1138483839101,-12.1155659644537,
18.));
#24703=CARTESIAN_POINT('Ctrl Pts',(-42.1704402333854,-12.1765058047069,
0.));
#24704=CARTESIAN_POINT('Ctrl Pts',(-42.1704402333854,-12.1765058047069,
18.));
#24705=CARTESIAN_POINT('Ctrl Pts',(-42.2127669677092,-12.2224014666679,
0.));
#24706=CARTESIAN_POINT('Ctrl Pts',(-42.2127669677092,-12.2224014666679,
18.));
#24707=CARTESIAN_POINT('Ctrl Pts',(-42.2409327400055,-12.2530833383985,
0.));
#24708=CARTESIAN_POINT('Ctrl Pts',(-42.2409327400055,-12.2530833383985,
18.));
#24709=CARTESIAN_POINT('Ctrl Pts',(-42.2550026135057,-12.2684454652018,
0.));
#24710=CARTESIAN_POINT('Ctrl Pts',(-42.2550026135057,-12.2684454652018,
18.));
#24711=CARTESIAN_POINT('Ctrl Pts',(-36.6758703925241,-8.2289783962506,0.));
#24712=CARTESIAN_POINT('Ctrl Pts',(-36.6943771018148,-8.23313075335376,
0.));
#24713=CARTESIAN_POINT('Ctrl Pts',(-36.7312504697652,-8.24192165947367,
0.));
#24714=CARTESIAN_POINT('Ctrl Pts',(-36.7861403757604,-8.2565665745182,0.));
#24715=CARTESIAN_POINT('Ctrl Pts',(-36.8585291300917,-8.27886599440784,
0.));
#24716=CARTESIAN_POINT('Ctrl Pts',(-36.9479311729484,-8.31052547794591,
0.));
#24717=CARTESIAN_POINT('Ctrl Pts',(-37.0365602155148,-8.34490818952639,
0.));
#24718=CARTESIAN_POINT('Ctrl Pts',(-37.1247207489179,-8.38096706211447,
0.));
#24719=CARTESIAN_POINT('Ctrl Pts',(-37.2126332013933,-8.41793088313259,
0.));
#24720=CARTESIAN_POINT('Ctrl Pts',(-37.3003733151561,-8.45550849433959,
0.));
#24721=CARTESIAN_POINT('Ctrl Pts',(-37.3879218093514,-8.49372546467075,
0.));
#24722=CARTESIAN_POINT('Ctrl Pts',(-37.4752030152968,-8.53279758643783,
0.));
#24723=CARTESIAN_POINT('Ctrl Pts',(-37.5621256752108,-8.57299698459465,
0.));
#24724=CARTESIAN_POINT('Ctrl Pts',(-37.6486274754754,-8.61450621749154,
0.));
#24725=CARTESIAN_POINT('Ctrl Pts',(-37.7347032383719,-8.65732553894524,
0.));
#24726=CARTESIAN_POINT('Ctrl Pts',(-37.8203816669031,-8.70134776631143,
0.));
#24727=CARTESIAN_POINT('Ctrl Pts',(-37.9057107230066,-8.74640499479002,
0.));
#24728=CARTESIAN_POINT('Ctrl Pts',(-37.9907407304174,-8.79232279131091,
0.));
#24729=CARTESIAN_POINT('Ctrl Pts',(-38.0755058326913,-8.83897959763348,
0.));
#24730=CARTESIAN_POINT('Ctrl Pts',(-38.1600150482528,-8.88633535238434,
0.));
#24731=CARTESIAN_POINT('Ctrl Pts',(-38.2442625706309,-8.93439830996338,
0.));
#24732=CARTESIAN_POINT('Ctrl Pts',(-38.3282340281403,-8.98320483785759,
0.));
#24733=CARTESIAN_POINT('Ctrl Pts',(-38.4119138099805,-9.0327957936019,0.));
#24734=CARTESIAN_POINT('Ctrl Pts',(-38.4952932486131,-9.08319014288085,
0.));
#24735=CARTESIAN_POINT('Ctrl Pts',(-38.5783736628826,-9.13437512010585,
0.));
#24736=CARTESIAN_POINT('Ctrl Pts',(-38.6611620045193,-9.18632019394329,
0.));
#24737=CARTESIAN_POINT('Ctrl Pts',(-38.7436682576832,-9.23898539199331,
0.));
#24738=CARTESIAN_POINT('Ctrl Pts',(-38.8259023794241,-9.29233110570902,
0.));
#24739=CARTESIAN_POINT('Ctrl Pts',(-38.9078708427078,-9.34632917154636,
0.));
#24740=CARTESIAN_POINT('Ctrl Pts',(-38.9895756526779,-9.40096600877643,
0.));
#24741=CARTESIAN_POINT('Ctrl Pts',(-39.0710161994951,-9.45623664577431,
0.));
#24742=CARTESIAN_POINT('Ctrl Pts',(-39.1521903958955,-9.5121410453562,0.));
#24743=CARTESIAN_POINT('Ctrl Pts',(-39.2330959982788,-9.56867984233622,
0.));
#24744=CARTESIAN_POINT('Ctrl Pts',(-39.3137321153686,-9.62584947846543,
0.));
#24745=CARTESIAN_POINT('Ctrl Pts',(-39.3940995760289,-9.68364100883826,
0.));
#24746=CARTESIAN_POINT('Ctrl Pts',(-39.4742001555227,-9.74204258152662,
0.));
#24747=CARTESIAN_POINT('Ctrl Pts',(-39.5540361022309,-9.80104095251613,
0.));
#24748=CARTESIAN_POINT('Ctrl Pts',(-39.6336095893767,-9.86062324242559,
0.));
#24749=CARTESIAN_POINT('Ctrl Pts',(-39.712922089547,-9.92077894513191,0.));
#24750=CARTESIAN_POINT('Ctrl Pts',(-39.7919742367922,-9.98150036150822,
0.));
#24751=CARTESIAN_POINT('Ctrl Pts',(-39.8707661565233,-10.0427815229883,
0.));
#24752=CARTESIAN_POINT('Ctrl Pts',(-39.9492976736738,-10.1046175096878,
0.));
#24753=CARTESIAN_POINT('Ctrl Pts',(-40.0275685525923,-10.1670036683795,
0.));
#24754=CARTESIAN_POINT('Ctrl Pts',(-40.1055787732578,-10.2299347125857,
0.));
#24755=CARTESIAN_POINT('Ctrl Pts',(-40.1833286010098,-10.2934044990237,
0.));
#24756=CARTESIAN_POINT('Ctrl Pts',(-40.2608184485326,-10.3574064830678,
0.));
#24757=CARTESIAN_POINT('Ctrl Pts',(-40.3380487942952,-10.421933993295,0.));
#24758=CARTESIAN_POINT('Ctrl Pts',(-40.4150200869536,-10.48698054978,0.));
#24759=CARTESIAN_POINT('Ctrl Pts',(-40.4917326404439,-10.5525402237951,
0.));
#24760=CARTESIAN_POINT('Ctrl Pts',(-40.5681866012103,-10.618607730849,0.));
#24761=CARTESIAN_POINT('Ctrl Pts',(-40.6443819999244,-10.6851782157325,
0.));
#24762=CARTESIAN_POINT('Ctrl Pts',(-40.7203187831783,-10.7522471109694,
0.));
#24763=CARTESIAN_POINT('Ctrl Pts',(-40.7959968527561,-10.8198099757795,
0.));
#24764=CARTESIAN_POINT('Ctrl Pts',(-40.8714161092412,-10.8878623066646,
0.));
#24765=CARTESIAN_POINT('Ctrl Pts',(-40.9465764747798,-10.956399476781,0.));
#24766=CARTESIAN_POINT('Ctrl Pts',(-41.0214778832142,-11.0254168609972,
0.));
#24767=CARTESIAN_POINT('Ctrl Pts',(-41.0961202807715,-11.0949099155251,
0.));
#24768=CARTESIAN_POINT('Ctrl Pts',(-41.1705036228854,-11.1648742640378,
0.));
#24769=CARTESIAN_POINT('Ctrl Pts',(-41.2446278781981,-11.2353057980338,
0.));
#24770=CARTESIAN_POINT('Ctrl Pts',(-41.3184930194148,-11.3062006993745,
0.));
#24771=CARTESIAN_POINT('Ctrl Pts',(-41.3920989905986,-11.3775553120176,
0.));
#24772=CARTESIAN_POINT('Ctrl Pts',(-41.4654456796071,-11.4493660393849,
0.));
#24773=CARTESIAN_POINT('Ctrl Pts',(-41.5385328935506,-11.5216292382388,
0.));
#24774=CARTESIAN_POINT('Ctrl Pts',(-41.6113603270596,-11.5943410868252,
0.));
#24775=CARTESIAN_POINT('Ctrl Pts',(-41.6839275596248,-11.6674975352851,
0.));
#24776=CARTESIAN_POINT('Ctrl Pts',(-41.7562341395977,-11.7410945211992,
0.));
#24777=CARTESIAN_POINT('Ctrl Pts',(-41.8282796562569,-11.81512813804,0.));
#24778=CARTESIAN_POINT('Ctrl Pts',(-41.9000638152266,-11.8895948153349,
0.));
#24779=CARTESIAN_POINT('Ctrl Pts',(-41.9715865222182,-11.9644914999263,
0.));
#24780=CARTESIAN_POINT('Ctrl Pts',(-42.0571002269437,-12.054880669507,0.));
#24781=CARTESIAN_POINT('Ctrl Pts',(-42.1280354231517,-12.1307372881904,
0.));
#24782=CARTESIAN_POINT('Ctrl Pts',(-42.18457517013,-12.1917619768791,0.));
#24783=CARTESIAN_POINT('Ctrl Pts',(-42.2268628664988,-12.2377212115623,
0.));
#24784=CARTESIAN_POINT('Ctrl Pts',(-42.2550026135057,-12.2684454652018,
0.));
#24785=CARTESIAN_POINT('Ctrl Pts',(-36.6758703925241,-8.2289783962506,15.));
#24786=CARTESIAN_POINT('Ctrl Pts',(-36.6943771018148,-8.23313075335376,
15.));
#24787=CARTESIAN_POINT('Ctrl Pts',(-36.7312504697652,-8.24192165947367,
15.));
#24788=CARTESIAN_POINT('Ctrl Pts',(-36.7861403757604,-8.2565665745182,15.));
#24789=CARTESIAN_POINT('Ctrl Pts',(-36.8585291300917,-8.27886599440784,
15.));
#24790=CARTESIAN_POINT('Ctrl Pts',(-36.9479311729484,-8.31052547794591,
15.));
#24791=CARTESIAN_POINT('Ctrl Pts',(-37.0365602155148,-8.34490818952639,
15.));
#24792=CARTESIAN_POINT('Ctrl Pts',(-37.1247207489179,-8.38096706211447,
15.));
#24793=CARTESIAN_POINT('Ctrl Pts',(-37.2126332013933,-8.41793088313259,
15.));
#24794=CARTESIAN_POINT('Ctrl Pts',(-37.3003733151561,-8.45550849433959,
15.));
#24795=CARTESIAN_POINT('Ctrl Pts',(-37.3879218093514,-8.49372546467075,
15.));
#24796=CARTESIAN_POINT('Ctrl Pts',(-37.4752030152968,-8.53279758643783,
15.));
#24797=CARTESIAN_POINT('Ctrl Pts',(-37.5621256752108,-8.57299698459465,
15.));
#24798=CARTESIAN_POINT('Ctrl Pts',(-37.6486274754754,-8.61450621749154,
15.));
#24799=CARTESIAN_POINT('Ctrl Pts',(-37.7347032383719,-8.65732553894524,
15.));
#24800=CARTESIAN_POINT('Ctrl Pts',(-37.8203816669031,-8.70134776631143,
15.));
#24801=CARTESIAN_POINT('Ctrl Pts',(-37.9057107230066,-8.74640499479002,
15.));
#24802=CARTESIAN_POINT('Ctrl Pts',(-37.9907407304174,-8.79232279131091,
15.));
#24803=CARTESIAN_POINT('Ctrl Pts',(-38.0755058326913,-8.83897959763348,
15.));
#24804=CARTESIAN_POINT('Ctrl Pts',(-38.1600150482528,-8.88633535238434,
15.));
#24805=CARTESIAN_POINT('Ctrl Pts',(-38.2442625706309,-8.93439830996338,
15.));
#24806=CARTESIAN_POINT('Ctrl Pts',(-38.3282340281403,-8.98320483785759,
15.));
#24807=CARTESIAN_POINT('Ctrl Pts',(-38.4119138099805,-9.0327957936019,15.));
#24808=CARTESIAN_POINT('Ctrl Pts',(-38.4952932486131,-9.08319014288085,
15.));
#24809=CARTESIAN_POINT('Ctrl Pts',(-38.5783736628826,-9.13437512010585,
15.));
#24810=CARTESIAN_POINT('Ctrl Pts',(-38.6611620045193,-9.18632019394329,
15.));
#24811=CARTESIAN_POINT('Ctrl Pts',(-38.7436682576832,-9.23898539199331,
15.));
#24812=CARTESIAN_POINT('Ctrl Pts',(-38.8259023794241,-9.29233110570902,
15.));
#24813=CARTESIAN_POINT('Ctrl Pts',(-38.9078708427078,-9.34632917154636,
15.));
#24814=CARTESIAN_POINT('Ctrl Pts',(-38.9895756526779,-9.40096600877643,
15.));
#24815=CARTESIAN_POINT('Ctrl Pts',(-39.0710161994951,-9.45623664577431,
15.));
#24816=CARTESIAN_POINT('Ctrl Pts',(-39.1521903958955,-9.5121410453562,15.));
#24817=CARTESIAN_POINT('Ctrl Pts',(-39.2330959982788,-9.56867984233622,
15.));
#24818=CARTESIAN_POINT('Ctrl Pts',(-39.3137321153686,-9.62584947846543,
15.));
#24819=CARTESIAN_POINT('Ctrl Pts',(-39.3940995760289,-9.68364100883826,
15.));
#24820=CARTESIAN_POINT('Ctrl Pts',(-39.4742001555227,-9.74204258152662,
15.));
#24821=CARTESIAN_POINT('Ctrl Pts',(-39.5540361022309,-9.80104095251613,
15.));
#24822=CARTESIAN_POINT('Ctrl Pts',(-39.6336095893767,-9.86062324242559,
15.));
#24823=CARTESIAN_POINT('Ctrl Pts',(-39.712922089547,-9.92077894513191,15.));
#24824=CARTESIAN_POINT('Ctrl Pts',(-39.7919742367922,-9.98150036150822,
15.));
#24825=CARTESIAN_POINT('Ctrl Pts',(-39.8707661565233,-10.0427815229883,
15.));
#24826=CARTESIAN_POINT('Ctrl Pts',(-39.9492976736738,-10.1046175096878,
15.));
#24827=CARTESIAN_POINT('Ctrl Pts',(-40.0275685525923,-10.1670036683795,
15.));
#24828=CARTESIAN_POINT('Ctrl Pts',(-40.1055787732578,-10.2299347125857,
15.));
#24829=CARTESIAN_POINT('Ctrl Pts',(-40.1833286010098,-10.2934044990237,
15.));
#24830=CARTESIAN_POINT('Ctrl Pts',(-40.2608184485326,-10.3574064830678,
15.));
#24831=CARTESIAN_POINT('Ctrl Pts',(-40.3380487942952,-10.421933993295,15.));
#24832=CARTESIAN_POINT('Ctrl Pts',(-40.4150200869536,-10.48698054978,15.));
#24833=CARTESIAN_POINT('Ctrl Pts',(-40.4917326404439,-10.5525402237951,
15.));
#24834=CARTESIAN_POINT('Ctrl Pts',(-40.5681866012103,-10.618607730849,15.));
#24835=CARTESIAN_POINT('Ctrl Pts',(-40.6443819999244,-10.6851782157325,
15.));
#24836=CARTESIAN_POINT('Ctrl Pts',(-40.7203187831783,-10.7522471109694,
15.));
#24837=CARTESIAN_POINT('Ctrl Pts',(-40.7959968527561,-10.8198099757795,
15.));
#24838=CARTESIAN_POINT('Ctrl Pts',(-40.8714161092412,-10.8878623066646,
15.));
#24839=CARTESIAN_POINT('Ctrl Pts',(-40.9465764747798,-10.956399476781,15.));
#24840=CARTESIAN_POINT('Ctrl Pts',(-41.0214778832142,-11.0254168609972,
15.));
#24841=CARTESIAN_POINT('Ctrl Pts',(-41.0961202807715,-11.0949099155251,
15.));
#24842=CARTESIAN_POINT('Ctrl Pts',(-41.1705036228854,-11.1648742640378,
15.));
#24843=CARTESIAN_POINT('Ctrl Pts',(-41.2446278781981,-11.2353057980338,
15.));
#24844=CARTESIAN_POINT('Ctrl Pts',(-41.3184930194148,-11.3062006993745,
15.));
#24845=CARTESIAN_POINT('Ctrl Pts',(-41.3920989905986,-11.3775553120176,
15.));
#24846=CARTESIAN_POINT('Ctrl Pts',(-41.4654456796071,-11.4493660393849,
15.));
#24847=CARTESIAN_POINT('Ctrl Pts',(-41.5385328935506,-11.5216292382388,
15.));
#24848=CARTESIAN_POINT('Ctrl Pts',(-41.6113603270596,-11.5943410868252,
15.));
#24849=CARTESIAN_POINT('Ctrl Pts',(-41.6839275596248,-11.6674975352851,
15.));
#24850=CARTESIAN_POINT('Ctrl Pts',(-41.7562341395977,-11.7410945211992,
15.));
#24851=CARTESIAN_POINT('Ctrl Pts',(-41.8282796562569,-11.81512813804,15.));
#24852=CARTESIAN_POINT('Ctrl Pts',(-41.9000638152266,-11.8895948153349,
15.));
#24853=CARTESIAN_POINT('Ctrl Pts',(-41.9715865222182,-11.9644914999263,
15.));
#24854=CARTESIAN_POINT('Ctrl Pts',(-42.0571002269437,-12.054880669507,15.));
#24855=CARTESIAN_POINT('Ctrl Pts',(-42.1280354231517,-12.1307372881904,
15.));
#24856=CARTESIAN_POINT('Ctrl Pts',(-42.18457517013,-12.1917619768791,15.));
#24857=CARTESIAN_POINT('Ctrl Pts',(-42.2268628664988,-12.2377212115623,
15.));
#24858=CARTESIAN_POINT('Ctrl Pts',(-42.2550026135057,-12.2684454652018,
15.));
#24859=CARTESIAN_POINT('Ctrl Pts',(-43.9780537249529,-1.38952890043916,
0.));
#24860=CARTESIAN_POINT('Ctrl Pts',(-43.9780537249529,-1.38952890043916,
18.));
#24861=CARTESIAN_POINT('Ctrl Pts',(-43.9599253218252,-1.39979132121931,
0.));
#24862=CARTESIAN_POINT('Ctrl Pts',(-43.9599253218252,-1.39979132121931,
18.));
#24863=CARTESIAN_POINT('Ctrl Pts',(-43.9236568607623,-1.42026781296156,
0.));
#24864=CARTESIAN_POINT('Ctrl Pts',(-43.9236568607623,-1.42026781296156,
18.));
#24865=CARTESIAN_POINT('Ctrl Pts',(-43.8692192047561,-1.45083750111682,
0.));
#24866=CARTESIAN_POINT('Ctrl Pts',(-43.8692192047561,-1.45083750111682,
18.));
#24867=CARTESIAN_POINT('Ctrl Pts',(-43.7965657112708,-1.49130689006066,
0.));
#24868=CARTESIAN_POINT('Ctrl Pts',(-43.7965657112708,-1.49130689006066,
18.));
#24869=CARTESIAN_POINT('Ctrl Pts',(-43.7056321934163,-1.54140922714764,
0.));
#24870=CARTESIAN_POINT('Ctrl Pts',(-43.7056321934163,-1.54140922714764,
18.));
#24871=CARTESIAN_POINT('Ctrl Pts',(-43.6145820637333,-1.59102591108103,
0.));
#24872=CARTESIAN_POINT('Ctrl Pts',(-43.6145820637333,-1.59102591108103,
18.));
#24873=CARTESIAN_POINT('Ctrl Pts',(-43.5234155788248,-1.64015515906648,
0.));
#24874=CARTESIAN_POINT('Ctrl Pts',(-43.5234155788248,-1.64015515906648,
18.));
#24875=CARTESIAN_POINT('Ctrl Pts',(-43.4321333178711,-1.68879465270608,
0.));
#24876=CARTESIAN_POINT('Ctrl Pts',(-43.4321333178711,-1.68879465270608,
18.));
#24877=CARTESIAN_POINT('Ctrl Pts',(-43.3407363140236,-1.73694151741123,
0.));
#24878=CARTESIAN_POINT('Ctrl Pts',(-43.3407363140236,-1.73694151741123,
18.));
#24879=CARTESIAN_POINT('Ctrl Pts',(-43.2492259505872,-1.78459244842769,
0.));
#24880=CARTESIAN_POINT('Ctrl Pts',(-43.2492259505872,-1.78459244842769,
18.));
#24881=CARTESIAN_POINT('Ctrl Pts',(-43.1576038253643,-1.83174385734711,
0.));
#24882=CARTESIAN_POINT('Ctrl Pts',(-43.1576038253643,-1.83174385734711,
18.));
#24883=CARTESIAN_POINT('Ctrl Pts',(-43.065871623255,-1.87839202014609,0.));
#24884=CARTESIAN_POINT('Ctrl Pts',(-43.065871623255,-1.87839202014609,18.));
#24885=CARTESIAN_POINT('Ctrl Pts',(-42.9740309956624,-1.92453321512435,
0.));
#24886=CARTESIAN_POINT('Ctrl Pts',(-42.9740309956624,-1.92453321512435,
18.));
#24887=CARTESIAN_POINT('Ctrl Pts',(-42.8820834139973,-1.97016390194216,
0.));
#24888=CARTESIAN_POINT('Ctrl Pts',(-42.8820834139973,-1.97016390194216,
18.));
#24889=CARTESIAN_POINT('Ctrl Pts',(-42.7900301875309,-2.01528067528089,
0.));
#24890=CARTESIAN_POINT('Ctrl Pts',(-42.7900301875309,-2.01528067528089,
18.));
#24891=CARTESIAN_POINT('Ctrl Pts',(-42.6978725343209,-2.05988014924519,
0.));
#24892=CARTESIAN_POINT('Ctrl Pts',(-42.6978725343209,-2.05988014924519,
18.));
#24893=CARTESIAN_POINT('Ctrl Pts',(-42.6056116373456,-2.1039588640177,0.));
#24894=CARTESIAN_POINT('Ctrl Pts',(-42.6056116373456,-2.1039588640177,18.));
#24895=CARTESIAN_POINT('Ctrl Pts',(-42.5132487024335,-2.14751319676745,
0.));
#24896=CARTESIAN_POINT('Ctrl Pts',(-42.5132487024335,-2.14751319676745,
18.));
#24897=CARTESIAN_POINT('Ctrl Pts',(-42.4207850290047,-2.19053924976737,
0.));
#24898=CARTESIAN_POINT('Ctrl Pts',(-42.4207850290047,-2.19053924976737,
18.));
#24899=CARTESIAN_POINT('Ctrl Pts',(-42.3282220118033,-2.23303287465499,
0.));
#24900=CARTESIAN_POINT('Ctrl Pts',(-42.3282220118033,-2.23303287465499,
18.));
#24901=CARTESIAN_POINT('Ctrl Pts',(-42.2355611060784,-2.27498976664774,
0.));
#24902=CARTESIAN_POINT('Ctrl Pts',(-42.2355611060784,-2.27498976664774,
18.));
#24903=CARTESIAN_POINT('Ctrl Pts',(-42.1428038039937,-2.31640554742808,
0.));
#24904=CARTESIAN_POINT('Ctrl Pts',(-42.1428038039937,-2.31640554742808,
18.));
#24905=CARTESIAN_POINT('Ctrl Pts',(-42.0499516093661,-2.35727584066429,
0.));
#24906=CARTESIAN_POINT('Ctrl Pts',(-42.0499516093661,-2.35727584066429,
18.));
#24907=CARTESIAN_POINT('Ctrl Pts',(-41.9570060084039,-2.39759639399648,
0.));
#24908=CARTESIAN_POINT('Ctrl Pts',(-41.9570060084039,-2.39759639399648,
18.));
#24909=CARTESIAN_POINT('Ctrl Pts',(-41.8639684667923,-2.437363014342,0.));
#24910=CARTESIAN_POINT('Ctrl Pts',(-41.8639684667923,-2.437363014342,18.));
#24911=CARTESIAN_POINT('Ctrl Pts',(-41.7708404467533,-2.47657137427693,
0.));
#24912=CARTESIAN_POINT('Ctrl Pts',(-41.7708404467533,-2.47657137427693,
18.));
#24913=CARTESIAN_POINT('Ctrl Pts',(-41.6776234194583,-2.51521684674477,
0.));
#24914=CARTESIAN_POINT('Ctrl Pts',(-41.6776234194583,-2.51521684674477,
18.));
#24915=CARTESIAN_POINT('Ctrl Pts',(-41.5843188786284,-2.55329436064184,
0.));
#24916=CARTESIAN_POINT('Ctrl Pts',(-41.5843188786284,-2.55329436064184,
18.));
#24917=CARTESIAN_POINT('Ctrl Pts',(-41.4909283577703,-2.59079818040171,
0.));
#24918=CARTESIAN_POINT('Ctrl Pts',(-41.4909283577703,-2.59079818040171,
18.));
#24919=CARTESIAN_POINT('Ctrl Pts',(-41.3974534325937,-2.62772200460656,
0.));
#24920=CARTESIAN_POINT('Ctrl Pts',(-41.3974534325937,-2.62772200460656,
18.));
#24921=CARTESIAN_POINT('Ctrl Pts',(-41.3038957096306,-2.66405934050118,
0.));
#24922=CARTESIAN_POINT('Ctrl Pts',(-41.3038957096306,-2.66405934050118,
18.));
#24923=CARTESIAN_POINT('Ctrl Pts',(-41.2102568187956,-2.69980383625015,
0.));
#24924=CARTESIAN_POINT('Ctrl Pts',(-41.2102568187956,-2.69980383625015,
18.));
#24925=CARTESIAN_POINT('Ctrl Pts',(-41.1165384061145,-2.73494956725005,
0.));
#24926=CARTESIAN_POINT('Ctrl Pts',(-41.1165384061145,-2.73494956725005,
18.));
#24927=CARTESIAN_POINT('Ctrl Pts',(-41.0227421242398,-2.76949151194863,
0.));
#24928=CARTESIAN_POINT('Ctrl Pts',(-41.0227421242398,-2.76949151194863,
18.));
#24929=CARTESIAN_POINT('Ctrl Pts',(-40.9288696352159,-2.80342531768405,
0.));
#24930=CARTESIAN_POINT('Ctrl Pts',(-40.9288696352159,-2.80342531768405,
18.));
#24931=CARTESIAN_POINT('Ctrl Pts',(-40.8349226258683,-2.83674635946679,
0.));
#24932=CARTESIAN_POINT('Ctrl Pts',(-40.8349226258683,-2.83674635946679,
18.));
#24933=CARTESIAN_POINT('Ctrl Pts',(-40.7409028213129,-2.86944892209897,
0.));
#24934=CARTESIAN_POINT('Ctrl Pts',(-40.7409028213129,-2.86944892209897,
18.));
#24935=CARTESIAN_POINT('Ctrl Pts',(-40.6468119976928,-2.90152548734342,
0.));
#24936=CARTESIAN_POINT('Ctrl Pts',(-40.6468119976928,-2.90152548734342,
18.));
#24937=CARTESIAN_POINT('Ctrl Pts',(-40.5526520010651,-2.93296560822893,
0.));
#24938=CARTESIAN_POINT('Ctrl Pts',(-40.5526520010651,-2.93296560822893,
18.));
#24939=CARTESIAN_POINT('Ctrl Pts',(-40.4584247445196,-2.96375636417322,
0.));
#24940=CARTESIAN_POINT('Ctrl Pts',(-40.4584247445196,-2.96375636417322,
18.));
#24941=CARTESIAN_POINT('Ctrl Pts',(-40.3641321823444,-2.99388446458219,
0.));
#24942=CARTESIAN_POINT('Ctrl Pts',(-40.3641321823444,-2.99388446458219,
18.));
#24943=CARTESIAN_POINT('Ctrl Pts',(-40.2697762886113,-3.02333808901595,
0.));
#24944=CARTESIAN_POINT('Ctrl Pts',(-40.2697762886113,-3.02333808901595,
18.));
#24945=CARTESIAN_POINT('Ctrl Pts',(-40.1753590391515,-3.0521084742307,0.));
#24946=CARTESIAN_POINT('Ctrl Pts',(-40.1753590391515,-3.0521084742307,18.));
#24947=CARTESIAN_POINT('Ctrl Pts',(-40.0808823811787,-3.08019251155015,
0.));
#24948=CARTESIAN_POINT('Ctrl Pts',(-40.0808823811787,-3.08019251155015,
18.));
#24949=CARTESIAN_POINT('Ctrl Pts',(-39.9863482523153,-3.10759149802907,
0.));
#24950=CARTESIAN_POINT('Ctrl Pts',(-39.9863482523153,-3.10759149802907,
18.));
#24951=CARTESIAN_POINT('Ctrl Pts',(-39.8917586491576,-3.13430604330355,
0.));
#24952=CARTESIAN_POINT('Ctrl Pts',(-39.8917586491576,-3.13430604330355,
18.));
#24953=CARTESIAN_POINT('Ctrl Pts',(-39.7971156880138,-3.16033160752803,
0.));
#24954=CARTESIAN_POINT('Ctrl Pts',(-39.7971156880138,-3.16033160752803,
18.));
#24955=CARTESIAN_POINT('Ctrl Pts',(-39.7024216585552,-3.18565465503835,
0.));
#24956=CARTESIAN_POINT('Ctrl Pts',(-39.7024216585552,-3.18565465503835,
18.));
#24957=CARTESIAN_POINT('Ctrl Pts',(-39.607679107639,-3.21024640045595,0.));
#24958=CARTESIAN_POINT('Ctrl Pts',(-39.607679107639,-3.21024640045595,18.));
#24959=CARTESIAN_POINT('Ctrl Pts',(-39.5128908052622,-3.23406609691661,
0.));
#24960=CARTESIAN_POINT('Ctrl Pts',(-39.5128908052622,-3.23406609691661,
18.));
#24961=CARTESIAN_POINT('Ctrl Pts',(-39.4180596080755,-3.25707264313388,
0.));
#24962=CARTESIAN_POINT('Ctrl Pts',(-39.4180596080755,-3.25707264313388,
18.));
#24963=CARTESIAN_POINT('Ctrl Pts',(-39.3231883392913,-3.27923485388117,
0.));
#24964=CARTESIAN_POINT('Ctrl Pts',(-39.3231883392913,-3.27923485388117,
18.));
#24965=CARTESIAN_POINT('Ctrl Pts',(-39.2282796893977,-3.30054018081687,
0.));
#24966=CARTESIAN_POINT('Ctrl Pts',(-39.2282796893977,-3.30054018081687,
18.));
#24967=CARTESIAN_POINT('Ctrl Pts',(-39.1333360409949,-3.32100933979557,
0.));
#24968=CARTESIAN_POINT('Ctrl Pts',(-39.1333360409949,-3.32100933979557,
18.));
#24969=CARTESIAN_POINT('Ctrl Pts',(-39.0383596151636,-3.34068601264472,
0.));
#24970=CARTESIAN_POINT('Ctrl Pts',(-39.0383596151636,-3.34068601264472,
18.));
#24971=CARTESIAN_POINT('Ctrl Pts',(-38.9433528420174,-3.3596092279948,0.));
#24972=CARTESIAN_POINT('Ctrl Pts',(-38.9433528420174,-3.3596092279948,18.));
#24973=CARTESIAN_POINT('Ctrl Pts',(-38.8483186930884,-3.37778863054482,
0.));
#24974=CARTESIAN_POINT('Ctrl Pts',(-38.8483186930884,-3.37778863054482,
18.));
#24975=CARTESIAN_POINT('Ctrl Pts',(-38.7532609709905,-3.39518333281818,
0.));
#24976=CARTESIAN_POINT('Ctrl Pts',(-38.7532609709905,-3.39518333281818,
18.));
#24977=CARTESIAN_POINT('Ctrl Pts',(-38.6581847668347,-3.411667175119,0.));
#24978=CARTESIAN_POINT('Ctrl Pts',(-38.6581847668347,-3.411667175119,18.));
#24979=CARTESIAN_POINT('Ctrl Pts',(-38.5630961226878,-3.42705871084996,
0.));
#24980=CARTESIAN_POINT('Ctrl Pts',(-38.5630961226878,-3.42705871084996,
18.));
#24981=CARTESIAN_POINT('Ctrl Pts',(-38.4680013094732,-3.44118343200303,
0.));
#24982=CARTESIAN_POINT('Ctrl Pts',(-38.4680013094732,-3.44118343200303,
18.));
#24983=CARTESIAN_POINT('Ctrl Pts',(-38.3729061502716,-3.45393053211022,
0.));
#24984=CARTESIAN_POINT('Ctrl Pts',(-38.3729061502716,-3.45393053211022,
18.));
#24985=CARTESIAN_POINT('Ctrl Pts',(-38.2778154909527,-3.46530185256872,
0.));
#24986=CARTESIAN_POINT('Ctrl Pts',(-38.2778154909527,-3.46530185256872,
18.));
#24987=CARTESIAN_POINT('Ctrl Pts',(-38.1827321816559,-3.47549027265411,
0.));
#24988=CARTESIAN_POINT('Ctrl Pts',(-38.1827321816559,-3.47549027265411,
18.));
#24989=CARTESIAN_POINT('Ctrl Pts',(-38.0876589224537,-3.48478279878233,
0.));
#24990=CARTESIAN_POINT('Ctrl Pts',(-38.0876589224537,-3.48478279878233,
18.));
#24991=CARTESIAN_POINT('Ctrl Pts',(-37.9926009950482,-3.49340804454645,
0.));
#24992=CARTESIAN_POINT('Ctrl Pts',(-37.9926009950482,-3.49340804454645,
18.));
#24993=CARTESIAN_POINT('Ctrl Pts',(-37.8975688353863,-3.50139628556083,
0.));
#24994=CARTESIAN_POINT('Ctrl Pts',(-37.8975688353863,-3.50139628556083,
18.));
#24995=CARTESIAN_POINT('Ctrl Pts',(-37.8025803811856,-3.50844720825128,
0.));
#24996=CARTESIAN_POINT('Ctrl Pts',(-37.8025803811856,-3.50844720825128,
18.));
#24997=CARTESIAN_POINT('Ctrl Pts',(-37.7076643105286,-3.51375922979957,
0.));
#24998=CARTESIAN_POINT('Ctrl Pts',(-37.7076643105286,-3.51375922979957,
18.));
#24999=CARTESIAN_POINT('Ctrl Pts',(-37.6128545966533,-3.51624243734645,
0.));
#25000=CARTESIAN_POINT('Ctrl Pts',(-37.6128545966533,-3.51624243734645,
18.));
#25001=CARTESIAN_POINT('Ctrl Pts',(-37.5371179004295,-3.51508109065209,
0.));
#25002=CARTESIAN_POINT('Ctrl Pts',(-37.5371179004295,-3.51508109065209,
18.));
#25003=CARTESIAN_POINT('Ctrl Pts',(-37.4803889700239,-3.51204731876361,
0.));
#25004=CARTESIAN_POINT('Ctrl Pts',(-37.4803889700239,-3.51204731876361,
18.));
#25005=CARTESIAN_POINT('Ctrl Pts',(-37.4426037737699,-3.50901346997657,
0.));
#25006=CARTESIAN_POINT('Ctrl Pts',(-37.4426037737699,-3.50901346997657,
18.));
#25007=CARTESIAN_POINT('Ctrl Pts',(-37.4237196983922,-3.50724370857673,
0.));
#25008=CARTESIAN_POINT('Ctrl Pts',(-37.4237196983922,-3.50724370857673,
18.));
#25009=CARTESIAN_POINT('',(-43.9780537249529,-1.38952890043929,0.));
#25010=CARTESIAN_POINT('Ctrl Pts',(-37.4237196983922,-3.50724370857673,
0.));
#25011=CARTESIAN_POINT('Ctrl Pts',(-37.4426037737699,-3.50901346997657,
0.));
#25012=CARTESIAN_POINT('Ctrl Pts',(-37.4803889700239,-3.51204731876361,
0.));
#25013=CARTESIAN_POINT('Ctrl Pts',(-37.5371179004295,-3.51508109065209,
0.));
#25014=CARTESIAN_POINT('Ctrl Pts',(-37.6128545966533,-3.51624243734645,
0.));
#25015=CARTESIAN_POINT('Ctrl Pts',(-37.7076643105286,-3.51375922979957,
0.));
#25016=CARTESIAN_POINT('Ctrl Pts',(-37.8025803811856,-3.50844720825128,
0.));
#25017=CARTESIAN_POINT('Ctrl Pts',(-37.8975688353863,-3.50139628556083,
0.));
#25018=CARTESIAN_POINT('Ctrl Pts',(-37.9926009950482,-3.49340804454645,
0.));
#25019=CARTESIAN_POINT('Ctrl Pts',(-38.0876589224537,-3.48478279878233,
0.));
#25020=CARTESIAN_POINT('Ctrl Pts',(-38.1827321816559,-3.47549027265411,
0.));
#25021=CARTESIAN_POINT('Ctrl Pts',(-38.2778154909527,-3.46530185256872,
0.));
#25022=CARTESIAN_POINT('Ctrl Pts',(-38.3729061502716,-3.45393053211022,
0.));
#25023=CARTESIAN_POINT('Ctrl Pts',(-38.4680013094732,-3.44118343200303,
0.));
#25024=CARTESIAN_POINT('Ctrl Pts',(-38.5630961226878,-3.42705871084996,
0.));
#25025=CARTESIAN_POINT('Ctrl Pts',(-38.6581847668347,-3.411667175119,0.));
#25026=CARTESIAN_POINT('Ctrl Pts',(-38.7532609709905,-3.39518333281818,
0.));
#25027=CARTESIAN_POINT('Ctrl Pts',(-38.8483186930884,-3.37778863054482,
0.));
#25028=CARTESIAN_POINT('Ctrl Pts',(-38.9433528420174,-3.3596092279948,0.));
#25029=CARTESIAN_POINT('Ctrl Pts',(-39.0383596151636,-3.34068601264472,
0.));
#25030=CARTESIAN_POINT('Ctrl Pts',(-39.1333360409949,-3.32100933979557,
0.));
#25031=CARTESIAN_POINT('Ctrl Pts',(-39.2282796893977,-3.30054018081687,
0.));
#25032=CARTESIAN_POINT('Ctrl Pts',(-39.3231883392913,-3.27923485388117,
0.));
#25033=CARTESIAN_POINT('Ctrl Pts',(-39.4180596080755,-3.25707264313388,
0.));
#25034=CARTESIAN_POINT('Ctrl Pts',(-39.5128908052622,-3.23406609691661,
0.));
#25035=CARTESIAN_POINT('Ctrl Pts',(-39.607679107639,-3.21024640045595,0.));
#25036=CARTESIAN_POINT('Ctrl Pts',(-39.7024216585552,-3.18565465503835,
0.));
#25037=CARTESIAN_POINT('Ctrl Pts',(-39.7971156880138,-3.16033160752803,
0.));
#25038=CARTESIAN_POINT('Ctrl Pts',(-39.8917586491576,-3.13430604330355,
0.));
#25039=CARTESIAN_POINT('Ctrl Pts',(-39.9863482523153,-3.10759149802907,
0.));
#25040=CARTESIAN_POINT('Ctrl Pts',(-40.0808823811787,-3.08019251155015,
0.));
#25041=CARTESIAN_POINT('Ctrl Pts',(-40.1753590391515,-3.0521084742307,0.));
#25042=CARTESIAN_POINT('Ctrl Pts',(-40.2697762886113,-3.02333808901595,
0.));
#25043=CARTESIAN_POINT('Ctrl Pts',(-40.3641321823444,-2.99388446458219,
0.));
#25044=CARTESIAN_POINT('Ctrl Pts',(-40.4584247445196,-2.96375636417322,
0.));
#25045=CARTESIAN_POINT('Ctrl Pts',(-40.5526520010651,-2.93296560822893,
0.));
#25046=CARTESIAN_POINT('Ctrl Pts',(-40.6468119976928,-2.90152548734342,
0.));
#25047=CARTESIAN_POINT('Ctrl Pts',(-40.7409028213129,-2.86944892209897,
0.));
#25048=CARTESIAN_POINT('Ctrl Pts',(-40.8349226258683,-2.83674635946679,
0.));
#25049=CARTESIAN_POINT('Ctrl Pts',(-40.9288696352159,-2.80342531768405,
0.));
#25050=CARTESIAN_POINT('Ctrl Pts',(-41.0227421242398,-2.76949151194863,
0.));
#25051=CARTESIAN_POINT('Ctrl Pts',(-41.1165384061145,-2.73494956725005,
0.));
#25052=CARTESIAN_POINT('Ctrl Pts',(-41.2102568187956,-2.69980383625015,
0.));
#25053=CARTESIAN_POINT('Ctrl Pts',(-41.3038957096306,-2.66405934050118,
0.));
#25054=CARTESIAN_POINT('Ctrl Pts',(-41.3974534325937,-2.62772200460656,
0.));
#25055=CARTESIAN_POINT('Ctrl Pts',(-41.4909283577703,-2.59079818040171,
0.));
#25056=CARTESIAN_POINT('Ctrl Pts',(-41.5843188786284,-2.55329436064184,
0.));
#25057=CARTESIAN_POINT('Ctrl Pts',(-41.6776234194583,-2.51521684674477,
0.));
#25058=CARTESIAN_POINT('Ctrl Pts',(-41.7708404467533,-2.47657137427693,
0.));
#25059=CARTESIAN_POINT('Ctrl Pts',(-41.8639684667923,-2.437363014342,0.));
#25060=CARTESIAN_POINT('Ctrl Pts',(-41.9570060084039,-2.39759639399648,
0.));
#25061=CARTESIAN_POINT('Ctrl Pts',(-42.0499516093661,-2.35727584066429,
0.));
#25062=CARTESIAN_POINT('Ctrl Pts',(-42.1428038039937,-2.31640554742808,
0.));
#25063=CARTESIAN_POINT('Ctrl Pts',(-42.2355611060784,-2.27498976664774,
0.));
#25064=CARTESIAN_POINT('Ctrl Pts',(-42.3282220118033,-2.23303287465499,
0.));
#25065=CARTESIAN_POINT('Ctrl Pts',(-42.4207850290047,-2.19053924976737,
0.));
#25066=CARTESIAN_POINT('Ctrl Pts',(-42.5132487024335,-2.14751319676745,
0.));
#25067=CARTESIAN_POINT('Ctrl Pts',(-42.6056116373456,-2.1039588640177,0.));
#25068=CARTESIAN_POINT('Ctrl Pts',(-42.6978725343209,-2.05988014924519,
0.));
#25069=CARTESIAN_POINT('Ctrl Pts',(-42.7900301875309,-2.01528067528089,
0.));
#25070=CARTESIAN_POINT('Ctrl Pts',(-42.8820834139973,-1.97016390194216,
0.));
#25071=CARTESIAN_POINT('Ctrl Pts',(-42.9740309956624,-1.92453321512435,
0.));
#25072=CARTESIAN_POINT('Ctrl Pts',(-43.065871623255,-1.87839202014609,0.));
#25073=CARTESIAN_POINT('Ctrl Pts',(-43.1576038253643,-1.83174385734711,
0.));
#25074=CARTESIAN_POINT('Ctrl Pts',(-43.2492259505872,-1.78459244842769,
0.));
#25075=CARTESIAN_POINT('Ctrl Pts',(-43.3407363140236,-1.73694151741123,
0.));
#25076=CARTESIAN_POINT('Ctrl Pts',(-43.4321333178711,-1.68879465270608,
0.));
#25077=CARTESIAN_POINT('Ctrl Pts',(-43.5234155788248,-1.64015515906648,
0.));
#25078=CARTESIAN_POINT('Ctrl Pts',(-43.6145820637333,-1.59102591108103,
0.));
#25079=CARTESIAN_POINT('Ctrl Pts',(-43.7238422193529,-1.53148589036096,
0.));
#25080=CARTESIAN_POINT('Ctrl Pts',(-43.8147465842503,-1.48126213998558,
0.));
#25081=CARTESIAN_POINT('Ctrl Pts',(-43.8873767449247,-1.44069595482723,
0.));
#25082=CARTESIAN_POINT('Ctrl Pts',(-43.9417969186811,-1.41005374202872,
0.));
#25083=CARTESIAN_POINT('Ctrl Pts',(-43.9780537249529,-1.38952890043916,
0.));
#25084=CARTESIAN_POINT('',(-43.9780537249529,-1.38952890043929,15.));
#25085=CARTESIAN_POINT('Ctrl Pts',(-43.9780537249529,-1.38952890043916,
15.));
#25086=CARTESIAN_POINT('Ctrl Pts',(-43.9599253218252,-1.39979132121931,
15.));
#25087=CARTESIAN_POINT('Ctrl Pts',(-43.9236568607623,-1.42026781296156,
15.));
#25088=CARTESIAN_POINT('Ctrl Pts',(-43.8692192047561,-1.45083750111682,
15.));
#25089=CARTESIAN_POINT('Ctrl Pts',(-43.7965657112708,-1.49130689006066,
15.));
#25090=CARTESIAN_POINT('Ctrl Pts',(-43.7056321934163,-1.54140922714764,
15.));
#25091=CARTESIAN_POINT('Ctrl Pts',(-43.6145820637333,-1.59102591108103,
15.));
#25092=CARTESIAN_POINT('Ctrl Pts',(-43.5234155788248,-1.64015515906648,
15.));
#25093=CARTESIAN_POINT('Ctrl Pts',(-43.4321333178711,-1.68879465270608,
15.));
#25094=CARTESIAN_POINT('Ctrl Pts',(-43.3407363140236,-1.73694151741123,
15.));
#25095=CARTESIAN_POINT('Ctrl Pts',(-43.2492259505872,-1.78459244842769,
15.));
#25096=CARTESIAN_POINT('Ctrl Pts',(-43.1576038253643,-1.83174385734711,
15.));
#25097=CARTESIAN_POINT('Ctrl Pts',(-43.065871623255,-1.87839202014609,15.));
#25098=CARTESIAN_POINT('Ctrl Pts',(-42.9740309956624,-1.92453321512435,
15.));
#25099=CARTESIAN_POINT('Ctrl Pts',(-42.8820834139973,-1.97016390194216,
15.));
#25100=CARTESIAN_POINT('Ctrl Pts',(-42.7900301875309,-2.01528067528089,
15.));
#25101=CARTESIAN_POINT('Ctrl Pts',(-42.6978725343209,-2.05988014924519,
15.));
#25102=CARTESIAN_POINT('Ctrl Pts',(-42.6056116373456,-2.1039588640177,15.));
#25103=CARTESIAN_POINT('Ctrl Pts',(-42.5132487024335,-2.14751319676745,
15.));
#25104=CARTESIAN_POINT('Ctrl Pts',(-42.4207850290047,-2.19053924976737,
15.));
#25105=CARTESIAN_POINT('Ctrl Pts',(-42.3282220118033,-2.23303287465499,
15.));
#25106=CARTESIAN_POINT('Ctrl Pts',(-42.2355611060784,-2.27498976664774,
15.));
#25107=CARTESIAN_POINT('Ctrl Pts',(-42.1428038039937,-2.31640554742808,
15.));
#25108=CARTESIAN_POINT('Ctrl Pts',(-42.0499516093661,-2.35727584066429,
15.));
#25109=CARTESIAN_POINT('Ctrl Pts',(-41.9570060084039,-2.39759639399648,
15.));
#25110=CARTESIAN_POINT('Ctrl Pts',(-41.8639684667923,-2.437363014342,15.));
#25111=CARTESIAN_POINT('Ctrl Pts',(-41.7708404467533,-2.47657137427693,
15.));
#25112=CARTESIAN_POINT('Ctrl Pts',(-41.6776234194583,-2.51521684674477,
15.));
#25113=CARTESIAN_POINT('Ctrl Pts',(-41.5843188786284,-2.55329436064184,
15.));
#25114=CARTESIAN_POINT('Ctrl Pts',(-41.4909283577703,-2.59079818040171,
15.));
#25115=CARTESIAN_POINT('Ctrl Pts',(-41.3974534325937,-2.62772200460656,
15.));
#25116=CARTESIAN_POINT('Ctrl Pts',(-41.3038957096306,-2.66405934050118,
15.));
#25117=CARTESIAN_POINT('Ctrl Pts',(-41.2102568187956,-2.69980383625015,
15.));
#25118=CARTESIAN_POINT('Ctrl Pts',(-41.1165384061145,-2.73494956725005,
15.));
#25119=CARTESIAN_POINT('Ctrl Pts',(-41.0227421242398,-2.76949151194863,
15.));
#25120=CARTESIAN_POINT('Ctrl Pts',(-40.9288696352159,-2.80342531768405,
15.));
#25121=CARTESIAN_POINT('Ctrl Pts',(-40.8349226258683,-2.83674635946679,
15.));
#25122=CARTESIAN_POINT('Ctrl Pts',(-40.7409028213129,-2.86944892209897,
15.));
#25123=CARTESIAN_POINT('Ctrl Pts',(-40.6468119976928,-2.90152548734342,
15.));
#25124=CARTESIAN_POINT('Ctrl Pts',(-40.5526520010651,-2.93296560822893,
15.));
#25125=CARTESIAN_POINT('Ctrl Pts',(-40.4584247445196,-2.96375636417322,
15.));
#25126=CARTESIAN_POINT('Ctrl Pts',(-40.3641321823444,-2.99388446458219,
15.));
#25127=CARTESIAN_POINT('Ctrl Pts',(-40.2697762886113,-3.02333808901595,
15.));
#25128=CARTESIAN_POINT('Ctrl Pts',(-40.1753590391515,-3.0521084742307,15.));
#25129=CARTESIAN_POINT('Ctrl Pts',(-40.0808823811787,-3.08019251155015,
15.));
#25130=CARTESIAN_POINT('Ctrl Pts',(-39.9863482523153,-3.10759149802907,
15.));
#25131=CARTESIAN_POINT('Ctrl Pts',(-39.8917586491576,-3.13430604330355,
15.));
#25132=CARTESIAN_POINT('Ctrl Pts',(-39.7971156880138,-3.16033160752803,
15.));
#25133=CARTESIAN_POINT('Ctrl Pts',(-39.7024216585552,-3.18565465503835,
15.));
#25134=CARTESIAN_POINT('Ctrl Pts',(-39.607679107639,-3.21024640045595,15.));
#25135=CARTESIAN_POINT('Ctrl Pts',(-39.5128908052622,-3.23406609691661,
15.));
#25136=CARTESIAN_POINT('Ctrl Pts',(-39.4180596080755,-3.25707264313388,
15.));
#25137=CARTESIAN_POINT('Ctrl Pts',(-39.3231883392913,-3.27923485388117,
15.));
#25138=CARTESIAN_POINT('Ctrl Pts',(-39.2282796893977,-3.30054018081687,
15.));
#25139=CARTESIAN_POINT('Ctrl Pts',(-39.1333360409949,-3.32100933979557,
15.));
#25140=CARTESIAN_POINT('Ctrl Pts',(-39.0383596151636,-3.34068601264472,
15.));
#25141=CARTESIAN_POINT('Ctrl Pts',(-38.9433528420174,-3.3596092279948,15.));
#25142=CARTESIAN_POINT('Ctrl Pts',(-38.8483186930884,-3.37778863054482,
15.));
#25143=CARTESIAN_POINT('Ctrl Pts',(-38.7532609709905,-3.39518333281818,
15.));
#25144=CARTESIAN_POINT('Ctrl Pts',(-38.6581847668347,-3.411667175119,15.));
#25145=CARTESIAN_POINT('Ctrl Pts',(-38.5630961226878,-3.42705871084996,
15.));
#25146=CARTESIAN_POINT('Ctrl Pts',(-38.4680013094732,-3.44118343200303,
15.));
#25147=CARTESIAN_POINT('Ctrl Pts',(-38.3729061502716,-3.45393053211022,
15.));
#25148=CARTESIAN_POINT('Ctrl Pts',(-38.2778154909527,-3.46530185256872,
15.));
#25149=CARTESIAN_POINT('Ctrl Pts',(-38.1827321816559,-3.47549027265411,
15.));
#25150=CARTESIAN_POINT('Ctrl Pts',(-38.0876589224537,-3.48478279878233,
15.));
#25151=CARTESIAN_POINT('Ctrl Pts',(-37.9926009950482,-3.49340804454645,
15.));
#25152=CARTESIAN_POINT('Ctrl Pts',(-37.8975688353863,-3.50139628556083,
15.));
#25153=CARTESIAN_POINT('Ctrl Pts',(-37.8025803811856,-3.50844720825128,
15.));
#25154=CARTESIAN_POINT('Ctrl Pts',(-37.7076643105286,-3.51375922979957,
15.));
#25155=CARTESIAN_POINT('Ctrl Pts',(-37.6128545966533,-3.51624243734645,
15.));
#25156=CARTESIAN_POINT('Ctrl Pts',(-37.5371179004295,-3.51508109065209,
15.));
#25157=CARTESIAN_POINT('Ctrl Pts',(-37.4803889700239,-3.51204731876361,
15.));
#25158=CARTESIAN_POINT('Ctrl Pts',(-37.4426037737699,-3.50901346997657,
15.));
#25159=CARTESIAN_POINT('Ctrl Pts',(-37.4237196983922,-3.50724370857673,
15.));
#25160=CARTESIAN_POINT('',(-43.9780537249529,-1.38952890043929,0.));
#25161=CARTESIAN_POINT('Origin',(-1.13331566353736E-11,5.04870979341448E-28,
0.));
#25162=CARTESIAN_POINT('',(-43.9780537249529,1.38952890043917,0.));
#25163=CARTESIAN_POINT('Origin',(-1.13331566353736E-11,5.04870979341448E-28,
0.));
#25164=CARTESIAN_POINT('',(-43.9780537249529,1.38952890043917,15.));
#25165=CARTESIAN_POINT('Origin',(-1.13331566353736E-11,5.04870979341448E-28,
15.));
#25166=CARTESIAN_POINT('',(-43.9780537249529,1.38952890043917,0.));
#25167=CARTESIAN_POINT('Ctrl Pts',(-37.4237196983923,3.50724370857673,0.));
#25168=CARTESIAN_POINT('Ctrl Pts',(-37.4237196983923,3.50724370857673,18.));
#25169=CARTESIAN_POINT('Ctrl Pts',(-37.4426037737699,3.50901346997657,0.));
#25170=CARTESIAN_POINT('Ctrl Pts',(-37.4426037737699,3.50901346997657,18.));
#25171=CARTESIAN_POINT('Ctrl Pts',(-37.4803889700239,3.51204731876362,0.));
#25172=CARTESIAN_POINT('Ctrl Pts',(-37.4803889700239,3.51204731876362,18.));
#25173=CARTESIAN_POINT('Ctrl Pts',(-37.5371179004295,3.5150810906521,0.));
#25174=CARTESIAN_POINT('Ctrl Pts',(-37.5371179004295,3.5150810906521,18.));
#25175=CARTESIAN_POINT('Ctrl Pts',(-37.6128545966533,3.51624243734645,0.));
#25176=CARTESIAN_POINT('Ctrl Pts',(-37.6128545966533,3.51624243734645,18.));
#25177=CARTESIAN_POINT('Ctrl Pts',(-37.7076643105286,3.51375922979958,0.));
#25178=CARTESIAN_POINT('Ctrl Pts',(-37.7076643105286,3.51375922979958,18.));
#25179=CARTESIAN_POINT('Ctrl Pts',(-37.8025803811856,3.50844720825129,0.));
#25180=CARTESIAN_POINT('Ctrl Pts',(-37.8025803811856,3.50844720825129,18.));
#25181=CARTESIAN_POINT('Ctrl Pts',(-37.8975688353863,3.50139628556084,0.));
#25182=CARTESIAN_POINT('Ctrl Pts',(-37.8975688353863,3.50139628556084,18.));
#25183=CARTESIAN_POINT('Ctrl Pts',(-37.9926009950482,3.49340804454646,0.));
#25184=CARTESIAN_POINT('Ctrl Pts',(-37.9926009950482,3.49340804454646,18.));
#25185=CARTESIAN_POINT('Ctrl Pts',(-38.0876589224537,3.48478279878234,0.));
#25186=CARTESIAN_POINT('Ctrl Pts',(-38.0876589224537,3.48478279878234,18.));
#25187=CARTESIAN_POINT('Ctrl Pts',(-38.1827321816559,3.47549027265412,0.));
#25188=CARTESIAN_POINT('Ctrl Pts',(-38.1827321816559,3.47549027265412,18.));
#25189=CARTESIAN_POINT('Ctrl Pts',(-38.2778154909527,3.46530185256873,0.));
#25190=CARTESIAN_POINT('Ctrl Pts',(-38.2778154909527,3.46530185256873,18.));
#25191=CARTESIAN_POINT('Ctrl Pts',(-38.3729061502716,3.45393053211023,0.));
#25192=CARTESIAN_POINT('Ctrl Pts',(-38.3729061502716,3.45393053211023,18.));
#25193=CARTESIAN_POINT('Ctrl Pts',(-38.4680013094732,3.44118343200304,0.));
#25194=CARTESIAN_POINT('Ctrl Pts',(-38.4680013094732,3.44118343200304,18.));
#25195=CARTESIAN_POINT('Ctrl Pts',(-38.5630961226878,3.42705871084997,0.));
#25196=CARTESIAN_POINT('Ctrl Pts',(-38.5630961226878,3.42705871084997,18.));
#25197=CARTESIAN_POINT('Ctrl Pts',(-38.6581847668347,3.41166717511901,0.));
#25198=CARTESIAN_POINT('Ctrl Pts',(-38.6581847668347,3.41166717511901,18.));
#25199=CARTESIAN_POINT('Ctrl Pts',(-38.7532609709905,3.39518333281819,0.));
#25200=CARTESIAN_POINT('Ctrl Pts',(-38.7532609709905,3.39518333281819,18.));
#25201=CARTESIAN_POINT('Ctrl Pts',(-38.8483186930884,3.37778863054482,0.));
#25202=CARTESIAN_POINT('Ctrl Pts',(-38.8483186930884,3.37778863054482,18.));
#25203=CARTESIAN_POINT('Ctrl Pts',(-38.9433528420174,3.35960922799481,0.));
#25204=CARTESIAN_POINT('Ctrl Pts',(-38.9433528420174,3.35960922799481,18.));
#25205=CARTESIAN_POINT('Ctrl Pts',(-39.0383596151636,3.34068601264473,0.));
#25206=CARTESIAN_POINT('Ctrl Pts',(-39.0383596151636,3.34068601264473,18.));
#25207=CARTESIAN_POINT('Ctrl Pts',(-39.1333360409949,3.32100933979558,0.));
#25208=CARTESIAN_POINT('Ctrl Pts',(-39.1333360409949,3.32100933979558,18.));
#25209=CARTESIAN_POINT('Ctrl Pts',(-39.2282796893977,3.30054018081688,0.));
#25210=CARTESIAN_POINT('Ctrl Pts',(-39.2282796893977,3.30054018081688,18.));
#25211=CARTESIAN_POINT('Ctrl Pts',(-39.3231883392913,3.27923485388118,0.));
#25212=CARTESIAN_POINT('Ctrl Pts',(-39.3231883392913,3.27923485388118,18.));
#25213=CARTESIAN_POINT('Ctrl Pts',(-39.4180596080755,3.25707264313388,0.));
#25214=CARTESIAN_POINT('Ctrl Pts',(-39.4180596080755,3.25707264313388,18.));
#25215=CARTESIAN_POINT('Ctrl Pts',(-39.5128908052622,3.23406609691661,0.));
#25216=CARTESIAN_POINT('Ctrl Pts',(-39.5128908052622,3.23406609691661,18.));
#25217=CARTESIAN_POINT('Ctrl Pts',(-39.607679107639,3.21024640045596,0.));
#25218=CARTESIAN_POINT('Ctrl Pts',(-39.607679107639,3.21024640045596,18.));
#25219=CARTESIAN_POINT('Ctrl Pts',(-39.7024216585552,3.18565465503836,0.));
#25220=CARTESIAN_POINT('Ctrl Pts',(-39.7024216585552,3.18565465503836,18.));
#25221=CARTESIAN_POINT('Ctrl Pts',(-39.7971156880138,3.16033160752804,0.));
#25222=CARTESIAN_POINT('Ctrl Pts',(-39.7971156880138,3.16033160752804,18.));
#25223=CARTESIAN_POINT('Ctrl Pts',(-39.8917586491576,3.13430604330356,0.));
#25224=CARTESIAN_POINT('Ctrl Pts',(-39.8917586491576,3.13430604330356,18.));
#25225=CARTESIAN_POINT('Ctrl Pts',(-39.9863482523153,3.10759149802908,0.));
#25226=CARTESIAN_POINT('Ctrl Pts',(-39.9863482523153,3.10759149802908,18.));
#25227=CARTESIAN_POINT('Ctrl Pts',(-40.0808823811787,3.08019251155016,0.));
#25228=CARTESIAN_POINT('Ctrl Pts',(-40.0808823811787,3.08019251155016,18.));
#25229=CARTESIAN_POINT('Ctrl Pts',(-40.1753590391515,3.05210847423071,0.));
#25230=CARTESIAN_POINT('Ctrl Pts',(-40.1753590391515,3.05210847423071,18.));
#25231=CARTESIAN_POINT('Ctrl Pts',(-40.2697762886113,3.02333808901596,0.));
#25232=CARTESIAN_POINT('Ctrl Pts',(-40.2697762886113,3.02333808901596,18.));
#25233=CARTESIAN_POINT('Ctrl Pts',(-40.3641321823444,2.9938844645822,0.));
#25234=CARTESIAN_POINT('Ctrl Pts',(-40.3641321823444,2.9938844645822,18.));
#25235=CARTESIAN_POINT('Ctrl Pts',(-40.4584247445196,2.96375636417323,0.));
#25236=CARTESIAN_POINT('Ctrl Pts',(-40.4584247445196,2.96375636417323,18.));
#25237=CARTESIAN_POINT('Ctrl Pts',(-40.5526520010651,2.93296560822894,0.));
#25238=CARTESIAN_POINT('Ctrl Pts',(-40.5526520010651,2.93296560822894,18.));
#25239=CARTESIAN_POINT('Ctrl Pts',(-40.6468119976928,2.90152548734343,0.));
#25240=CARTESIAN_POINT('Ctrl Pts',(-40.6468119976928,2.90152548734343,18.));
#25241=CARTESIAN_POINT('Ctrl Pts',(-40.7409028213129,2.86944892209898,0.));
#25242=CARTESIAN_POINT('Ctrl Pts',(-40.7409028213129,2.86944892209898,18.));
#25243=CARTESIAN_POINT('Ctrl Pts',(-40.8349226258683,2.8367463594668,0.));
#25244=CARTESIAN_POINT('Ctrl Pts',(-40.8349226258683,2.8367463594668,18.));
#25245=CARTESIAN_POINT('Ctrl Pts',(-40.9288696352159,2.80342531768405,0.));
#25246=CARTESIAN_POINT('Ctrl Pts',(-40.9288696352159,2.80342531768405,18.));
#25247=CARTESIAN_POINT('Ctrl Pts',(-41.0227421242398,2.76949151194864,0.));
#25248=CARTESIAN_POINT('Ctrl Pts',(-41.0227421242398,2.76949151194864,18.));
#25249=CARTESIAN_POINT('Ctrl Pts',(-41.1165384061145,2.73494956725006,0.));
#25250=CARTESIAN_POINT('Ctrl Pts',(-41.1165384061145,2.73494956725006,18.));
#25251=CARTESIAN_POINT('Ctrl Pts',(-41.2102568187956,2.69980383625016,0.));
#25252=CARTESIAN_POINT('Ctrl Pts',(-41.2102568187956,2.69980383625016,18.));
#25253=CARTESIAN_POINT('Ctrl Pts',(-41.3038957096306,2.66405934050119,0.));
#25254=CARTESIAN_POINT('Ctrl Pts',(-41.3038957096306,2.66405934050119,18.));
#25255=CARTESIAN_POINT('Ctrl Pts',(-41.3974534325937,2.62772200460657,0.));
#25256=CARTESIAN_POINT('Ctrl Pts',(-41.3974534325937,2.62772200460657,18.));
#25257=CARTESIAN_POINT('Ctrl Pts',(-41.4909283577703,2.59079818040173,0.));
#25258=CARTESIAN_POINT('Ctrl Pts',(-41.4909283577703,2.59079818040173,18.));
#25259=CARTESIAN_POINT('Ctrl Pts',(-41.5843188786284,2.55329436064184,0.));
#25260=CARTESIAN_POINT('Ctrl Pts',(-41.5843188786284,2.55329436064184,18.));
#25261=CARTESIAN_POINT('Ctrl Pts',(-41.6776234194583,2.51521684674477,0.));
#25262=CARTESIAN_POINT('Ctrl Pts',(-41.6776234194583,2.51521684674477,18.));
#25263=CARTESIAN_POINT('Ctrl Pts',(-41.7708404467533,2.47657137427693,0.));
#25264=CARTESIAN_POINT('Ctrl Pts',(-41.7708404467533,2.47657137427693,18.));
#25265=CARTESIAN_POINT('Ctrl Pts',(-41.8639684667923,2.43736301434201,0.));
#25266=CARTESIAN_POINT('Ctrl Pts',(-41.8639684667923,2.43736301434201,18.));
#25267=CARTESIAN_POINT('Ctrl Pts',(-41.9570060084039,2.39759639399648,0.));
#25268=CARTESIAN_POINT('Ctrl Pts',(-41.9570060084039,2.39759639399648,18.));
#25269=CARTESIAN_POINT('Ctrl Pts',(-42.0499516093661,2.3572758406643,0.));
#25270=CARTESIAN_POINT('Ctrl Pts',(-42.0499516093661,2.3572758406643,18.));
#25271=CARTESIAN_POINT('Ctrl Pts',(-42.1428038039937,2.3164055474281,0.));
#25272=CARTESIAN_POINT('Ctrl Pts',(-42.1428038039937,2.3164055474281,18.));
#25273=CARTESIAN_POINT('Ctrl Pts',(-42.2355611060784,2.27498976664775,0.));
#25274=CARTESIAN_POINT('Ctrl Pts',(-42.2355611060784,2.27498976664775,18.));
#25275=CARTESIAN_POINT('Ctrl Pts',(-42.3282220118033,2.233032874655,0.));
#25276=CARTESIAN_POINT('Ctrl Pts',(-42.3282220118033,2.233032874655,18.));
#25277=CARTESIAN_POINT('Ctrl Pts',(-42.4207850290047,2.19053924976738,0.));
#25278=CARTESIAN_POINT('Ctrl Pts',(-42.4207850290047,2.19053924976738,18.));
#25279=CARTESIAN_POINT('Ctrl Pts',(-42.5132487024335,2.14751319676746,0.));
#25280=CARTESIAN_POINT('Ctrl Pts',(-42.5132487024335,2.14751319676746,18.));
#25281=CARTESIAN_POINT('Ctrl Pts',(-42.6056116373456,2.10395886401771,0.));
#25282=CARTESIAN_POINT('Ctrl Pts',(-42.6056116373456,2.10395886401771,18.));
#25283=CARTESIAN_POINT('Ctrl Pts',(-42.6978725343209,2.0598801492452,0.));
#25284=CARTESIAN_POINT('Ctrl Pts',(-42.6978725343209,2.0598801492452,18.));
#25285=CARTESIAN_POINT('Ctrl Pts',(-42.7900301875309,2.0152806752809,0.));
#25286=CARTESIAN_POINT('Ctrl Pts',(-42.7900301875309,2.0152806752809,18.));
#25287=CARTESIAN_POINT('Ctrl Pts',(-42.8820834139973,1.97016390194217,0.));
#25288=CARTESIAN_POINT('Ctrl Pts',(-42.8820834139973,1.97016390194217,18.));
#25289=CARTESIAN_POINT('Ctrl Pts',(-42.9740309956624,1.92453321512436,0.));
#25290=CARTESIAN_POINT('Ctrl Pts',(-42.9740309956624,1.92453321512436,18.));
#25291=CARTESIAN_POINT('Ctrl Pts',(-43.065871623255,1.8783920201461,0.));
#25292=CARTESIAN_POINT('Ctrl Pts',(-43.065871623255,1.8783920201461,18.));
#25293=CARTESIAN_POINT('Ctrl Pts',(-43.1576038253643,1.83174385734712,0.));
#25294=CARTESIAN_POINT('Ctrl Pts',(-43.1576038253643,1.83174385734712,18.));
#25295=CARTESIAN_POINT('Ctrl Pts',(-43.2492259505872,1.7845924484277,0.));
#25296=CARTESIAN_POINT('Ctrl Pts',(-43.2492259505872,1.7845924484277,18.));
#25297=CARTESIAN_POINT('Ctrl Pts',(-43.3407363140236,1.73694151741124,0.));
#25298=CARTESIAN_POINT('Ctrl Pts',(-43.3407363140236,1.73694151741124,18.));
#25299=CARTESIAN_POINT('Ctrl Pts',(-43.4321333178711,1.68879465270609,0.));
#25300=CARTESIAN_POINT('Ctrl Pts',(-43.4321333178711,1.68879465270609,18.));
#25301=CARTESIAN_POINT('Ctrl Pts',(-43.5234155788248,1.64015515906649,0.));
#25302=CARTESIAN_POINT('Ctrl Pts',(-43.5234155788248,1.64015515906649,18.));
#25303=CARTESIAN_POINT('Ctrl Pts',(-43.6145820637333,1.59102591108104,0.));
#25304=CARTESIAN_POINT('Ctrl Pts',(-43.6145820637333,1.59102591108104,18.));
#25305=CARTESIAN_POINT('Ctrl Pts',(-43.7056321934163,1.54140922714765,0.));
#25306=CARTESIAN_POINT('Ctrl Pts',(-43.7056321934163,1.54140922714765,18.));
#25307=CARTESIAN_POINT('Ctrl Pts',(-43.7965657112708,1.49130689006067,0.));
#25308=CARTESIAN_POINT('Ctrl Pts',(-43.7965657112708,1.49130689006067,18.));
#25309=CARTESIAN_POINT('Ctrl Pts',(-43.8692192047561,1.45083750111683,0.));
#25310=CARTESIAN_POINT('Ctrl Pts',(-43.8692192047561,1.45083750111683,18.));
#25311=CARTESIAN_POINT('Ctrl Pts',(-43.9236568607623,1.42026781296157,0.));
#25312=CARTESIAN_POINT('Ctrl Pts',(-43.9236568607623,1.42026781296157,18.));
#25313=CARTESIAN_POINT('Ctrl Pts',(-43.9599253218252,1.39979132121932,0.));
#25314=CARTESIAN_POINT('Ctrl Pts',(-43.9599253218252,1.39979132121932,18.));
#25315=CARTESIAN_POINT('Ctrl Pts',(-43.9780537249529,1.38952890043917,0.));
#25316=CARTESIAN_POINT('Ctrl Pts',(-43.9780537249529,1.38952890043917,18.));
#25317=CARTESIAN_POINT('Ctrl Pts',(-37.4237196983923,3.50724370857673,0.));
#25318=CARTESIAN_POINT('Ctrl Pts',(-37.4426037737699,3.50901346997657,0.));
#25319=CARTESIAN_POINT('Ctrl Pts',(-37.4803889700239,3.51204731876362,0.));
#25320=CARTESIAN_POINT('Ctrl Pts',(-37.5371179004295,3.5150810906521,0.));
#25321=CARTESIAN_POINT('Ctrl Pts',(-37.6128545966533,3.51624243734645,0.));
#25322=CARTESIAN_POINT('Ctrl Pts',(-37.7076643105286,3.51375922979958,0.));
#25323=CARTESIAN_POINT('Ctrl Pts',(-37.8025803811856,3.50844720825129,0.));
#25324=CARTESIAN_POINT('Ctrl Pts',(-37.8975688353863,3.50139628556084,0.));
#25325=CARTESIAN_POINT('Ctrl Pts',(-37.9926009950482,3.49340804454646,0.));
#25326=CARTESIAN_POINT('Ctrl Pts',(-38.0876589224537,3.48478279878234,0.));
#25327=CARTESIAN_POINT('Ctrl Pts',(-38.1827321816559,3.47549027265412,0.));
#25328=CARTESIAN_POINT('Ctrl Pts',(-38.2778154909527,3.46530185256873,0.));
#25329=CARTESIAN_POINT('Ctrl Pts',(-38.3729061502716,3.45393053211023,0.));
#25330=CARTESIAN_POINT('Ctrl Pts',(-38.4680013094732,3.44118343200304,0.));
#25331=CARTESIAN_POINT('Ctrl Pts',(-38.5630961226878,3.42705871084997,0.));
#25332=CARTESIAN_POINT('Ctrl Pts',(-38.6581847668347,3.41166717511901,0.));
#25333=CARTESIAN_POINT('Ctrl Pts',(-38.7532609709905,3.39518333281819,0.));
#25334=CARTESIAN_POINT('Ctrl Pts',(-38.8483186930884,3.37778863054482,0.));
#25335=CARTESIAN_POINT('Ctrl Pts',(-38.9433528420174,3.35960922799481,0.));
#25336=CARTESIAN_POINT('Ctrl Pts',(-39.0383596151636,3.34068601264473,0.));
#25337=CARTESIAN_POINT('Ctrl Pts',(-39.1333360409949,3.32100933979558,0.));
#25338=CARTESIAN_POINT('Ctrl Pts',(-39.2282796893977,3.30054018081688,0.));
#25339=CARTESIAN_POINT('Ctrl Pts',(-39.3231883392913,3.27923485388118,0.));
#25340=CARTESIAN_POINT('Ctrl Pts',(-39.4180596080755,3.25707264313388,0.));
#25341=CARTESIAN_POINT('Ctrl Pts',(-39.5128908052622,3.23406609691661,0.));
#25342=CARTESIAN_POINT('Ctrl Pts',(-39.607679107639,3.21024640045596,0.));
#25343=CARTESIAN_POINT('Ctrl Pts',(-39.7024216585552,3.18565465503836,0.));
#25344=CARTESIAN_POINT('Ctrl Pts',(-39.7971156880138,3.16033160752804,0.));
#25345=CARTESIAN_POINT('Ctrl Pts',(-39.8917586491576,3.13430604330356,0.));
#25346=CARTESIAN_POINT('Ctrl Pts',(-39.9863482523153,3.10759149802908,0.));
#25347=CARTESIAN_POINT('Ctrl Pts',(-40.0808823811787,3.08019251155016,0.));
#25348=CARTESIAN_POINT('Ctrl Pts',(-40.1753590391515,3.05210847423071,0.));
#25349=CARTESIAN_POINT('Ctrl Pts',(-40.2697762886113,3.02333808901596,0.));
#25350=CARTESIAN_POINT('Ctrl Pts',(-40.3641321823444,2.9938844645822,0.));
#25351=CARTESIAN_POINT('Ctrl Pts',(-40.4584247445196,2.96375636417323,0.));
#25352=CARTESIAN_POINT('Ctrl Pts',(-40.5526520010651,2.93296560822894,0.));
#25353=CARTESIAN_POINT('Ctrl Pts',(-40.6468119976928,2.90152548734343,0.));
#25354=CARTESIAN_POINT('Ctrl Pts',(-40.7409028213129,2.86944892209898,0.));
#25355=CARTESIAN_POINT('Ctrl Pts',(-40.8349226258683,2.8367463594668,0.));
#25356=CARTESIAN_POINT('Ctrl Pts',(-40.9288696352159,2.80342531768405,0.));
#25357=CARTESIAN_POINT('Ctrl Pts',(-41.0227421242398,2.76949151194864,0.));
#25358=CARTESIAN_POINT('Ctrl Pts',(-41.1165384061145,2.73494956725006,0.));
#25359=CARTESIAN_POINT('Ctrl Pts',(-41.2102568187956,2.69980383625016,0.));
#25360=CARTESIAN_POINT('Ctrl Pts',(-41.3038957096306,2.66405934050119,0.));
#25361=CARTESIAN_POINT('Ctrl Pts',(-41.3974534325937,2.62772200460657,0.));
#25362=CARTESIAN_POINT('Ctrl Pts',(-41.4909283577703,2.59079818040173,0.));
#25363=CARTESIAN_POINT('Ctrl Pts',(-41.5843188786284,2.55329436064184,0.));
#25364=CARTESIAN_POINT('Ctrl Pts',(-41.6776234194583,2.51521684674477,0.));
#25365=CARTESIAN_POINT('Ctrl Pts',(-41.7708404467533,2.47657137427693,0.));
#25366=CARTESIAN_POINT('Ctrl Pts',(-41.8639684667923,2.43736301434201,0.));
#25367=CARTESIAN_POINT('Ctrl Pts',(-41.9570060084039,2.39759639399648,0.));
#25368=CARTESIAN_POINT('Ctrl Pts',(-42.0499516093661,2.3572758406643,0.));
#25369=CARTESIAN_POINT('Ctrl Pts',(-42.1428038039937,2.3164055474281,0.));
#25370=CARTESIAN_POINT('Ctrl Pts',(-42.2355611060784,2.27498976664775,0.));
#25371=CARTESIAN_POINT('Ctrl Pts',(-42.3282220118033,2.233032874655,0.));
#25372=CARTESIAN_POINT('Ctrl Pts',(-42.4207850290047,2.19053924976738,0.));
#25373=CARTESIAN_POINT('Ctrl Pts',(-42.5132487024335,2.14751319676746,0.));
#25374=CARTESIAN_POINT('Ctrl Pts',(-42.6056116373456,2.10395886401771,0.));
#25375=CARTESIAN_POINT('Ctrl Pts',(-42.6978725343209,2.0598801492452,0.));
#25376=CARTESIAN_POINT('Ctrl Pts',(-42.7900301875309,2.0152806752809,0.));
#25377=CARTESIAN_POINT('Ctrl Pts',(-42.8820834139973,1.97016390194217,0.));
#25378=CARTESIAN_POINT('Ctrl Pts',(-42.9740309956624,1.92453321512436,0.));
#25379=CARTESIAN_POINT('Ctrl Pts',(-43.065871623255,1.8783920201461,0.));
#25380=CARTESIAN_POINT('Ctrl Pts',(-43.1576038253643,1.83174385734712,0.));
#25381=CARTESIAN_POINT('Ctrl Pts',(-43.2492259505872,1.7845924484277,0.));
#25382=CARTESIAN_POINT('Ctrl Pts',(-43.3407363140236,1.73694151741124,0.));
#25383=CARTESIAN_POINT('Ctrl Pts',(-43.4321333178711,1.68879465270609,0.));
#25384=CARTESIAN_POINT('Ctrl Pts',(-43.5234155788248,1.64015515906649,0.));
#25385=CARTESIAN_POINT('Ctrl Pts',(-43.6145820637333,1.59102591108104,0.));
#25386=CARTESIAN_POINT('Ctrl Pts',(-43.7238422193529,1.53148589036097,0.));
#25387=CARTESIAN_POINT('Ctrl Pts',(-43.8147465842503,1.48126213998559,0.));
#25388=CARTESIAN_POINT('Ctrl Pts',(-43.8873767449247,1.44069595482724,0.));
#25389=CARTESIAN_POINT('Ctrl Pts',(-43.9417969186811,1.41005374202873,0.));
#25390=CARTESIAN_POINT('Ctrl Pts',(-43.9780537249529,1.38952890043917,0.));
#25391=CARTESIAN_POINT('Ctrl Pts',(-37.4237196983923,3.50724370857673,15.));
#25392=CARTESIAN_POINT('Ctrl Pts',(-37.4426037737699,3.50901346997657,15.));
#25393=CARTESIAN_POINT('Ctrl Pts',(-37.4803889700239,3.51204731876362,15.));
#25394=CARTESIAN_POINT('Ctrl Pts',(-37.5371179004295,3.5150810906521,15.));
#25395=CARTESIAN_POINT('Ctrl Pts',(-37.6128545966533,3.51624243734645,15.));
#25396=CARTESIAN_POINT('Ctrl Pts',(-37.7076643105286,3.51375922979958,15.));
#25397=CARTESIAN_POINT('Ctrl Pts',(-37.8025803811856,3.50844720825129,15.));
#25398=CARTESIAN_POINT('Ctrl Pts',(-37.8975688353863,3.50139628556084,15.));
#25399=CARTESIAN_POINT('Ctrl Pts',(-37.9926009950482,3.49340804454646,15.));
#25400=CARTESIAN_POINT('Ctrl Pts',(-38.0876589224537,3.48478279878234,15.));
#25401=CARTESIAN_POINT('Ctrl Pts',(-38.1827321816559,3.47549027265412,15.));
#25402=CARTESIAN_POINT('Ctrl Pts',(-38.2778154909527,3.46530185256873,15.));
#25403=CARTESIAN_POINT('Ctrl Pts',(-38.3729061502716,3.45393053211023,15.));
#25404=CARTESIAN_POINT('Ctrl Pts',(-38.4680013094732,3.44118343200304,15.));
#25405=CARTESIAN_POINT('Ctrl Pts',(-38.5630961226878,3.42705871084997,15.));
#25406=CARTESIAN_POINT('Ctrl Pts',(-38.6581847668347,3.41166717511901,15.));
#25407=CARTESIAN_POINT('Ctrl Pts',(-38.7532609709905,3.39518333281819,15.));
#25408=CARTESIAN_POINT('Ctrl Pts',(-38.8483186930884,3.37778863054482,15.));
#25409=CARTESIAN_POINT('Ctrl Pts',(-38.9433528420174,3.35960922799481,15.));
#25410=CARTESIAN_POINT('Ctrl Pts',(-39.0383596151636,3.34068601264473,15.));
#25411=CARTESIAN_POINT('Ctrl Pts',(-39.1333360409949,3.32100933979558,15.));
#25412=CARTESIAN_POINT('Ctrl Pts',(-39.2282796893977,3.30054018081688,15.));
#25413=CARTESIAN_POINT('Ctrl Pts',(-39.3231883392913,3.27923485388118,15.));
#25414=CARTESIAN_POINT('Ctrl Pts',(-39.4180596080755,3.25707264313388,15.));
#25415=CARTESIAN_POINT('Ctrl Pts',(-39.5128908052622,3.23406609691661,15.));
#25416=CARTESIAN_POINT('Ctrl Pts',(-39.607679107639,3.21024640045596,15.));
#25417=CARTESIAN_POINT('Ctrl Pts',(-39.7024216585552,3.18565465503836,15.));
#25418=CARTESIAN_POINT('Ctrl Pts',(-39.7971156880138,3.16033160752804,15.));
#25419=CARTESIAN_POINT('Ctrl Pts',(-39.8917586491576,3.13430604330356,15.));
#25420=CARTESIAN_POINT('Ctrl Pts',(-39.9863482523153,3.10759149802908,15.));
#25421=CARTESIAN_POINT('Ctrl Pts',(-40.0808823811787,3.08019251155016,15.));
#25422=CARTESIAN_POINT('Ctrl Pts',(-40.1753590391515,3.05210847423071,15.));
#25423=CARTESIAN_POINT('Ctrl Pts',(-40.2697762886113,3.02333808901596,15.));
#25424=CARTESIAN_POINT('Ctrl Pts',(-40.3641321823444,2.9938844645822,15.));
#25425=CARTESIAN_POINT('Ctrl Pts',(-40.4584247445196,2.96375636417323,15.));
#25426=CARTESIAN_POINT('Ctrl Pts',(-40.5526520010651,2.93296560822894,15.));
#25427=CARTESIAN_POINT('Ctrl Pts',(-40.6468119976928,2.90152548734343,15.));
#25428=CARTESIAN_POINT('Ctrl Pts',(-40.7409028213129,2.86944892209898,15.));
#25429=CARTESIAN_POINT('Ctrl Pts',(-40.8349226258683,2.8367463594668,15.));
#25430=CARTESIAN_POINT('Ctrl Pts',(-40.9288696352159,2.80342531768405,15.));
#25431=CARTESIAN_POINT('Ctrl Pts',(-41.0227421242398,2.76949151194864,15.));
#25432=CARTESIAN_POINT('Ctrl Pts',(-41.1165384061145,2.73494956725006,15.));
#25433=CARTESIAN_POINT('Ctrl Pts',(-41.2102568187956,2.69980383625016,15.));
#25434=CARTESIAN_POINT('Ctrl Pts',(-41.3038957096306,2.66405934050119,15.));
#25435=CARTESIAN_POINT('Ctrl Pts',(-41.3974534325937,2.62772200460657,15.));
#25436=CARTESIAN_POINT('Ctrl Pts',(-41.4909283577703,2.59079818040173,15.));
#25437=CARTESIAN_POINT('Ctrl Pts',(-41.5843188786284,2.55329436064184,15.));
#25438=CARTESIAN_POINT('Ctrl Pts',(-41.6776234194583,2.51521684674477,15.));
#25439=CARTESIAN_POINT('Ctrl Pts',(-41.7708404467533,2.47657137427693,15.));
#25440=CARTESIAN_POINT('Ctrl Pts',(-41.8639684667923,2.43736301434201,15.));
#25441=CARTESIAN_POINT('Ctrl Pts',(-41.9570060084039,2.39759639399648,15.));
#25442=CARTESIAN_POINT('Ctrl Pts',(-42.0499516093661,2.3572758406643,15.));
#25443=CARTESIAN_POINT('Ctrl Pts',(-42.1428038039937,2.3164055474281,15.));
#25444=CARTESIAN_POINT('Ctrl Pts',(-42.2355611060784,2.27498976664775,15.));
#25445=CARTESIAN_POINT('Ctrl Pts',(-42.3282220118033,2.233032874655,15.));
#25446=CARTESIAN_POINT('Ctrl Pts',(-42.4207850290047,2.19053924976738,15.));
#25447=CARTESIAN_POINT('Ctrl Pts',(-42.5132487024335,2.14751319676746,15.));
#25448=CARTESIAN_POINT('Ctrl Pts',(-42.6056116373456,2.10395886401771,15.));
#25449=CARTESIAN_POINT('Ctrl Pts',(-42.6978725343209,2.0598801492452,15.));
#25450=CARTESIAN_POINT('Ctrl Pts',(-42.7900301875309,2.0152806752809,15.));
#25451=CARTESIAN_POINT('Ctrl Pts',(-42.8820834139973,1.97016390194217,15.));
#25452=CARTESIAN_POINT('Ctrl Pts',(-42.9740309956624,1.92453321512436,15.));
#25453=CARTESIAN_POINT('Ctrl Pts',(-43.065871623255,1.8783920201461,15.));
#25454=CARTESIAN_POINT('Ctrl Pts',(-43.1576038253643,1.83174385734712,15.));
#25455=CARTESIAN_POINT('Ctrl Pts',(-43.2492259505872,1.7845924484277,15.));
#25456=CARTESIAN_POINT('Ctrl Pts',(-43.3407363140236,1.73694151741124,15.));
#25457=CARTESIAN_POINT('Ctrl Pts',(-43.4321333178711,1.68879465270609,15.));
#25458=CARTESIAN_POINT('Ctrl Pts',(-43.5234155788248,1.64015515906649,15.));
#25459=CARTESIAN_POINT('Ctrl Pts',(-43.6145820637333,1.59102591108104,15.));
#25460=CARTESIAN_POINT('Ctrl Pts',(-43.7238422193529,1.53148589036097,15.));
#25461=CARTESIAN_POINT('Ctrl Pts',(-43.8147465842503,1.48126213998559,15.));
#25462=CARTESIAN_POINT('Ctrl Pts',(-43.8873767449247,1.44069595482724,15.));
#25463=CARTESIAN_POINT('Ctrl Pts',(-43.9417969186811,1.41005374202873,15.));
#25464=CARTESIAN_POINT('Ctrl Pts',(-43.9780537249529,1.38952890043917,15.));
#25465=CARTESIAN_POINT('Ctrl Pts',(-42.2550026135057,12.2684454652018,0.));
#25466=CARTESIAN_POINT('Ctrl Pts',(-42.2550026135057,12.2684454652018,18.));
#25467=CARTESIAN_POINT('Ctrl Pts',(-42.2409327400055,12.2530833383985,0.));
#25468=CARTESIAN_POINT('Ctrl Pts',(-42.2409327400055,12.2530833383985,18.));
#25469=CARTESIAN_POINT('Ctrl Pts',(-42.2127669677092,12.222401466668,0.));
#25470=CARTESIAN_POINT('Ctrl Pts',(-42.2127669677092,12.222401466668,18.));
#25471=CARTESIAN_POINT('Ctrl Pts',(-42.1704402333854,12.1765058047069,0.));
#25472=CARTESIAN_POINT('Ctrl Pts',(-42.1704402333854,12.1765058047069,18.));
#25473=CARTESIAN_POINT('Ctrl Pts',(-42.1138483839101,12.1155659644537,0.));
#25474=CARTESIAN_POINT('Ctrl Pts',(-42.1138483839101,12.1155659644537,18.));
#25475=CARTESIAN_POINT('Ctrl Pts',(-42.0428479428228,12.0398158079102,0.));
#25476=CARTESIAN_POINT('Ctrl Pts',(-42.0428479428228,12.0398158079102,18.));
#25477=CARTESIAN_POINT('Ctrl Pts',(-41.9715865222182,11.9644914999263,0.));
#25478=CARTESIAN_POINT('Ctrl Pts',(-41.9715865222182,11.9644914999263,18.));
#25479=CARTESIAN_POINT('Ctrl Pts',(-41.9000638152266,11.8895948153349,0.));
#25480=CARTESIAN_POINT('Ctrl Pts',(-41.9000638152266,11.8895948153349,18.));
#25481=CARTESIAN_POINT('Ctrl Pts',(-41.8282796562569,11.81512813804,0.));
#25482=CARTESIAN_POINT('Ctrl Pts',(-41.8282796562569,11.81512813804,18.));
#25483=CARTESIAN_POINT('Ctrl Pts',(-41.7562341395977,11.7410945211992,0.));
#25484=CARTESIAN_POINT('Ctrl Pts',(-41.7562341395977,11.7410945211992,18.));
#25485=CARTESIAN_POINT('Ctrl Pts',(-41.6839275596248,11.6674975352852,0.));
#25486=CARTESIAN_POINT('Ctrl Pts',(-41.6839275596248,11.6674975352852,18.));
#25487=CARTESIAN_POINT('Ctrl Pts',(-41.6113603270596,11.5943410868252,0.));
#25488=CARTESIAN_POINT('Ctrl Pts',(-41.6113603270596,11.5943410868252,18.));
#25489=CARTESIAN_POINT('Ctrl Pts',(-41.5385328935506,11.5216292382388,0.));
#25490=CARTESIAN_POINT('Ctrl Pts',(-41.5385328935506,11.5216292382388,18.));
#25491=CARTESIAN_POINT('Ctrl Pts',(-41.4654456796071,11.4493660393849,0.));
#25492=CARTESIAN_POINT('Ctrl Pts',(-41.4654456796071,11.4493660393849,18.));
#25493=CARTESIAN_POINT('Ctrl Pts',(-41.3920989905986,11.3775553120176,0.));
#25494=CARTESIAN_POINT('Ctrl Pts',(-41.3920989905986,11.3775553120176,18.));
#25495=CARTESIAN_POINT('Ctrl Pts',(-41.3184930194148,11.3062006993745,0.));
#25496=CARTESIAN_POINT('Ctrl Pts',(-41.3184930194148,11.3062006993745,18.));
#25497=CARTESIAN_POINT('Ctrl Pts',(-41.2446278781981,11.2353057980338,0.));
#25498=CARTESIAN_POINT('Ctrl Pts',(-41.2446278781981,11.2353057980338,18.));
#25499=CARTESIAN_POINT('Ctrl Pts',(-41.1705036228854,11.1648742640378,0.));
#25500=CARTESIAN_POINT('Ctrl Pts',(-41.1705036228854,11.1648742640378,18.));
#25501=CARTESIAN_POINT('Ctrl Pts',(-41.0961202807715,11.0949099155251,0.));
#25502=CARTESIAN_POINT('Ctrl Pts',(-41.0961202807715,11.0949099155251,18.));
#25503=CARTESIAN_POINT('Ctrl Pts',(-41.0214778832142,11.0254168609972,0.));
#25504=CARTESIAN_POINT('Ctrl Pts',(-41.0214778832142,11.0254168609972,18.));
#25505=CARTESIAN_POINT('Ctrl Pts',(-40.9465764747798,10.956399476781,0.));
#25506=CARTESIAN_POINT('Ctrl Pts',(-40.9465764747798,10.956399476781,18.));
#25507=CARTESIAN_POINT('Ctrl Pts',(-40.8714161092412,10.8878623066646,0.));
#25508=CARTESIAN_POINT('Ctrl Pts',(-40.8714161092412,10.8878623066646,18.));
#25509=CARTESIAN_POINT('Ctrl Pts',(-40.7959968527561,10.8198099757795,0.));
#25510=CARTESIAN_POINT('Ctrl Pts',(-40.7959968527561,10.8198099757795,18.));
#25511=CARTESIAN_POINT('Ctrl Pts',(-40.7203187831783,10.7522471109694,0.));
#25512=CARTESIAN_POINT('Ctrl Pts',(-40.7203187831783,10.7522471109694,18.));
#25513=CARTESIAN_POINT('Ctrl Pts',(-40.6443819999244,10.6851782157325,0.));
#25514=CARTESIAN_POINT('Ctrl Pts',(-40.6443819999244,10.6851782157325,18.));
#25515=CARTESIAN_POINT('Ctrl Pts',(-40.5681866012103,10.618607730849,0.));
#25516=CARTESIAN_POINT('Ctrl Pts',(-40.5681866012103,10.618607730849,18.));
#25517=CARTESIAN_POINT('Ctrl Pts',(-40.4917326404439,10.5525402237951,0.));
#25518=CARTESIAN_POINT('Ctrl Pts',(-40.4917326404439,10.5525402237951,18.));
#25519=CARTESIAN_POINT('Ctrl Pts',(-40.4150200869536,10.48698054978,0.));
#25520=CARTESIAN_POINT('Ctrl Pts',(-40.4150200869536,10.48698054978,18.));
#25521=CARTESIAN_POINT('Ctrl Pts',(-40.3380487942952,10.4219339932951,0.));
#25522=CARTESIAN_POINT('Ctrl Pts',(-40.3380487942952,10.4219339932951,18.));
#25523=CARTESIAN_POINT('Ctrl Pts',(-40.2608184485326,10.3574064830678,0.));
#25524=CARTESIAN_POINT('Ctrl Pts',(-40.2608184485326,10.3574064830678,18.));
#25525=CARTESIAN_POINT('Ctrl Pts',(-40.1833286010098,10.2934044990237,0.));
#25526=CARTESIAN_POINT('Ctrl Pts',(-40.1833286010098,10.2934044990237,18.));
#25527=CARTESIAN_POINT('Ctrl Pts',(-40.1055787732578,10.2299347125857,0.));
#25528=CARTESIAN_POINT('Ctrl Pts',(-40.1055787732578,10.2299347125857,18.));
#25529=CARTESIAN_POINT('Ctrl Pts',(-40.0275685525923,10.1670036683795,0.));
#25530=CARTESIAN_POINT('Ctrl Pts',(-40.0275685525923,10.1670036683795,18.));
#25531=CARTESIAN_POINT('Ctrl Pts',(-39.9492976736738,10.1046175096878,0.));
#25532=CARTESIAN_POINT('Ctrl Pts',(-39.9492976736738,10.1046175096878,18.));
#25533=CARTESIAN_POINT('Ctrl Pts',(-39.8707661565233,10.0427815229883,0.));
#25534=CARTESIAN_POINT('Ctrl Pts',(-39.8707661565233,10.0427815229883,18.));
#25535=CARTESIAN_POINT('Ctrl Pts',(-39.7919742367922,9.98150036150823,0.));
#25536=CARTESIAN_POINT('Ctrl Pts',(-39.7919742367922,9.98150036150823,18.));
#25537=CARTESIAN_POINT('Ctrl Pts',(-39.712922089547,9.92077894513192,0.));
#25538=CARTESIAN_POINT('Ctrl Pts',(-39.712922089547,9.92077894513192,18.));
#25539=CARTESIAN_POINT('Ctrl Pts',(-39.6336095893767,9.8606232424256,0.));
#25540=CARTESIAN_POINT('Ctrl Pts',(-39.6336095893767,9.8606232424256,18.));
#25541=CARTESIAN_POINT('Ctrl Pts',(-39.5540361022309,9.80104095251614,0.));
#25542=CARTESIAN_POINT('Ctrl Pts',(-39.5540361022309,9.80104095251614,18.));
#25543=CARTESIAN_POINT('Ctrl Pts',(-39.4742001555227,9.74204258152664,0.));
#25544=CARTESIAN_POINT('Ctrl Pts',(-39.4742001555227,9.74204258152664,18.));
#25545=CARTESIAN_POINT('Ctrl Pts',(-39.3940995760289,9.68364100883827,0.));
#25546=CARTESIAN_POINT('Ctrl Pts',(-39.3940995760289,9.68364100883827,18.));
#25547=CARTESIAN_POINT('Ctrl Pts',(-39.3137321153686,9.62584947846543,0.));
#25548=CARTESIAN_POINT('Ctrl Pts',(-39.3137321153686,9.62584947846543,18.));
#25549=CARTESIAN_POINT('Ctrl Pts',(-39.2330959982788,9.56867984233623,0.));
#25550=CARTESIAN_POINT('Ctrl Pts',(-39.2330959982788,9.56867984233623,18.));
#25551=CARTESIAN_POINT('Ctrl Pts',(-39.1521903958955,9.51214104535621,0.));
#25552=CARTESIAN_POINT('Ctrl Pts',(-39.1521903958955,9.51214104535621,18.));
#25553=CARTESIAN_POINT('Ctrl Pts',(-39.071016199495,9.45623664577432,0.));
#25554=CARTESIAN_POINT('Ctrl Pts',(-39.071016199495,9.45623664577432,18.));
#25555=CARTESIAN_POINT('Ctrl Pts',(-38.9895756526779,9.40096600877644,0.));
#25556=CARTESIAN_POINT('Ctrl Pts',(-38.9895756526779,9.40096600877644,18.));
#25557=CARTESIAN_POINT('Ctrl Pts',(-38.9078708427078,9.34632917154637,0.));
#25558=CARTESIAN_POINT('Ctrl Pts',(-38.9078708427078,9.34632917154637,18.));
#25559=CARTESIAN_POINT('Ctrl Pts',(-38.8259023794241,9.29233110570903,0.));
#25560=CARTESIAN_POINT('Ctrl Pts',(-38.8259023794241,9.29233110570903,18.));
#25561=CARTESIAN_POINT('Ctrl Pts',(-38.7436682576832,9.23898539199332,0.));
#25562=CARTESIAN_POINT('Ctrl Pts',(-38.7436682576832,9.23898539199332,18.));
#25563=CARTESIAN_POINT('Ctrl Pts',(-38.6611620045193,9.1863201939433,0.));
#25564=CARTESIAN_POINT('Ctrl Pts',(-38.6611620045193,9.1863201939433,18.));
#25565=CARTESIAN_POINT('Ctrl Pts',(-38.5783736628826,9.13437512010586,0.));
#25566=CARTESIAN_POINT('Ctrl Pts',(-38.5783736628826,9.13437512010586,18.));
#25567=CARTESIAN_POINT('Ctrl Pts',(-38.4952932486131,9.08319014288086,0.));
#25568=CARTESIAN_POINT('Ctrl Pts',(-38.4952932486131,9.08319014288086,18.));
#25569=CARTESIAN_POINT('Ctrl Pts',(-38.4119138099805,9.03279579360191,0.));
#25570=CARTESIAN_POINT('Ctrl Pts',(-38.4119138099805,9.03279579360191,18.));
#25571=CARTESIAN_POINT('Ctrl Pts',(-38.3282340281403,8.9832048378576,0.));
#25572=CARTESIAN_POINT('Ctrl Pts',(-38.3282340281403,8.9832048378576,18.));
#25573=CARTESIAN_POINT('Ctrl Pts',(-38.2442625706309,8.93439830996339,0.));
#25574=CARTESIAN_POINT('Ctrl Pts',(-38.2442625706309,8.93439830996339,18.));
#25575=CARTESIAN_POINT('Ctrl Pts',(-38.1600150482528,8.88633535238434,0.));
#25576=CARTESIAN_POINT('Ctrl Pts',(-38.1600150482528,8.88633535238434,18.));
#25577=CARTESIAN_POINT('Ctrl Pts',(-38.0755058326913,8.83897959763349,0.));
#25578=CARTESIAN_POINT('Ctrl Pts',(-38.0755058326913,8.83897959763349,18.));
#25579=CARTESIAN_POINT('Ctrl Pts',(-37.9907407304174,8.79232279131092,0.));
#25580=CARTESIAN_POINT('Ctrl Pts',(-37.9907407304174,8.79232279131092,18.));
#25581=CARTESIAN_POINT('Ctrl Pts',(-37.9057107230066,8.74640499479002,0.));
#25582=CARTESIAN_POINT('Ctrl Pts',(-37.9057107230066,8.74640499479002,18.));
#25583=CARTESIAN_POINT('Ctrl Pts',(-37.8203816669031,8.70134776631143,0.));
#25584=CARTESIAN_POINT('Ctrl Pts',(-37.8203816669031,8.70134776631143,18.));
#25585=CARTESIAN_POINT('Ctrl Pts',(-37.7347032383719,8.65732553894525,0.));
#25586=CARTESIAN_POINT('Ctrl Pts',(-37.7347032383719,8.65732553894525,18.));
#25587=CARTESIAN_POINT('Ctrl Pts',(-37.6486274754754,8.61450621749155,0.));
#25588=CARTESIAN_POINT('Ctrl Pts',(-37.6486274754754,8.61450621749155,18.));
#25589=CARTESIAN_POINT('Ctrl Pts',(-37.5621256752108,8.57299698459466,0.));
#25590=CARTESIAN_POINT('Ctrl Pts',(-37.5621256752108,8.57299698459466,18.));
#25591=CARTESIAN_POINT('Ctrl Pts',(-37.4752030152968,8.53279758643785,0.));
#25592=CARTESIAN_POINT('Ctrl Pts',(-37.4752030152968,8.53279758643785,18.));
#25593=CARTESIAN_POINT('Ctrl Pts',(-37.3879218093514,8.49372546467076,0.));
#25594=CARTESIAN_POINT('Ctrl Pts',(-37.3879218093514,8.49372546467076,18.));
#25595=CARTESIAN_POINT('Ctrl Pts',(-37.3003733151561,8.4555084943396,0.));
#25596=CARTESIAN_POINT('Ctrl Pts',(-37.3003733151561,8.4555084943396,18.));
#25597=CARTESIAN_POINT('Ctrl Pts',(-37.2126332013933,8.41793088313261,0.));
#25598=CARTESIAN_POINT('Ctrl Pts',(-37.2126332013933,8.41793088313261,18.));
#25599=CARTESIAN_POINT('Ctrl Pts',(-37.1247207489179,8.38096706211448,0.));
#25600=CARTESIAN_POINT('Ctrl Pts',(-37.1247207489179,8.38096706211448,18.));
#25601=CARTESIAN_POINT('Ctrl Pts',(-37.0365602155148,8.3449081895264,0.));
#25602=CARTESIAN_POINT('Ctrl Pts',(-37.0365602155148,8.3449081895264,18.));
#25603=CARTESIAN_POINT('Ctrl Pts',(-36.9479311729484,8.31052547794592,0.));
#25604=CARTESIAN_POINT('Ctrl Pts',(-36.9479311729484,8.31052547794592,18.));
#25605=CARTESIAN_POINT('Ctrl Pts',(-36.8585291300917,8.27886599440785,0.));
#25606=CARTESIAN_POINT('Ctrl Pts',(-36.8585291300917,8.27886599440785,18.));
#25607=CARTESIAN_POINT('Ctrl Pts',(-36.7861403757604,8.25656657451821,0.));
#25608=CARTESIAN_POINT('Ctrl Pts',(-36.7861403757604,8.25656657451821,18.));
#25609=CARTESIAN_POINT('Ctrl Pts',(-36.7312504697652,8.24192165947368,0.));
#25610=CARTESIAN_POINT('Ctrl Pts',(-36.7312504697652,8.24192165947368,18.));
#25611=CARTESIAN_POINT('Ctrl Pts',(-36.6943771018148,8.23313075335377,0.));
#25612=CARTESIAN_POINT('Ctrl Pts',(-36.6943771018148,8.23313075335377,18.));
#25613=CARTESIAN_POINT('Ctrl Pts',(-36.6758703925241,8.22897839625061,0.));
#25614=CARTESIAN_POINT('Ctrl Pts',(-36.6758703925241,8.22897839625061,18.));
#25615=CARTESIAN_POINT('',(-42.2550026135057,12.2684454652017,0.));
#25616=CARTESIAN_POINT('Ctrl Pts',(-36.6758703925241,8.22897839625061,0.));
#25617=CARTESIAN_POINT('Ctrl Pts',(-36.6943771018148,8.23313075335377,0.));
#25618=CARTESIAN_POINT('Ctrl Pts',(-36.7312504697652,8.24192165947368,0.));
#25619=CARTESIAN_POINT('Ctrl Pts',(-36.7861403757604,8.25656657451821,0.));
#25620=CARTESIAN_POINT('Ctrl Pts',(-36.8585291300917,8.27886599440785,0.));
#25621=CARTESIAN_POINT('Ctrl Pts',(-36.9479311729484,8.31052547794592,0.));
#25622=CARTESIAN_POINT('Ctrl Pts',(-37.0365602155148,8.3449081895264,0.));
#25623=CARTESIAN_POINT('Ctrl Pts',(-37.1247207489179,8.38096706211448,0.));
#25624=CARTESIAN_POINT('Ctrl Pts',(-37.2126332013933,8.41793088313261,0.));
#25625=CARTESIAN_POINT('Ctrl Pts',(-37.3003733151561,8.4555084943396,0.));
#25626=CARTESIAN_POINT('Ctrl Pts',(-37.3879218093514,8.49372546467076,0.));
#25627=CARTESIAN_POINT('Ctrl Pts',(-37.4752030152968,8.53279758643785,0.));
#25628=CARTESIAN_POINT('Ctrl Pts',(-37.5621256752108,8.57299698459466,0.));
#25629=CARTESIAN_POINT('Ctrl Pts',(-37.6486274754754,8.61450621749155,0.));
#25630=CARTESIAN_POINT('Ctrl Pts',(-37.7347032383719,8.65732553894525,0.));
#25631=CARTESIAN_POINT('Ctrl Pts',(-37.8203816669031,8.70134776631143,0.));
#25632=CARTESIAN_POINT('Ctrl Pts',(-37.9057107230066,8.74640499479002,0.));
#25633=CARTESIAN_POINT('Ctrl Pts',(-37.9907407304174,8.79232279131092,0.));
#25634=CARTESIAN_POINT('Ctrl Pts',(-38.0755058326913,8.83897959763349,0.));
#25635=CARTESIAN_POINT('Ctrl Pts',(-38.1600150482528,8.88633535238434,0.));
#25636=CARTESIAN_POINT('Ctrl Pts',(-38.2442625706309,8.93439830996339,0.));
#25637=CARTESIAN_POINT('Ctrl Pts',(-38.3282340281403,8.9832048378576,0.));
#25638=CARTESIAN_POINT('Ctrl Pts',(-38.4119138099805,9.03279579360191,0.));
#25639=CARTESIAN_POINT('Ctrl Pts',(-38.4952932486131,9.08319014288086,0.));
#25640=CARTESIAN_POINT('Ctrl Pts',(-38.5783736628826,9.13437512010586,0.));
#25641=CARTESIAN_POINT('Ctrl Pts',(-38.6611620045193,9.1863201939433,0.));
#25642=CARTESIAN_POINT('Ctrl Pts',(-38.7436682576832,9.23898539199332,0.));
#25643=CARTESIAN_POINT('Ctrl Pts',(-38.8259023794241,9.29233110570903,0.));
#25644=CARTESIAN_POINT('Ctrl Pts',(-38.9078708427078,9.34632917154637,0.));
#25645=CARTESIAN_POINT('Ctrl Pts',(-38.9895756526779,9.40096600877644,0.));
#25646=CARTESIAN_POINT('Ctrl Pts',(-39.071016199495,9.45623664577432,0.));
#25647=CARTESIAN_POINT('Ctrl Pts',(-39.1521903958955,9.51214104535621,0.));
#25648=CARTESIAN_POINT('Ctrl Pts',(-39.2330959982788,9.56867984233623,0.));
#25649=CARTESIAN_POINT('Ctrl Pts',(-39.3137321153686,9.62584947846543,0.));
#25650=CARTESIAN_POINT('Ctrl Pts',(-39.3940995760289,9.68364100883827,0.));
#25651=CARTESIAN_POINT('Ctrl Pts',(-39.4742001555227,9.74204258152664,0.));
#25652=CARTESIAN_POINT('Ctrl Pts',(-39.5540361022309,9.80104095251614,0.));
#25653=CARTESIAN_POINT('Ctrl Pts',(-39.6336095893767,9.8606232424256,0.));
#25654=CARTESIAN_POINT('Ctrl Pts',(-39.712922089547,9.92077894513192,0.));
#25655=CARTESIAN_POINT('Ctrl Pts',(-39.7919742367922,9.98150036150823,0.));
#25656=CARTESIAN_POINT('Ctrl Pts',(-39.8707661565233,10.0427815229883,0.));
#25657=CARTESIAN_POINT('Ctrl Pts',(-39.9492976736738,10.1046175096878,0.));
#25658=CARTESIAN_POINT('Ctrl Pts',(-40.0275685525923,10.1670036683795,0.));
#25659=CARTESIAN_POINT('Ctrl Pts',(-40.1055787732578,10.2299347125857,0.));
#25660=CARTESIAN_POINT('Ctrl Pts',(-40.1833286010098,10.2934044990237,0.));
#25661=CARTESIAN_POINT('Ctrl Pts',(-40.2608184485326,10.3574064830678,0.));
#25662=CARTESIAN_POINT('Ctrl Pts',(-40.3380487942952,10.4219339932951,0.));
#25663=CARTESIAN_POINT('Ctrl Pts',(-40.4150200869536,10.48698054978,0.));
#25664=CARTESIAN_POINT('Ctrl Pts',(-40.4917326404439,10.5525402237951,0.));
#25665=CARTESIAN_POINT('Ctrl Pts',(-40.5681866012103,10.618607730849,0.));
#25666=CARTESIAN_POINT('Ctrl Pts',(-40.6443819999244,10.6851782157325,0.));
#25667=CARTESIAN_POINT('Ctrl Pts',(-40.7203187831783,10.7522471109694,0.));
#25668=CARTESIAN_POINT('Ctrl Pts',(-40.7959968527561,10.8198099757795,0.));
#25669=CARTESIAN_POINT('Ctrl Pts',(-40.8714161092412,10.8878623066646,0.));
#25670=CARTESIAN_POINT('Ctrl Pts',(-40.9465764747798,10.956399476781,0.));
#25671=CARTESIAN_POINT('Ctrl Pts',(-41.0214778832142,11.0254168609972,0.));
#25672=CARTESIAN_POINT('Ctrl Pts',(-41.0961202807715,11.0949099155251,0.));
#25673=CARTESIAN_POINT('Ctrl Pts',(-41.1705036228854,11.1648742640378,0.));
#25674=CARTESIAN_POINT('Ctrl Pts',(-41.2446278781981,11.2353057980338,0.));
#25675=CARTESIAN_POINT('Ctrl Pts',(-41.3184930194148,11.3062006993745,0.));
#25676=CARTESIAN_POINT('Ctrl Pts',(-41.3920989905986,11.3775553120176,0.));
#25677=CARTESIAN_POINT('Ctrl Pts',(-41.4654456796071,11.4493660393849,0.));
#25678=CARTESIAN_POINT('Ctrl Pts',(-41.5385328935506,11.5216292382388,0.));
#25679=CARTESIAN_POINT('Ctrl Pts',(-41.6113603270596,11.5943410868252,0.));
#25680=CARTESIAN_POINT('Ctrl Pts',(-41.6839275596248,11.6674975352852,0.));
#25681=CARTESIAN_POINT('Ctrl Pts',(-41.7562341395977,11.7410945211992,0.));
#25682=CARTESIAN_POINT('Ctrl Pts',(-41.8282796562569,11.81512813804,0.));
#25683=CARTESIAN_POINT('Ctrl Pts',(-41.9000638152266,11.8895948153349,0.));
#25684=CARTESIAN_POINT('Ctrl Pts',(-41.9715865222182,11.9644914999263,0.));
#25685=CARTESIAN_POINT('Ctrl Pts',(-42.0571002269437,12.054880669507,0.));
#25686=CARTESIAN_POINT('Ctrl Pts',(-42.1280354231517,12.1307372881904,0.));
#25687=CARTESIAN_POINT('Ctrl Pts',(-42.18457517013,12.1917619768791,0.));
#25688=CARTESIAN_POINT('Ctrl Pts',(-42.2268628664988,12.2377212115625,0.));
#25689=CARTESIAN_POINT('Ctrl Pts',(-42.2550026135057,12.2684454652018,0.));
#25690=CARTESIAN_POINT('',(-42.2550026135057,12.2684454652017,15.));
#25691=CARTESIAN_POINT('Ctrl Pts',(-42.2550026135057,12.2684454652018,15.));
#25692=CARTESIAN_POINT('Ctrl Pts',(-42.2409327400055,12.2530833383985,15.));
#25693=CARTESIAN_POINT('Ctrl Pts',(-42.2127669677092,12.222401466668,15.));
#25694=CARTESIAN_POINT('Ctrl Pts',(-42.1704402333854,12.1765058047069,15.));
#25695=CARTESIAN_POINT('Ctrl Pts',(-42.1138483839101,12.1155659644537,15.));
#25696=CARTESIAN_POINT('Ctrl Pts',(-42.0428479428228,12.0398158079102,15.));
#25697=CARTESIAN_POINT('Ctrl Pts',(-41.9715865222182,11.9644914999263,15.));
#25698=CARTESIAN_POINT('Ctrl Pts',(-41.9000638152266,11.8895948153349,15.));
#25699=CARTESIAN_POINT('Ctrl Pts',(-41.8282796562569,11.81512813804,15.));
#25700=CARTESIAN_POINT('Ctrl Pts',(-41.7562341395977,11.7410945211992,15.));
#25701=CARTESIAN_POINT('Ctrl Pts',(-41.6839275596248,11.6674975352852,15.));
#25702=CARTESIAN_POINT('Ctrl Pts',(-41.6113603270596,11.5943410868252,15.));
#25703=CARTESIAN_POINT('Ctrl Pts',(-41.5385328935506,11.5216292382388,15.));
#25704=CARTESIAN_POINT('Ctrl Pts',(-41.4654456796071,11.4493660393849,15.));
#25705=CARTESIAN_POINT('Ctrl Pts',(-41.3920989905986,11.3775553120176,15.));
#25706=CARTESIAN_POINT('Ctrl Pts',(-41.3184930194148,11.3062006993745,15.));
#25707=CARTESIAN_POINT('Ctrl Pts',(-41.2446278781981,11.2353057980338,15.));
#25708=CARTESIAN_POINT('Ctrl Pts',(-41.1705036228854,11.1648742640378,15.));
#25709=CARTESIAN_POINT('Ctrl Pts',(-41.0961202807715,11.0949099155251,15.));
#25710=CARTESIAN_POINT('Ctrl Pts',(-41.0214778832142,11.0254168609972,15.));
#25711=CARTESIAN_POINT('Ctrl Pts',(-40.9465764747798,10.956399476781,15.));
#25712=CARTESIAN_POINT('Ctrl Pts',(-40.8714161092412,10.8878623066646,15.));
#25713=CARTESIAN_POINT('Ctrl Pts',(-40.7959968527561,10.8198099757795,15.));
#25714=CARTESIAN_POINT('Ctrl Pts',(-40.7203187831783,10.7522471109694,15.));
#25715=CARTESIAN_POINT('Ctrl Pts',(-40.6443819999244,10.6851782157325,15.));
#25716=CARTESIAN_POINT('Ctrl Pts',(-40.5681866012103,10.618607730849,15.));
#25717=CARTESIAN_POINT('Ctrl Pts',(-40.4917326404439,10.5525402237951,15.));
#25718=CARTESIAN_POINT('Ctrl Pts',(-40.4150200869536,10.48698054978,15.));
#25719=CARTESIAN_POINT('Ctrl Pts',(-40.3380487942952,10.4219339932951,15.));
#25720=CARTESIAN_POINT('Ctrl Pts',(-40.2608184485326,10.3574064830678,15.));
#25721=CARTESIAN_POINT('Ctrl Pts',(-40.1833286010098,10.2934044990237,15.));
#25722=CARTESIAN_POINT('Ctrl Pts',(-40.1055787732578,10.2299347125857,15.));
#25723=CARTESIAN_POINT('Ctrl Pts',(-40.0275685525923,10.1670036683795,15.));
#25724=CARTESIAN_POINT('Ctrl Pts',(-39.9492976736738,10.1046175096878,15.));
#25725=CARTESIAN_POINT('Ctrl Pts',(-39.8707661565233,10.0427815229883,15.));
#25726=CARTESIAN_POINT('Ctrl Pts',(-39.7919742367922,9.98150036150823,15.));
#25727=CARTESIAN_POINT('Ctrl Pts',(-39.712922089547,9.92077894513192,15.));
#25728=CARTESIAN_POINT('Ctrl Pts',(-39.6336095893767,9.8606232424256,15.));
#25729=CARTESIAN_POINT('Ctrl Pts',(-39.5540361022309,9.80104095251614,15.));
#25730=CARTESIAN_POINT('Ctrl Pts',(-39.4742001555227,9.74204258152664,15.));
#25731=CARTESIAN_POINT('Ctrl Pts',(-39.3940995760289,9.68364100883827,15.));
#25732=CARTESIAN_POINT('Ctrl Pts',(-39.3137321153686,9.62584947846543,15.));
#25733=CARTESIAN_POINT('Ctrl Pts',(-39.2330959982788,9.56867984233623,15.));
#25734=CARTESIAN_POINT('Ctrl Pts',(-39.1521903958955,9.51214104535621,15.));
#25735=CARTESIAN_POINT('Ctrl Pts',(-39.071016199495,9.45623664577432,15.));
#25736=CARTESIAN_POINT('Ctrl Pts',(-38.9895756526779,9.40096600877644,15.));
#25737=CARTESIAN_POINT('Ctrl Pts',(-38.9078708427078,9.34632917154637,15.));
#25738=CARTESIAN_POINT('Ctrl Pts',(-38.8259023794241,9.29233110570903,15.));
#25739=CARTESIAN_POINT('Ctrl Pts',(-38.7436682576832,9.23898539199332,15.));
#25740=CARTESIAN_POINT('Ctrl Pts',(-38.6611620045193,9.1863201939433,15.));
#25741=CARTESIAN_POINT('Ctrl Pts',(-38.5783736628826,9.13437512010586,15.));
#25742=CARTESIAN_POINT('Ctrl Pts',(-38.4952932486131,9.08319014288086,15.));
#25743=CARTESIAN_POINT('Ctrl Pts',(-38.4119138099805,9.03279579360191,15.));
#25744=CARTESIAN_POINT('Ctrl Pts',(-38.3282340281403,8.9832048378576,15.));
#25745=CARTESIAN_POINT('Ctrl Pts',(-38.2442625706309,8.93439830996339,15.));
#25746=CARTESIAN_POINT('Ctrl Pts',(-38.1600150482528,8.88633535238434,15.));
#25747=CARTESIAN_POINT('Ctrl Pts',(-38.0755058326913,8.83897959763349,15.));
#25748=CARTESIAN_POINT('Ctrl Pts',(-37.9907407304174,8.79232279131092,15.));
#25749=CARTESIAN_POINT('Ctrl Pts',(-37.9057107230066,8.74640499479002,15.));
#25750=CARTESIAN_POINT('Ctrl Pts',(-37.8203816669031,8.70134776631143,15.));
#25751=CARTESIAN_POINT('Ctrl Pts',(-37.7347032383719,8.65732553894525,15.));
#25752=CARTESIAN_POINT('Ctrl Pts',(-37.6486274754754,8.61450621749155,15.));
#25753=CARTESIAN_POINT('Ctrl Pts',(-37.5621256752108,8.57299698459466,15.));
#25754=CARTESIAN_POINT('Ctrl Pts',(-37.4752030152968,8.53279758643785,15.));
#25755=CARTESIAN_POINT('Ctrl Pts',(-37.3879218093514,8.49372546467076,15.));
#25756=CARTESIAN_POINT('Ctrl Pts',(-37.3003733151561,8.4555084943396,15.));
#25757=CARTESIAN_POINT('Ctrl Pts',(-37.2126332013933,8.41793088313261,15.));
#25758=CARTESIAN_POINT('Ctrl Pts',(-37.1247207489179,8.38096706211448,15.));
#25759=CARTESIAN_POINT('Ctrl Pts',(-37.0365602155148,8.3449081895264,15.));
#25760=CARTESIAN_POINT('Ctrl Pts',(-36.9479311729484,8.31052547794592,15.));
#25761=CARTESIAN_POINT('Ctrl Pts',(-36.8585291300917,8.27886599440785,15.));
#25762=CARTESIAN_POINT('Ctrl Pts',(-36.7861403757604,8.25656657451821,15.));
#25763=CARTESIAN_POINT('Ctrl Pts',(-36.7312504697652,8.24192165947368,15.));
#25764=CARTESIAN_POINT('Ctrl Pts',(-36.6943771018148,8.23313075335377,15.));
#25765=CARTESIAN_POINT('Ctrl Pts',(-36.6758703925241,8.22897839625061,15.));
#25766=CARTESIAN_POINT('',(-42.2550026135057,12.2684454652017,0.));
#25767=CARTESIAN_POINT('Origin',(-1.07784724682657E-11,3.50213800024364E-12,
0.));
#25768=CARTESIAN_POINT('',(-41.396226524684,14.911486495888,0.));
#25769=CARTESIAN_POINT('Origin',(-1.07784724682657E-11,3.50213800024364E-12,
0.));
#25770=CARTESIAN_POINT('',(-41.396226524684,14.911486495888,15.));
#25771=CARTESIAN_POINT('Origin',(-1.07784724682657E-11,3.50213800024364E-12,
15.));
#25772=CARTESIAN_POINT('',(-41.396226524684,14.911486495888,0.));
#25773=CARTESIAN_POINT('Ctrl Pts',(-34.5082745737944,14.9001523628048,0.));
#25774=CARTESIAN_POINT('Ctrl Pts',(-34.5082745737944,14.9001523628048,18.));
#25775=CARTESIAN_POINT('Ctrl Pts',(-34.525687510388,14.9076710061311,0.));
#25776=CARTESIAN_POINT('Ctrl Pts',(-34.525687510388,14.9076710061311,18.));
#25777=CARTESIAN_POINT('Ctrl Pts',(-34.5606858566713,14.9222326355678,0.));
#25778=CARTESIAN_POINT('Ctrl Pts',(-34.5606858566713,14.9222326355678,18.));
#25779=CARTESIAN_POINT('Ctrl Pts',(-34.6137007885254,14.9426481276593,0.));
#25780=CARTESIAN_POINT('Ctrl Pts',(-34.6137007885254,14.9426481276593,18.));
#25781=CARTESIAN_POINT('Ctrl Pts',(-34.6853717911268,14.9671565602316,0.));
#25782=CARTESIAN_POINT('Ctrl Pts',(-34.6853717911268,14.9671565602316,18.));
#25783=CARTESIAN_POINT('Ctrl Pts',(-34.7763085406486,14.9940927023322,0.));
#25784=CARTESIAN_POINT('Ctrl Pts',(-34.7763085406486,14.9940927023322,18.));
#25785=CARTESIAN_POINT('Ctrl Pts',(-34.8682205930809,15.0183713484962,0.));
#25786=CARTESIAN_POINT('Ctrl Pts',(-34.8682205930809,15.0183713484962,18.));
#25787=CARTESIAN_POINT('Ctrl Pts',(-34.9607388363587,15.041018569143,0.));
#25788=CARTESIAN_POINT('Ctrl Pts',(-34.9607388363587,15.041018569143,18.));
#25789=CARTESIAN_POINT('Ctrl Pts',(-35.0535882932913,15.0627878528202,0.));
#25790=CARTESIAN_POINT('Ctrl Pts',(-35.0535882932913,15.0627878528202,18.));
#25791=CARTESIAN_POINT('Ctrl Pts',(-35.1466591020976,15.08395927165,0.));
#25792=CARTESIAN_POINT('Ctrl Pts',(-35.1466591020976,15.08395927165,18.));
#25793=CARTESIAN_POINT('Ctrl Pts',(-35.2399506932815,15.104500806927,0.));
#25794=CARTESIAN_POINT('Ctrl Pts',(-35.2399506932815,15.104500806927,18.));
#25795=CARTESIAN_POINT('Ctrl Pts',(-35.3335286891314,15.1241934020682,0.));
#25796=CARTESIAN_POINT('Ctrl Pts',(-35.3335286891314,15.1241934020682,18.));
#25797=CARTESIAN_POINT('Ctrl Pts',(-35.4274792115856,15.1427632633831,0.));
#25798=CARTESIAN_POINT('Ctrl Pts',(-35.4274792115856,15.1427632633831,18.));
#25799=CARTESIAN_POINT('Ctrl Pts',(-35.5218591529746,15.1600260710384,0.));
#25800=CARTESIAN_POINT('Ctrl Pts',(-35.5218591529746,15.1600260710384,18.));
#25801=CARTESIAN_POINT('Ctrl Pts',(-35.6166644736253,15.1759785763051,0.));
#25802=CARTESIAN_POINT('Ctrl Pts',(-35.6166644736253,15.1759785763051,18.));
#25803=CARTESIAN_POINT('Ctrl Pts',(-35.7118553943773,15.1907243629659,0.));
#25804=CARTESIAN_POINT('Ctrl Pts',(-35.7118553943773,15.1907243629659,18.));
#25805=CARTESIAN_POINT('Ctrl Pts',(-35.8073720252878,15.2044274601769,0.));
#25806=CARTESIAN_POINT('Ctrl Pts',(-35.8073720252878,15.2044274601769,18.));
#25807=CARTESIAN_POINT('Ctrl Pts',(-35.9031525499277,15.2172585668056,0.));
#25808=CARTESIAN_POINT('Ctrl Pts',(-35.9031525499277,15.2172585668056,18.));
#25809=CARTESIAN_POINT('Ctrl Pts',(-35.9991531408727,15.2293360946131,0.));
#25810=CARTESIAN_POINT('Ctrl Pts',(-35.9991531408727,15.2293360946131,18.));
#25811=CARTESIAN_POINT('Ctrl Pts',(-36.095357546697,15.240697754828,0.));
#25812=CARTESIAN_POINT('Ctrl Pts',(-36.095357546697,15.240697754828,18.));
#25813=CARTESIAN_POINT('Ctrl Pts',(-36.1917659216814,15.2513334565427,0.));
#25814=CARTESIAN_POINT('Ctrl Pts',(-36.1917659216814,15.2513334565427,18.));
#25815=CARTESIAN_POINT('Ctrl Pts',(-36.2883880151607,15.2612053303773,0.));
#25816=CARTESIAN_POINT('Ctrl Pts',(-36.2883880151607,15.2612053303773,18.));
#25817=CARTESIAN_POINT('Ctrl Pts',(-36.3852352131887,15.2702711460937,0.));
#25818=CARTESIAN_POINT('Ctrl Pts',(-36.3852352131887,15.2702711460937,18.));
#25819=CARTESIAN_POINT('Ctrl Pts',(-36.4823116513289,15.2785104654792,0.));
#25820=CARTESIAN_POINT('Ctrl Pts',(-36.4823116513289,15.2785104654792,18.));
#25821=CARTESIAN_POINT('Ctrl Pts',(-36.5796108931244,15.2859343913094,0.));
#25822=CARTESIAN_POINT('Ctrl Pts',(-36.5796108931244,15.2859343913094,18.));
#25823=CARTESIAN_POINT('Ctrl Pts',(-36.6771206167756,15.2925717100767,0.));
#25824=CARTESIAN_POINT('Ctrl Pts',(-36.6771206167756,15.2925717100767,18.));
#25825=CARTESIAN_POINT('Ctrl Pts',(-36.7748254044502,15.2984606286737,0.));
#25826=CARTESIAN_POINT('Ctrl Pts',(-36.7748254044502,15.2984606286737,18.));
#25827=CARTESIAN_POINT('Ctrl Pts',(-36.8727100302512,15.3036390436952,0.));
#25828=CARTESIAN_POINT('Ctrl Pts',(-36.8727100302512,15.3036390436952,18.));
#25829=CARTESIAN_POINT('Ctrl Pts',(-36.970763176802,15.3081335446406,0.));
#25830=CARTESIAN_POINT('Ctrl Pts',(-36.970763176802,15.3081335446406,18.));
#25831=CARTESIAN_POINT('Ctrl Pts',(-37.0689784837457,15.3119562971444,0.));
#25832=CARTESIAN_POINT('Ctrl Pts',(-37.0689784837457,15.3119562971444,18.));
#25833=CARTESIAN_POINT('Ctrl Pts',(-37.1673525354642,15.3151109648809,0.));
#25834=CARTESIAN_POINT('Ctrl Pts',(-37.1673525354642,15.3151109648809,18.));
#25835=CARTESIAN_POINT('Ctrl Pts',(-37.2658836214694,15.3175963510698,0.));
#25836=CARTESIAN_POINT('Ctrl Pts',(-37.2658836214694,15.3175963510698,18.));
#25837=CARTESIAN_POINT('Ctrl Pts',(-37.3645702997848,15.3194106233801,0.));
#25838=CARTESIAN_POINT('Ctrl Pts',(-37.3645702997848,15.3194106233801,18.));
#25839=CARTESIAN_POINT('Ctrl Pts',(-37.4634097578665,15.3205561366169,0.));
#25840=CARTESIAN_POINT('Ctrl Pts',(-37.4634097578665,15.3205561366169,18.));
#25841=CARTESIAN_POINT('Ctrl Pts',(-37.562397408596,15.3210406145546,0.));
#25842=CARTESIAN_POINT('Ctrl Pts',(-37.562397408596,15.3210406145546,18.));
#25843=CARTESIAN_POINT('Ctrl Pts',(-37.6615277218027,15.3208746890781,0.));
#25844=CARTESIAN_POINT('Ctrl Pts',(-37.6615277218027,15.3208746890781,18.));
#25845=CARTESIAN_POINT('Ctrl Pts',(-37.7607947318286,15.320070396385,0.));
#25846=CARTESIAN_POINT('Ctrl Pts',(-37.7607947318286,15.320070396385,18.));
#25847=CARTESIAN_POINT('Ctrl Pts',(-37.8601926265378,15.3186394335023,0.));
#25848=CARTESIAN_POINT('Ctrl Pts',(-37.8601926265378,15.3186394335023,18.));
#25849=CARTESIAN_POINT('Ctrl Pts',(-37.959716421934,15.3165911656268,0.));
#25850=CARTESIAN_POINT('Ctrl Pts',(-37.959716421934,15.3165911656268,18.));
#25851=CARTESIAN_POINT('Ctrl Pts',(-38.0593621055415,15.3139321941687,0.));
#25852=CARTESIAN_POINT('Ctrl Pts',(-38.0593621055415,15.3139321941687,18.));
#25853=CARTESIAN_POINT('Ctrl Pts',(-38.1591262705847,15.310667421514,0.));
#25854=CARTESIAN_POINT('Ctrl Pts',(-38.1591262705847,15.310667421514,18.));
#25855=CARTESIAN_POINT('Ctrl Pts',(-38.2590058835965,15.3068007250314,0.));
#25856=CARTESIAN_POINT('Ctrl Pts',(-38.2590058835965,15.3068007250314,18.));
#25857=CARTESIAN_POINT('Ctrl Pts',(-38.3589980188324,15.3023357307483,0.));
#25858=CARTESIAN_POINT('Ctrl Pts',(-38.3589980188324,15.3023357307483,18.));
#25859=CARTESIAN_POINT('Ctrl Pts',(-38.4590995527814,15.2972767037469,0.));
#25860=CARTESIAN_POINT('Ctrl Pts',(-38.4590995527814,15.2972767037469,18.));
#25861=CARTESIAN_POINT('Ctrl Pts',(-38.5593070891769,15.2916287700102,0.));
#25862=CARTESIAN_POINT('Ctrl Pts',(-38.5593070891769,15.2916287700102,18.));
#25863=CARTESIAN_POINT('Ctrl Pts',(-38.659617115053,15.2853974668211,0.));
#25864=CARTESIAN_POINT('Ctrl Pts',(-38.659617115053,15.2853974668211,18.));
#25865=CARTESIAN_POINT('Ctrl Pts',(-38.7600260961351,15.2785884727112,0.));
#25866=CARTESIAN_POINT('Ctrl Pts',(-38.7600260961351,15.2785884727112,18.));
#25867=CARTESIAN_POINT('Ctrl Pts',(-38.860530586589,15.2712072937639,0.));
#25868=CARTESIAN_POINT('Ctrl Pts',(-38.860530586589,15.2712072937639,18.));
#25869=CARTESIAN_POINT('Ctrl Pts',(-38.9611273555758,15.2632589109473,0.));
#25870=CARTESIAN_POINT('Ctrl Pts',(-38.9611273555758,15.2632589109473,18.));
#25871=CARTESIAN_POINT('Ctrl Pts',(-39.061813415425,15.2547476855825,0.));
#25872=CARTESIAN_POINT('Ctrl Pts',(-39.061813415425,15.2547476855825,18.));
#25873=CARTESIAN_POINT('Ctrl Pts',(-39.1625859371304,15.2456775636447,0.));
#25874=CARTESIAN_POINT('Ctrl Pts',(-39.1625859371304,15.2456775636447,18.));
#25875=CARTESIAN_POINT('Ctrl Pts',(-39.2634421927888,15.2360522089072,0.));
#25876=CARTESIAN_POINT('Ctrl Pts',(-39.2634421927888,15.2360522089072,18.));
#25877=CARTESIAN_POINT('Ctrl Pts',(-39.3643794927167,15.225875156307,0.));
#25878=CARTESIAN_POINT('Ctrl Pts',(-39.3643794927167,15.225875156307,18.));
#25879=CARTESIAN_POINT('Ctrl Pts',(-39.4653951093947,15.2151499908149,0.));
#25880=CARTESIAN_POINT('Ctrl Pts',(-39.4653951093947,15.2151499908149,18.));
#25881=CARTESIAN_POINT('Ctrl Pts',(-39.5664862602472,15.2038804098649,0.));
#25882=CARTESIAN_POINT('Ctrl Pts',(-39.5664862602472,15.2038804098649,18.));
#25883=CARTESIAN_POINT('Ctrl Pts',(-39.6676501731673,15.1920701163803,0.));
#25884=CARTESIAN_POINT('Ctrl Pts',(-39.6676501731673,15.1920701163803,18.));
#25885=CARTESIAN_POINT('Ctrl Pts',(-39.7688841338802,15.1797227547562,0.));
#25886=CARTESIAN_POINT('Ctrl Pts',(-39.7688841338802,15.1797227547562,18.));
#25887=CARTESIAN_POINT('Ctrl Pts',(-39.8701855339908,15.1668418393198,0.));
#25888=CARTESIAN_POINT('Ctrl Pts',(-39.8701855339908,15.1668418393198,18.));
#25889=CARTESIAN_POINT('Ctrl Pts',(-39.9715519332134,15.1534306754871,0.));
#25890=CARTESIAN_POINT('Ctrl Pts',(-39.9715519332134,15.1534306754871,18.));
#25891=CARTESIAN_POINT('Ctrl Pts',(-40.0729810652204,15.1394923361537,0.));
#25892=CARTESIAN_POINT('Ctrl Pts',(-40.0729810652204,15.1394923361537,18.));
#25893=CARTESIAN_POINT('Ctrl Pts',(-40.1744707357902,15.1250297462408,0.));
#25894=CARTESIAN_POINT('Ctrl Pts',(-40.1744707357902,15.1250297462408,18.));
#25895=CARTESIAN_POINT('Ctrl Pts',(-40.2760187401822,15.1100457495259,0.));
#25896=CARTESIAN_POINT('Ctrl Pts',(-40.2760187401822,15.1100457495259,18.));
#25897=CARTESIAN_POINT('Ctrl Pts',(-40.3776227809037,15.0945431800723,0.));
#25898=CARTESIAN_POINT('Ctrl Pts',(-40.3776227809037,15.0945431800723,18.));
#25899=CARTESIAN_POINT('Ctrl Pts',(-40.4792803645352,15.0785249502524,0.));
#25900=CARTESIAN_POINT('Ctrl Pts',(-40.4792803645352,15.0785249502524,18.));
#25901=CARTESIAN_POINT('Ctrl Pts',(-40.58098877043,15.0619940893017,0.));
#25902=CARTESIAN_POINT('Ctrl Pts',(-40.58098877043,15.0619940893017,18.));
#25903=CARTESIAN_POINT('Ctrl Pts',(-40.6827452453667,15.0449536183143,0.));
#25904=CARTESIAN_POINT('Ctrl Pts',(-40.6827452453667,15.0449536183143,18.));
#25905=CARTESIAN_POINT('Ctrl Pts',(-40.7845471608654,15.0274064563211,0.));
#25906=CARTESIAN_POINT('Ctrl Pts',(-40.7845471608654,15.0274064563211,18.));
#25907=CARTESIAN_POINT('Ctrl Pts',(-40.8863921801,15.0093553188655,0.));
#25908=CARTESIAN_POINT('Ctrl Pts',(-40.8863921801,15.0093553188655,18.));
#25909=CARTESIAN_POINT('Ctrl Pts',(-40.9882784321884,14.9908026205824,0.));
#25910=CARTESIAN_POINT('Ctrl Pts',(-40.9882784321884,14.9908026205824,18.));
#25911=CARTESIAN_POINT('Ctrl Pts',(-41.0902046498729,14.9717503874227,0.));
#25912=CARTESIAN_POINT('Ctrl Pts',(-41.0902046498729,14.9717503874227,18.));
#25913=CARTESIAN_POINT('Ctrl Pts',(-41.1921700381957,14.9522002356298,0.));
#25914=CARTESIAN_POINT('Ctrl Pts',(-41.1921700381957,14.9522002356298,18.));
#25915=CARTESIAN_POINT('Ctrl Pts',(-41.2737733455422,14.936162723752,0.));
#25916=CARTESIAN_POINT('Ctrl Pts',(-41.2737733455422,14.936162723752,18.));
#25917=CARTESIAN_POINT('Ctrl Pts',(-41.3349931861715,14.9239113834707,0.));
#25918=CARTESIAN_POINT('Ctrl Pts',(-41.3349931861715,14.9239113834707,18.));
#25919=CARTESIAN_POINT('Ctrl Pts',(-41.3758141263348,14.9156446533966,0.));
#25920=CARTESIAN_POINT('Ctrl Pts',(-41.3758141263348,14.9156446533966,18.));
#25921=CARTESIAN_POINT('Ctrl Pts',(-41.396226524684,14.911486495888,0.));
#25922=CARTESIAN_POINT('Ctrl Pts',(-41.396226524684,14.911486495888,18.));
#25923=CARTESIAN_POINT('Ctrl Pts',(-34.5082745737944,14.9001523628048,0.));
#25924=CARTESIAN_POINT('Ctrl Pts',(-34.525687510388,14.9076710061311,0.));
#25925=CARTESIAN_POINT('Ctrl Pts',(-34.5606858566713,14.9222326355678,0.));
#25926=CARTESIAN_POINT('Ctrl Pts',(-34.6137007885254,14.9426481276593,0.));
#25927=CARTESIAN_POINT('Ctrl Pts',(-34.6853717911268,14.9671565602316,0.));
#25928=CARTESIAN_POINT('Ctrl Pts',(-34.7763085406486,14.9940927023322,0.));
#25929=CARTESIAN_POINT('Ctrl Pts',(-34.8682205930809,15.0183713484962,0.));
#25930=CARTESIAN_POINT('Ctrl Pts',(-34.9607388363587,15.041018569143,0.));
#25931=CARTESIAN_POINT('Ctrl Pts',(-35.0535882932913,15.0627878528202,0.));
#25932=CARTESIAN_POINT('Ctrl Pts',(-35.1466591020976,15.08395927165,0.));
#25933=CARTESIAN_POINT('Ctrl Pts',(-35.2399506932815,15.104500806927,0.));
#25934=CARTESIAN_POINT('Ctrl Pts',(-35.3335286891314,15.1241934020682,0.));
#25935=CARTESIAN_POINT('Ctrl Pts',(-35.4274792115856,15.1427632633831,0.));
#25936=CARTESIAN_POINT('Ctrl Pts',(-35.5218591529746,15.1600260710384,0.));
#25937=CARTESIAN_POINT('Ctrl Pts',(-35.6166644736253,15.1759785763051,0.));
#25938=CARTESIAN_POINT('Ctrl Pts',(-35.7118553943773,15.1907243629659,0.));
#25939=CARTESIAN_POINT('Ctrl Pts',(-35.8073720252878,15.2044274601769,0.));
#25940=CARTESIAN_POINT('Ctrl Pts',(-35.9031525499277,15.2172585668056,0.));
#25941=CARTESIAN_POINT('Ctrl Pts',(-35.9991531408727,15.2293360946131,0.));
#25942=CARTESIAN_POINT('Ctrl Pts',(-36.095357546697,15.240697754828,0.));
#25943=CARTESIAN_POINT('Ctrl Pts',(-36.1917659216814,15.2513334565427,0.));
#25944=CARTESIAN_POINT('Ctrl Pts',(-36.2883880151607,15.2612053303773,0.));
#25945=CARTESIAN_POINT('Ctrl Pts',(-36.3852352131887,15.2702711460937,0.));
#25946=CARTESIAN_POINT('Ctrl Pts',(-36.4823116513289,15.2785104654792,0.));
#25947=CARTESIAN_POINT('Ctrl Pts',(-36.5796108931244,15.2859343913094,0.));
#25948=CARTESIAN_POINT('Ctrl Pts',(-36.6771206167756,15.2925717100767,0.));
#25949=CARTESIAN_POINT('Ctrl Pts',(-36.7748254044502,15.2984606286737,0.));
#25950=CARTESIAN_POINT('Ctrl Pts',(-36.8727100302512,15.3036390436952,0.));
#25951=CARTESIAN_POINT('Ctrl Pts',(-36.970763176802,15.3081335446406,0.));
#25952=CARTESIAN_POINT('Ctrl Pts',(-37.0689784837457,15.3119562971444,0.));
#25953=CARTESIAN_POINT('Ctrl Pts',(-37.1673525354642,15.3151109648809,0.));
#25954=CARTESIAN_POINT('Ctrl Pts',(-37.2658836214694,15.3175963510698,0.));
#25955=CARTESIAN_POINT('Ctrl Pts',(-37.3645702997848,15.3194106233801,0.));
#25956=CARTESIAN_POINT('Ctrl Pts',(-37.4634097578665,15.3205561366169,0.));
#25957=CARTESIAN_POINT('Ctrl Pts',(-37.562397408596,15.3210406145546,0.));
#25958=CARTESIAN_POINT('Ctrl Pts',(-37.6615277218027,15.3208746890781,0.));
#25959=CARTESIAN_POINT('Ctrl Pts',(-37.7607947318286,15.320070396385,0.));
#25960=CARTESIAN_POINT('Ctrl Pts',(-37.8601926265378,15.3186394335023,0.));
#25961=CARTESIAN_POINT('Ctrl Pts',(-37.959716421934,15.3165911656268,0.));
#25962=CARTESIAN_POINT('Ctrl Pts',(-38.0593621055415,15.3139321941687,0.));
#25963=CARTESIAN_POINT('Ctrl Pts',(-38.1591262705847,15.310667421514,0.));
#25964=CARTESIAN_POINT('Ctrl Pts',(-38.2590058835965,15.3068007250314,0.));
#25965=CARTESIAN_POINT('Ctrl Pts',(-38.3589980188324,15.3023357307483,0.));
#25966=CARTESIAN_POINT('Ctrl Pts',(-38.4590995527814,15.2972767037469,0.));
#25967=CARTESIAN_POINT('Ctrl Pts',(-38.5593070891769,15.2916287700102,0.));
#25968=CARTESIAN_POINT('Ctrl Pts',(-38.659617115053,15.2853974668211,0.));
#25969=CARTESIAN_POINT('Ctrl Pts',(-38.7600260961351,15.2785884727112,0.));
#25970=CARTESIAN_POINT('Ctrl Pts',(-38.860530586589,15.2712072937639,0.));
#25971=CARTESIAN_POINT('Ctrl Pts',(-38.9611273555758,15.2632589109473,0.));
#25972=CARTESIAN_POINT('Ctrl Pts',(-39.061813415425,15.2547476855825,0.));
#25973=CARTESIAN_POINT('Ctrl Pts',(-39.1625859371304,15.2456775636447,0.));
#25974=CARTESIAN_POINT('Ctrl Pts',(-39.2634421927888,15.2360522089072,0.));
#25975=CARTESIAN_POINT('Ctrl Pts',(-39.3643794927167,15.225875156307,0.));
#25976=CARTESIAN_POINT('Ctrl Pts',(-39.4653951093947,15.2151499908149,0.));
#25977=CARTESIAN_POINT('Ctrl Pts',(-39.5664862602472,15.2038804098649,0.));
#25978=CARTESIAN_POINT('Ctrl Pts',(-39.6676501731673,15.1920701163803,0.));
#25979=CARTESIAN_POINT('Ctrl Pts',(-39.7688841338802,15.1797227547562,0.));
#25980=CARTESIAN_POINT('Ctrl Pts',(-39.8701855339908,15.1668418393198,0.));
#25981=CARTESIAN_POINT('Ctrl Pts',(-39.9715519332134,15.1534306754871,0.));
#25982=CARTESIAN_POINT('Ctrl Pts',(-40.0729810652204,15.1394923361537,0.));
#25983=CARTESIAN_POINT('Ctrl Pts',(-40.1744707357902,15.1250297462408,0.));
#25984=CARTESIAN_POINT('Ctrl Pts',(-40.2760187401822,15.1100457495259,0.));
#25985=CARTESIAN_POINT('Ctrl Pts',(-40.3776227809037,15.0945431800723,0.));
#25986=CARTESIAN_POINT('Ctrl Pts',(-40.4792803645352,15.0785249502524,0.));
#25987=CARTESIAN_POINT('Ctrl Pts',(-40.58098877043,15.0619940893017,0.));
#25988=CARTESIAN_POINT('Ctrl Pts',(-40.6827452453667,15.0449536183143,0.));
#25989=CARTESIAN_POINT('Ctrl Pts',(-40.7845471608654,15.0274064563211,0.));
#25990=CARTESIAN_POINT('Ctrl Pts',(-40.8863921801,15.0093553188655,0.));
#25991=CARTESIAN_POINT('Ctrl Pts',(-40.9882784321884,14.9908026205824,0.));
#25992=CARTESIAN_POINT('Ctrl Pts',(-41.1105898934098,14.9679399407908,0.));
#25993=CARTESIAN_POINT('Ctrl Pts',(-41.2125650743922,14.9482653093396,0.));
#25994=CARTESIAN_POINT('Ctrl Pts',(-41.2941761025922,14.9321285285561,0.));
#25995=CARTESIAN_POINT('Ctrl Pts',(-41.3554017279611,14.919802810928,0.));
#25996=CARTESIAN_POINT('Ctrl Pts',(-41.396226524684,14.911486495888,0.));
#25997=CARTESIAN_POINT('Ctrl Pts',(-34.5082745737944,14.9001523628048,15.));
#25998=CARTESIAN_POINT('Ctrl Pts',(-34.525687510388,14.9076710061311,15.));
#25999=CARTESIAN_POINT('Ctrl Pts',(-34.5606858566713,14.9222326355678,15.));
#26000=CARTESIAN_POINT('Ctrl Pts',(-34.6137007885254,14.9426481276593,15.));
#26001=CARTESIAN_POINT('Ctrl Pts',(-34.6853717911268,14.9671565602316,15.));
#26002=CARTESIAN_POINT('Ctrl Pts',(-34.7763085406486,14.9940927023322,15.));
#26003=CARTESIAN_POINT('Ctrl Pts',(-34.8682205930809,15.0183713484962,15.));
#26004=CARTESIAN_POINT('Ctrl Pts',(-34.9607388363587,15.041018569143,15.));
#26005=CARTESIAN_POINT('Ctrl Pts',(-35.0535882932913,15.0627878528202,15.));
#26006=CARTESIAN_POINT('Ctrl Pts',(-35.1466591020976,15.08395927165,15.));
#26007=CARTESIAN_POINT('Ctrl Pts',(-35.2399506932815,15.104500806927,15.));
#26008=CARTESIAN_POINT('Ctrl Pts',(-35.3335286891314,15.1241934020682,15.));
#26009=CARTESIAN_POINT('Ctrl Pts',(-35.4274792115856,15.1427632633831,15.));
#26010=CARTESIAN_POINT('Ctrl Pts',(-35.5218591529746,15.1600260710384,15.));
#26011=CARTESIAN_POINT('Ctrl Pts',(-35.6166644736253,15.1759785763051,15.));
#26012=CARTESIAN_POINT('Ctrl Pts',(-35.7118553943773,15.1907243629659,15.));
#26013=CARTESIAN_POINT('Ctrl Pts',(-35.8073720252878,15.2044274601769,15.));
#26014=CARTESIAN_POINT('Ctrl Pts',(-35.9031525499277,15.2172585668056,15.));
#26015=CARTESIAN_POINT('Ctrl Pts',(-35.9991531408727,15.2293360946131,15.));
#26016=CARTESIAN_POINT('Ctrl Pts',(-36.095357546697,15.240697754828,15.));
#26017=CARTESIAN_POINT('Ctrl Pts',(-36.1917659216814,15.2513334565427,15.));
#26018=CARTESIAN_POINT('Ctrl Pts',(-36.2883880151607,15.2612053303773,15.));
#26019=CARTESIAN_POINT('Ctrl Pts',(-36.3852352131887,15.2702711460937,15.));
#26020=CARTESIAN_POINT('Ctrl Pts',(-36.4823116513289,15.2785104654792,15.));
#26021=CARTESIAN_POINT('Ctrl Pts',(-36.5796108931244,15.2859343913094,15.));
#26022=CARTESIAN_POINT('Ctrl Pts',(-36.6771206167756,15.2925717100767,15.));
#26023=CARTESIAN_POINT('Ctrl Pts',(-36.7748254044502,15.2984606286737,15.));
#26024=CARTESIAN_POINT('Ctrl Pts',(-36.8727100302512,15.3036390436952,15.));
#26025=CARTESIAN_POINT('Ctrl Pts',(-36.970763176802,15.3081335446406,15.));
#26026=CARTESIAN_POINT('Ctrl Pts',(-37.0689784837457,15.3119562971444,15.));
#26027=CARTESIAN_POINT('Ctrl Pts',(-37.1673525354642,15.3151109648809,15.));
#26028=CARTESIAN_POINT('Ctrl Pts',(-37.2658836214694,15.3175963510698,15.));
#26029=CARTESIAN_POINT('Ctrl Pts',(-37.3645702997848,15.3194106233801,15.));
#26030=CARTESIAN_POINT('Ctrl Pts',(-37.4634097578665,15.3205561366169,15.));
#26031=CARTESIAN_POINT('Ctrl Pts',(-37.562397408596,15.3210406145546,15.));
#26032=CARTESIAN_POINT('Ctrl Pts',(-37.6615277218027,15.3208746890781,15.));
#26033=CARTESIAN_POINT('Ctrl Pts',(-37.7607947318286,15.320070396385,15.));
#26034=CARTESIAN_POINT('Ctrl Pts',(-37.8601926265378,15.3186394335023,15.));
#26035=CARTESIAN_POINT('Ctrl Pts',(-37.959716421934,15.3165911656268,15.));
#26036=CARTESIAN_POINT('Ctrl Pts',(-38.0593621055415,15.3139321941687,15.));
#26037=CARTESIAN_POINT('Ctrl Pts',(-38.1591262705847,15.310667421514,15.));
#26038=CARTESIAN_POINT('Ctrl Pts',(-38.2590058835965,15.3068007250314,15.));
#26039=CARTESIAN_POINT('Ctrl Pts',(-38.3589980188324,15.3023357307483,15.));
#26040=CARTESIAN_POINT('Ctrl Pts',(-38.4590995527814,15.2972767037469,15.));
#26041=CARTESIAN_POINT('Ctrl Pts',(-38.5593070891769,15.2916287700102,15.));
#26042=CARTESIAN_POINT('Ctrl Pts',(-38.659617115053,15.2853974668211,15.));
#26043=CARTESIAN_POINT('Ctrl Pts',(-38.7600260961351,15.2785884727112,15.));
#26044=CARTESIAN_POINT('Ctrl Pts',(-38.860530586589,15.2712072937639,15.));
#26045=CARTESIAN_POINT('Ctrl Pts',(-38.9611273555758,15.2632589109473,15.));
#26046=CARTESIAN_POINT('Ctrl Pts',(-39.061813415425,15.2547476855825,15.));
#26047=CARTESIAN_POINT('Ctrl Pts',(-39.1625859371304,15.2456775636447,15.));
#26048=CARTESIAN_POINT('Ctrl Pts',(-39.2634421927888,15.2360522089072,15.));
#26049=CARTESIAN_POINT('Ctrl Pts',(-39.3643794927167,15.225875156307,15.));
#26050=CARTESIAN_POINT('Ctrl Pts',(-39.4653951093947,15.2151499908149,15.));
#26051=CARTESIAN_POINT('Ctrl Pts',(-39.5664862602472,15.2038804098649,15.));
#26052=CARTESIAN_POINT('Ctrl Pts',(-39.6676501731673,15.1920701163803,15.));
#26053=CARTESIAN_POINT('Ctrl Pts',(-39.7688841338802,15.1797227547562,15.));
#26054=CARTESIAN_POINT('Ctrl Pts',(-39.8701855339908,15.1668418393198,15.));
#26055=CARTESIAN_POINT('Ctrl Pts',(-39.9715519332134,15.1534306754871,15.));
#26056=CARTESIAN_POINT('Ctrl Pts',(-40.0729810652204,15.1394923361537,15.));
#26057=CARTESIAN_POINT('Ctrl Pts',(-40.1744707357902,15.1250297462408,15.));
#26058=CARTESIAN_POINT('Ctrl Pts',(-40.2760187401822,15.1100457495259,15.));
#26059=CARTESIAN_POINT('Ctrl Pts',(-40.3776227809037,15.0945431800723,15.));
#26060=CARTESIAN_POINT('Ctrl Pts',(-40.4792803645352,15.0785249502524,15.));
#26061=CARTESIAN_POINT('Ctrl Pts',(-40.58098877043,15.0619940893017,15.));
#26062=CARTESIAN_POINT('Ctrl Pts',(-40.6827452453667,15.0449536183143,15.));
#26063=CARTESIAN_POINT('Ctrl Pts',(-40.7845471608654,15.0274064563211,15.));
#26064=CARTESIAN_POINT('Ctrl Pts',(-40.8863921801,15.0093553188655,15.));
#26065=CARTESIAN_POINT('Ctrl Pts',(-40.9882784321884,14.9908026205824,15.));
#26066=CARTESIAN_POINT('Ctrl Pts',(-41.1105898934098,14.9679399407908,15.));
#26067=CARTESIAN_POINT('Ctrl Pts',(-41.2125650743922,14.9482653093396,15.));
#26068=CARTESIAN_POINT('Ctrl Pts',(-41.2941761025922,14.9321285285561,15.));
#26069=CARTESIAN_POINT('Ctrl Pts',(-41.3554017279611,14.919802810928,15.));
#26070=CARTESIAN_POINT('Ctrl Pts',(-41.396226524684,14.911486495888,15.));
#26071=CARTESIAN_POINT('Ctrl Pts',(-36.3957374383337,24.725498909423,0.));
#26072=CARTESIAN_POINT('Ctrl Pts',(-36.3957374383337,24.725498909423,18.));
#26073=CARTESIAN_POINT('Ctrl Pts',(-36.3871033517098,24.7065408286023,0.));
#26074=CARTESIAN_POINT('Ctrl Pts',(-36.3871033517098,24.7065408286023,18.));
#26075=CARTESIAN_POINT('Ctrl Pts',(-36.369797330215,24.6686569322616,0.));
#26076=CARTESIAN_POINT('Ctrl Pts',(-36.369797330215,24.6686569322616,18.));
#26077=CARTESIAN_POINT('Ctrl Pts',(-36.3437247532368,24.6119278836614,0.));
#26078=CARTESIAN_POINT('Ctrl Pts',(-36.3437247532368,24.6119278836614,18.));
#26079=CARTESIAN_POINT('Ctrl Pts',(-36.3087341522969,24.5364828082556,0.));
#26080=CARTESIAN_POINT('Ctrl Pts',(-36.3087341522969,24.5364828082556,18.));
#26081=CARTESIAN_POINT('Ctrl Pts',(-36.2646168058395,24.4424997853605,0.));
#26082=CARTESIAN_POINT('Ctrl Pts',(-36.2646168058395,24.4424997853605,18.));
#26083=CARTESIAN_POINT('Ctrl Pts',(-36.2201196586696,24.3488411214068,0.));
#26084=CARTESIAN_POINT('Ctrl Pts',(-36.2201196586696,24.3488411214068,18.));
#26085=CARTESIAN_POINT('Ctrl Pts',(-36.1752418704833,24.2555084095332,0.));
#26086=CARTESIAN_POINT('Ctrl Pts',(-36.1752418704833,24.2555084095332,18.));
#26087=CARTESIAN_POINT('Ctrl Pts',(-36.1299825471271,24.1625038657964,0.));
#26088=CARTESIAN_POINT('Ctrl Pts',(-36.1299825471271,24.1625038657964,18.));
#26089=CARTESIAN_POINT('Ctrl Pts',(-36.0843408347974,24.0698304230588,0.));
#26090=CARTESIAN_POINT('Ctrl Pts',(-36.0843408347974,24.0698304230588,18.));
#26091=CARTESIAN_POINT('Ctrl Pts',(-36.0383159101253,23.9774915680089,0.));
#26092=CARTESIAN_POINT('Ctrl Pts',(-36.0383159101253,23.9774915680089,18.));
#26093=CARTESIAN_POINT('Ctrl Pts',(-35.9919069565469,23.8854911428946,0.));
#26094=CARTESIAN_POINT('Ctrl Pts',(-35.9919069565469,23.8854911428946,18.));
#26095=CARTESIAN_POINT('Ctrl Pts',(-35.9451131482488,23.7938331508737,0.));
#26096=CARTESIAN_POINT('Ctrl Pts',(-35.9451131482488,23.7938331508737,18.));
#26097=CARTESIAN_POINT('Ctrl Pts',(-35.8979336336837,23.7025215735353,0.));
#26098=CARTESIAN_POINT('Ctrl Pts',(-35.8979336336837,23.7025215735353,18.));
#26099=CARTESIAN_POINT('Ctrl Pts',(-35.8503675222885,23.611560139948,0.));
#26100=CARTESIAN_POINT('Ctrl Pts',(-35.8503675222885,23.611560139948,18.));
#26101=CARTESIAN_POINT('Ctrl Pts',(-35.8024138716896,23.5209523746427,0.));
#26102=CARTESIAN_POINT('Ctrl Pts',(-35.8024138716896,23.5209523746427,18.));
#26103=CARTESIAN_POINT('Ctrl Pts',(-35.7540716771372,23.4307017328227,0.));
#26104=CARTESIAN_POINT('Ctrl Pts',(-35.7540716771372,23.4307017328227,18.));
#26105=CARTESIAN_POINT('Ctrl Pts',(-35.7053398620512,23.3408117088762,0.));
#26106=CARTESIAN_POINT('Ctrl Pts',(-35.7053398620512,23.3408117088762,18.));
#26107=CARTESIAN_POINT('Ctrl Pts',(-35.6562172725207,23.2512859425032,0.));
#26108=CARTESIAN_POINT('Ctrl Pts',(-35.6562172725207,23.2512859425032,18.));
#26109=CARTESIAN_POINT('Ctrl Pts',(-35.6067026687722,23.1621283508111,0.));
#26110=CARTESIAN_POINT('Ctrl Pts',(-35.6067026687722,23.1621283508111,18.));
#26111=CARTESIAN_POINT('Ctrl Pts',(-35.5567947408311,23.0733431097058,0.));
#26112=CARTESIAN_POINT('Ctrl Pts',(-35.5567947408311,23.0733431097058,18.));
#26113=CARTESIAN_POINT('Ctrl Pts',(-35.5064921357308,22.9849345572033,0.));
#26114=CARTESIAN_POINT('Ctrl Pts',(-35.5064921357308,22.9849345572033,18.));
#26115=CARTESIAN_POINT('Ctrl Pts',(-35.4557934871468,22.8969071125089,0.));
#26116=CARTESIAN_POINT('Ctrl Pts',(-35.4557934871468,22.8969071125089,18.));
#26117=CARTESIAN_POINT('Ctrl Pts',(-35.4046974393492,22.8092652000706,0.));
#26118=CARTESIAN_POINT('Ctrl Pts',(-35.4046974393492,22.8092652000706,18.));
#26119=CARTESIAN_POINT('Ctrl Pts',(-35.3532026952313,22.7220131336912,0.));
#26120=CARTESIAN_POINT('Ctrl Pts',(-35.3532026952313,22.7220131336912,18.));
#26121=CARTESIAN_POINT('Ctrl Pts',(-35.3013079759252,22.635155167154,0.));
#26122=CARTESIAN_POINT('Ctrl Pts',(-35.3013079759252,22.635155167154,18.));
#26123=CARTESIAN_POINT('Ctrl Pts',(-35.2490119207975,22.5486956608909,0.));
#26124=CARTESIAN_POINT('Ctrl Pts',(-35.2490119207975,22.5486956608909,18.));
#26125=CARTESIAN_POINT('Ctrl Pts',(-35.1963130003352,22.4626392230023,0.));
#26126=CARTESIAN_POINT('Ctrl Pts',(-35.1963130003352,22.4626392230023,18.));
#26127=CARTESIAN_POINT('Ctrl Pts',(-35.1432094422642,22.3769908340843,0.));
#26128=CARTESIAN_POINT('Ctrl Pts',(-35.1432094422642,22.3769908340843,18.));
#26129=CARTESIAN_POINT('Ctrl Pts',(-35.0896991159359,22.2917560356803,0.));
#26130=CARTESIAN_POINT('Ctrl Pts',(-35.0896991159359,22.2917560356803,18.));
#26131=CARTESIAN_POINT('Ctrl Pts',(-35.0357795922459,22.2069408519233,0.));
#26132=CARTESIAN_POINT('Ctrl Pts',(-35.0357795922459,22.2069408519233,18.));
#26133=CARTESIAN_POINT('Ctrl Pts',(-34.9814483545602,22.1225514798584,0.));
#26134=CARTESIAN_POINT('Ctrl Pts',(-34.9814483545602,22.1225514798584,18.));
#26135=CARTESIAN_POINT('Ctrl Pts',(-34.9267029879922,22.0385940162683,0.));
#26136=CARTESIAN_POINT('Ctrl Pts',(-34.9267029879922,22.0385940162683,18.));
#26137=CARTESIAN_POINT('Ctrl Pts',(-34.8715413418101,21.9550742217675,0.));
#26138=CARTESIAN_POINT('Ctrl Pts',(-34.8715413418101,21.9550742217675,18.));
#26139=CARTESIAN_POINT('Ctrl Pts',(-34.8159618014436,21.8719971302817,0.));
#26140=CARTESIAN_POINT('Ctrl Pts',(-34.8159618014436,21.8719971302817,18.));
#26141=CARTESIAN_POINT('Ctrl Pts',(-34.7599631530844,21.7893672401137,0.));
#26142=CARTESIAN_POINT('Ctrl Pts',(-34.7599631530844,21.7893672401137,18.));
#26143=CARTESIAN_POINT('Ctrl Pts',(-34.7035440429025,21.7071892844497,0.));
#26144=CARTESIAN_POINT('Ctrl Pts',(-34.7035440429025,21.7071892844497,18.));
#26145=CARTESIAN_POINT('Ctrl Pts',(-34.6467025072367,21.6254689009796,0.));
#26146=CARTESIAN_POINT('Ctrl Pts',(-34.6467025072367,21.6254689009796,18.));
#26147=CARTESIAN_POINT('Ctrl Pts',(-34.5894355639081,21.5442132160757,0.));
#26148=CARTESIAN_POINT('Ctrl Pts',(-34.5894355639081,21.5442132160757,18.));
#26149=CARTESIAN_POINT('Ctrl Pts',(-34.5317385658329,21.4634317666005,0.));
#26150=CARTESIAN_POINT('Ctrl Pts',(-34.5317385658329,21.4634317666005,18.));
#26151=CARTESIAN_POINT('Ctrl Pts',(-34.4736054662052,21.3831361300104,0.));
#26152=CARTESIAN_POINT('Ctrl Pts',(-34.4736054662052,21.3831361300104,18.));
#26153=CARTESIAN_POINT('Ctrl Pts',(-34.4150300340623,21.3033382073239,0.));
#26154=CARTESIAN_POINT('Ctrl Pts',(-34.4150300340623,21.3033382073239,18.));
#26155=CARTESIAN_POINT('Ctrl Pts',(-34.3560069185815,21.2240487218079,0.));
#26156=CARTESIAN_POINT('Ctrl Pts',(-34.3560069185815,21.2240487218079,18.));
#26157=CARTESIAN_POINT('Ctrl Pts',(-34.2965325673384,21.1452759244399,0.));
#26158=CARTESIAN_POINT('Ctrl Pts',(-34.2965325673384,21.1452759244399,18.));
#26159=CARTESIAN_POINT('Ctrl Pts',(-34.2366067284279,21.0670234747355,0.));
#26160=CARTESIAN_POINT('Ctrl Pts',(-34.2366067284279,21.0670234747355,18.));
#26161=CARTESIAN_POINT('Ctrl Pts',(-34.176231731809,20.9892914622612,0.));
#26162=CARTESIAN_POINT('Ctrl Pts',(-34.176231731809,20.9892914622612,18.));
#26163=CARTESIAN_POINT('Ctrl Pts',(-34.1154095510973,20.9120805673809,0.));
#26164=CARTESIAN_POINT('Ctrl Pts',(-34.1154095510973,20.9120805673809,18.));
#26165=CARTESIAN_POINT('Ctrl Pts',(-34.0541392299678,20.8353957068415,0.));
#26166=CARTESIAN_POINT('Ctrl Pts',(-34.0541392299678,20.8353957068415,18.));
#26167=CARTESIAN_POINT('Ctrl Pts',(-33.9924146647395,20.7592491770603,0.));
#26168=CARTESIAN_POINT('Ctrl Pts',(-33.9924146647395,20.7592491770603,18.));
#26169=CARTESIAN_POINT('Ctrl Pts',(-33.9302209962425,20.683665762903,0.));
#26170=CARTESIAN_POINT('Ctrl Pts',(-33.9302209962425,20.683665762903,18.));
#26171=CARTESIAN_POINT('Ctrl Pts',(-33.8675365150454,20.6086800574386,0.));
#26172=CARTESIAN_POINT('Ctrl Pts',(-33.8675365150454,20.6086800574386,18.));
#26173=CARTESIAN_POINT('Ctrl Pts',(-33.8043393734971,20.5343269914034,0.));
#26174=CARTESIAN_POINT('Ctrl Pts',(-33.8043393734971,20.5343269914034,18.));
#26175=CARTESIAN_POINT('Ctrl Pts',(-33.7406135254082,20.4606334536183,0.));
#26176=CARTESIAN_POINT('Ctrl Pts',(-33.7406135254082,20.4606334536183,18.));
#26177=CARTESIAN_POINT('Ctrl Pts',(-33.6763537716992,20.3876111773341,0.));
#26178=CARTESIAN_POINT('Ctrl Pts',(-33.6763537716992,20.3876111773341,18.));
#26179=CARTESIAN_POINT('Ctrl Pts',(-33.6115742164079,20.3152448035298,0.));
#26180=CARTESIAN_POINT('Ctrl Pts',(-33.6115742164079,20.3152448035298,18.));
#26181=CARTESIAN_POINT('Ctrl Pts',(-33.5463023319603,20.243500298383,0.));
#26182=CARTESIAN_POINT('Ctrl Pts',(-33.5463023319603,20.243500298383,18.));
#26183=CARTESIAN_POINT('Ctrl Pts',(-33.480563024813,20.1723475154533,0.));
#26184=CARTESIAN_POINT('Ctrl Pts',(-33.480563024813,20.1723475154533,18.));
#26185=CARTESIAN_POINT('Ctrl Pts',(-33.4143643679979,20.1017803986381,0.));
#26186=CARTESIAN_POINT('Ctrl Pts',(-33.4143643679979,20.1017803986381,18.));
#26187=CARTESIAN_POINT('Ctrl Pts',(-33.3476854048385,20.0318342617213,0.));
#26188=CARTESIAN_POINT('Ctrl Pts',(-33.3476854048385,20.0318342617213,18.));
#26189=CARTESIAN_POINT('Ctrl Pts',(-33.2804560993213,19.9626141625205,0.));
#26190=CARTESIAN_POINT('Ctrl Pts',(-33.2804560993213,19.9626141625205,18.));
#26191=CARTESIAN_POINT('Ctrl Pts',(-33.2125746879471,19.8942704458546,0.));
#26192=CARTESIAN_POINT('Ctrl Pts',(-33.2125746879471,19.8942704458546,18.));
#26193=CARTESIAN_POINT('Ctrl Pts',(-33.1439436707661,19.8269479776239,0.));
#26194=CARTESIAN_POINT('Ctrl Pts',(-33.1439436707661,19.8269479776239,18.));
#26195=CARTESIAN_POINT('Ctrl Pts',(-33.0745026283418,19.7607398248651,0.));
#26196=CARTESIAN_POINT('Ctrl Pts',(-33.0745026283418,19.7607398248651,18.));
#26197=CARTESIAN_POINT('Ctrl Pts',(-33.004256563411,19.6956473461873,0.));
#26198=CARTESIAN_POINT('Ctrl Pts',(-33.004256563411,19.6956473461873,18.));
#26199=CARTESIAN_POINT('Ctrl Pts',(-32.9333211533788,19.6315161742485,0.));
#26200=CARTESIAN_POINT('Ctrl Pts',(-32.9333211533788,19.6315161742485,18.));
#26201=CARTESIAN_POINT('Ctrl Pts',(-32.8618672807884,19.5681157030437,0.));
#26202=CARTESIAN_POINT('Ctrl Pts',(-32.8618672807884,19.5681157030437,18.));
#26203=CARTESIAN_POINT('Ctrl Pts',(-32.7900335943248,19.5052640847974,0.));
#26204=CARTESIAN_POINT('Ctrl Pts',(-32.7900335943248,19.5052640847974,18.));
#26205=CARTESIAN_POINT('Ctrl Pts',(-32.7178463324062,19.4429429601189,0.));
#26206=CARTESIAN_POINT('Ctrl Pts',(-32.7178463324062,19.4429429601189,18.));
#26207=CARTESIAN_POINT('Ctrl Pts',(-32.6451434870609,19.381405831319,0.));
#26208=CARTESIAN_POINT('Ctrl Pts',(-32.6451434870609,19.381405831319,18.));
#26209=CARTESIAN_POINT('Ctrl Pts',(-32.5714771007861,19.3213180490743,0.));
#26210=CARTESIAN_POINT('Ctrl Pts',(-32.5714771007861,19.3213180490743,18.));
#26211=CARTESIAN_POINT('Ctrl Pts',(-32.4962340238036,19.2635813403783,0.));
#26212=CARTESIAN_POINT('Ctrl Pts',(-32.4962340238036,19.2635813403783,18.));
#26213=CARTESIAN_POINT('Ctrl Pts',(-32.4342791270009,19.2200039764927,0.));
#26214=CARTESIAN_POINT('Ctrl Pts',(-32.4342791270009,19.2200039764927,18.));
#26215=CARTESIAN_POINT('Ctrl Pts',(-32.3866012518553,19.1891139208368,0.));
#26216=CARTESIAN_POINT('Ctrl Pts',(-32.3866012518553,19.1891139208368,18.));
#26217=CARTESIAN_POINT('Ctrl Pts',(-32.3542491343753,19.1693587749508,0.));
#26218=CARTESIAN_POINT('Ctrl Pts',(-32.3542491343753,19.1693587749508,18.));
#26219=CARTESIAN_POINT('Ctrl Pts',(-32.3379313568208,19.1596907609891,0.));
#26220=CARTESIAN_POINT('Ctrl Pts',(-32.3379313568208,19.1596907609891,18.));
#26221=CARTESIAN_POINT('',(-36.3957374383337,24.7254989094229,0.));
#26222=CARTESIAN_POINT('Ctrl Pts',(-32.3379313568208,19.1596907609891,0.));
#26223=CARTESIAN_POINT('Ctrl Pts',(-32.3542491343753,19.1693587749508,0.));
#26224=CARTESIAN_POINT('Ctrl Pts',(-32.3866012518553,19.1891139208368,0.));
#26225=CARTESIAN_POINT('Ctrl Pts',(-32.4342791270009,19.2200039764927,0.));
#26226=CARTESIAN_POINT('Ctrl Pts',(-32.4962340238036,19.2635813403783,0.));
#26227=CARTESIAN_POINT('Ctrl Pts',(-32.5714771007861,19.3213180490743,0.));
#26228=CARTESIAN_POINT('Ctrl Pts',(-32.6451434870609,19.381405831319,0.));
#26229=CARTESIAN_POINT('Ctrl Pts',(-32.7178463324062,19.4429429601189,0.));
#26230=CARTESIAN_POINT('Ctrl Pts',(-32.7900335943248,19.5052640847974,0.));
#26231=CARTESIAN_POINT('Ctrl Pts',(-32.8618672807884,19.5681157030437,0.));
#26232=CARTESIAN_POINT('Ctrl Pts',(-32.9333211533788,19.6315161742485,0.));
#26233=CARTESIAN_POINT('Ctrl Pts',(-33.004256563411,19.6956473461873,0.));
#26234=CARTESIAN_POINT('Ctrl Pts',(-33.0745026283418,19.7607398248651,0.));
#26235=CARTESIAN_POINT('Ctrl Pts',(-33.1439436707661,19.8269479776239,0.));
#26236=CARTESIAN_POINT('Ctrl Pts',(-33.2125746879471,19.8942704458546,0.));
#26237=CARTESIAN_POINT('Ctrl Pts',(-33.2804560993213,19.9626141625205,0.));
#26238=CARTESIAN_POINT('Ctrl Pts',(-33.3476854048385,20.0318342617213,0.));
#26239=CARTESIAN_POINT('Ctrl Pts',(-33.4143643679979,20.1017803986381,0.));
#26240=CARTESIAN_POINT('Ctrl Pts',(-33.480563024813,20.1723475154533,0.));
#26241=CARTESIAN_POINT('Ctrl Pts',(-33.5463023319603,20.243500298383,0.));
#26242=CARTESIAN_POINT('Ctrl Pts',(-33.6115742164079,20.3152448035298,0.));
#26243=CARTESIAN_POINT('Ctrl Pts',(-33.6763537716992,20.3876111773341,0.));
#26244=CARTESIAN_POINT('Ctrl Pts',(-33.7406135254082,20.4606334536183,0.));
#26245=CARTESIAN_POINT('Ctrl Pts',(-33.8043393734971,20.5343269914034,0.));
#26246=CARTESIAN_POINT('Ctrl Pts',(-33.8675365150454,20.6086800574386,0.));
#26247=CARTESIAN_POINT('Ctrl Pts',(-33.9302209962425,20.683665762903,0.));
#26248=CARTESIAN_POINT('Ctrl Pts',(-33.9924146647395,20.7592491770603,0.));
#26249=CARTESIAN_POINT('Ctrl Pts',(-34.0541392299678,20.8353957068415,0.));
#26250=CARTESIAN_POINT('Ctrl Pts',(-34.1154095510973,20.9120805673809,0.));
#26251=CARTESIAN_POINT('Ctrl Pts',(-34.176231731809,20.9892914622612,0.));
#26252=CARTESIAN_POINT('Ctrl Pts',(-34.2366067284279,21.0670234747355,0.));
#26253=CARTESIAN_POINT('Ctrl Pts',(-34.2965325673384,21.1452759244399,0.));
#26254=CARTESIAN_POINT('Ctrl Pts',(-34.3560069185815,21.2240487218079,0.));
#26255=CARTESIAN_POINT('Ctrl Pts',(-34.4150300340623,21.3033382073239,0.));
#26256=CARTESIAN_POINT('Ctrl Pts',(-34.4736054662052,21.3831361300104,0.));
#26257=CARTESIAN_POINT('Ctrl Pts',(-34.5317385658329,21.4634317666005,0.));
#26258=CARTESIAN_POINT('Ctrl Pts',(-34.5894355639081,21.5442132160757,0.));
#26259=CARTESIAN_POINT('Ctrl Pts',(-34.6467025072367,21.6254689009796,0.));
#26260=CARTESIAN_POINT('Ctrl Pts',(-34.7035440429025,21.7071892844497,0.));
#26261=CARTESIAN_POINT('Ctrl Pts',(-34.7599631530844,21.7893672401137,0.));
#26262=CARTESIAN_POINT('Ctrl Pts',(-34.8159618014436,21.8719971302817,0.));
#26263=CARTESIAN_POINT('Ctrl Pts',(-34.8715413418101,21.9550742217675,0.));
#26264=CARTESIAN_POINT('Ctrl Pts',(-34.9267029879922,22.0385940162683,0.));
#26265=CARTESIAN_POINT('Ctrl Pts',(-34.9814483545602,22.1225514798584,0.));
#26266=CARTESIAN_POINT('Ctrl Pts',(-35.0357795922459,22.2069408519233,0.));
#26267=CARTESIAN_POINT('Ctrl Pts',(-35.0896991159359,22.2917560356803,0.));
#26268=CARTESIAN_POINT('Ctrl Pts',(-35.1432094422642,22.3769908340843,0.));
#26269=CARTESIAN_POINT('Ctrl Pts',(-35.1963130003352,22.4626392230023,0.));
#26270=CARTESIAN_POINT('Ctrl Pts',(-35.2490119207975,22.5486956608909,0.));
#26271=CARTESIAN_POINT('Ctrl Pts',(-35.3013079759252,22.635155167154,0.));
#26272=CARTESIAN_POINT('Ctrl Pts',(-35.3532026952313,22.7220131336912,0.));
#26273=CARTESIAN_POINT('Ctrl Pts',(-35.4046974393492,22.8092652000706,0.));
#26274=CARTESIAN_POINT('Ctrl Pts',(-35.4557934871468,22.8969071125089,0.));
#26275=CARTESIAN_POINT('Ctrl Pts',(-35.5064921357308,22.9849345572033,0.));
#26276=CARTESIAN_POINT('Ctrl Pts',(-35.5567947408311,23.0733431097058,0.));
#26277=CARTESIAN_POINT('Ctrl Pts',(-35.6067026687722,23.1621283508111,0.));
#26278=CARTESIAN_POINT('Ctrl Pts',(-35.6562172725207,23.2512859425032,0.));
#26279=CARTESIAN_POINT('Ctrl Pts',(-35.7053398620512,23.3408117088762,0.));
#26280=CARTESIAN_POINT('Ctrl Pts',(-35.7540716771372,23.4307017328227,0.));
#26281=CARTESIAN_POINT('Ctrl Pts',(-35.8024138716896,23.5209523746427,0.));
#26282=CARTESIAN_POINT('Ctrl Pts',(-35.8503675222885,23.611560139948,0.));
#26283=CARTESIAN_POINT('Ctrl Pts',(-35.8979336336837,23.7025215735353,0.));
#26284=CARTESIAN_POINT('Ctrl Pts',(-35.9451131482488,23.7938331508737,0.));
#26285=CARTESIAN_POINT('Ctrl Pts',(-35.9919069565469,23.8854911428946,0.));
#26286=CARTESIAN_POINT('Ctrl Pts',(-36.0383159101253,23.9774915680089,0.));
#26287=CARTESIAN_POINT('Ctrl Pts',(-36.0843408347974,24.0698304230588,0.));
#26288=CARTESIAN_POINT('Ctrl Pts',(-36.1299825471271,24.1625038657964,0.));
#26289=CARTESIAN_POINT('Ctrl Pts',(-36.1752418704833,24.2555084095332,0.));
#26290=CARTESIAN_POINT('Ctrl Pts',(-36.2201196586696,24.3488411214068,0.));
#26291=CARTESIAN_POINT('Ctrl Pts',(-36.2735162352735,24.4612315181512,0.));
#26292=CARTESIAN_POINT('Ctrl Pts',(-36.3175386315528,24.5552956307817,0.));
#26293=CARTESIAN_POINT('Ctrl Pts',(-36.3524534604648,24.630805301288,0.));
#26294=CARTESIAN_POINT('Ctrl Pts',(-36.3784692650901,24.6875827477484,0.));
#26295=CARTESIAN_POINT('Ctrl Pts',(-36.3957374383337,24.725498909423,0.));
#26296=CARTESIAN_POINT('',(-36.3957374383337,24.7254989094229,15.));
#26297=CARTESIAN_POINT('Ctrl Pts',(-36.3957374383337,24.725498909423,15.));
#26298=CARTESIAN_POINT('Ctrl Pts',(-36.3871033517098,24.7065408286023,15.));
#26299=CARTESIAN_POINT('Ctrl Pts',(-36.369797330215,24.6686569322616,15.));
#26300=CARTESIAN_POINT('Ctrl Pts',(-36.3437247532368,24.6119278836614,15.));
#26301=CARTESIAN_POINT('Ctrl Pts',(-36.3087341522969,24.5364828082556,15.));
#26302=CARTESIAN_POINT('Ctrl Pts',(-36.2646168058395,24.4424997853605,15.));
#26303=CARTESIAN_POINT('Ctrl Pts',(-36.2201196586696,24.3488411214068,15.));
#26304=CARTESIAN_POINT('Ctrl Pts',(-36.1752418704833,24.2555084095332,15.));
#26305=CARTESIAN_POINT('Ctrl Pts',(-36.1299825471271,24.1625038657964,15.));
#26306=CARTESIAN_POINT('Ctrl Pts',(-36.0843408347974,24.0698304230588,15.));
#26307=CARTESIAN_POINT('Ctrl Pts',(-36.0383159101253,23.9774915680089,15.));
#26308=CARTESIAN_POINT('Ctrl Pts',(-35.9919069565469,23.8854911428946,15.));
#26309=CARTESIAN_POINT('Ctrl Pts',(-35.9451131482488,23.7938331508737,15.));
#26310=CARTESIAN_POINT('Ctrl Pts',(-35.8979336336837,23.7025215735353,15.));
#26311=CARTESIAN_POINT('Ctrl Pts',(-35.8503675222885,23.611560139948,15.));
#26312=CARTESIAN_POINT('Ctrl Pts',(-35.8024138716896,23.5209523746427,15.));
#26313=CARTESIAN_POINT('Ctrl Pts',(-35.7540716771372,23.4307017328227,15.));
#26314=CARTESIAN_POINT('Ctrl Pts',(-35.7053398620512,23.3408117088762,15.));
#26315=CARTESIAN_POINT('Ctrl Pts',(-35.6562172725207,23.2512859425032,15.));
#26316=CARTESIAN_POINT('Ctrl Pts',(-35.6067026687722,23.1621283508111,15.));
#26317=CARTESIAN_POINT('Ctrl Pts',(-35.5567947408311,23.0733431097058,15.));
#26318=CARTESIAN_POINT('Ctrl Pts',(-35.5064921357308,22.9849345572033,15.));
#26319=CARTESIAN_POINT('Ctrl Pts',(-35.4557934871468,22.8969071125089,15.));
#26320=CARTESIAN_POINT('Ctrl Pts',(-35.4046974393492,22.8092652000706,15.));
#26321=CARTESIAN_POINT('Ctrl Pts',(-35.3532026952313,22.7220131336912,15.));
#26322=CARTESIAN_POINT('Ctrl Pts',(-35.3013079759252,22.635155167154,15.));
#26323=CARTESIAN_POINT('Ctrl Pts',(-35.2490119207975,22.5486956608909,15.));
#26324=CARTESIAN_POINT('Ctrl Pts',(-35.1963130003352,22.4626392230023,15.));
#26325=CARTESIAN_POINT('Ctrl Pts',(-35.1432094422642,22.3769908340843,15.));
#26326=CARTESIAN_POINT('Ctrl Pts',(-35.0896991159359,22.2917560356803,15.));
#26327=CARTESIAN_POINT('Ctrl Pts',(-35.0357795922459,22.2069408519233,15.));
#26328=CARTESIAN_POINT('Ctrl Pts',(-34.9814483545602,22.1225514798584,15.));
#26329=CARTESIAN_POINT('Ctrl Pts',(-34.9267029879922,22.0385940162683,15.));
#26330=CARTESIAN_POINT('Ctrl Pts',(-34.8715413418101,21.9550742217675,15.));
#26331=CARTESIAN_POINT('Ctrl Pts',(-34.8159618014436,21.8719971302817,15.));
#26332=CARTESIAN_POINT('Ctrl Pts',(-34.7599631530844,21.7893672401137,15.));
#26333=CARTESIAN_POINT('Ctrl Pts',(-34.7035440429025,21.7071892844497,15.));
#26334=CARTESIAN_POINT('Ctrl Pts',(-34.6467025072367,21.6254689009796,15.));
#26335=CARTESIAN_POINT('Ctrl Pts',(-34.5894355639081,21.5442132160757,15.));
#26336=CARTESIAN_POINT('Ctrl Pts',(-34.5317385658329,21.4634317666005,15.));
#26337=CARTESIAN_POINT('Ctrl Pts',(-34.4736054662052,21.3831361300104,15.));
#26338=CARTESIAN_POINT('Ctrl Pts',(-34.4150300340623,21.3033382073239,15.));
#26339=CARTESIAN_POINT('Ctrl Pts',(-34.3560069185815,21.2240487218079,15.));
#26340=CARTESIAN_POINT('Ctrl Pts',(-34.2965325673384,21.1452759244399,15.));
#26341=CARTESIAN_POINT('Ctrl Pts',(-34.2366067284279,21.0670234747355,15.));
#26342=CARTESIAN_POINT('Ctrl Pts',(-34.176231731809,20.9892914622612,15.));
#26343=CARTESIAN_POINT('Ctrl Pts',(-34.1154095510973,20.9120805673809,15.));
#26344=CARTESIAN_POINT('Ctrl Pts',(-34.0541392299678,20.8353957068415,15.));
#26345=CARTESIAN_POINT('Ctrl Pts',(-33.9924146647395,20.7592491770603,15.));
#26346=CARTESIAN_POINT('Ctrl Pts',(-33.9302209962425,20.683665762903,15.));
#26347=CARTESIAN_POINT('Ctrl Pts',(-33.8675365150454,20.6086800574386,15.));
#26348=CARTESIAN_POINT('Ctrl Pts',(-33.8043393734971,20.5343269914034,15.));
#26349=CARTESIAN_POINT('Ctrl Pts',(-33.7406135254082,20.4606334536183,15.));
#26350=CARTESIAN_POINT('Ctrl Pts',(-33.6763537716992,20.3876111773341,15.));
#26351=CARTESIAN_POINT('Ctrl Pts',(-33.6115742164079,20.3152448035298,15.));
#26352=CARTESIAN_POINT('Ctrl Pts',(-33.5463023319603,20.243500298383,15.));
#26353=CARTESIAN_POINT('Ctrl Pts',(-33.480563024813,20.1723475154533,15.));
#26354=CARTESIAN_POINT('Ctrl Pts',(-33.4143643679979,20.1017803986381,15.));
#26355=CARTESIAN_POINT('Ctrl Pts',(-33.3476854048385,20.0318342617213,15.));
#26356=CARTESIAN_POINT('Ctrl Pts',(-33.2804560993213,19.9626141625205,15.));
#26357=CARTESIAN_POINT('Ctrl Pts',(-33.2125746879471,19.8942704458546,15.));
#26358=CARTESIAN_POINT('Ctrl Pts',(-33.1439436707661,19.8269479776239,15.));
#26359=CARTESIAN_POINT('Ctrl Pts',(-33.0745026283418,19.7607398248651,15.));
#26360=CARTESIAN_POINT('Ctrl Pts',(-33.004256563411,19.6956473461873,15.));
#26361=CARTESIAN_POINT('Ctrl Pts',(-32.9333211533788,19.6315161742485,15.));
#26362=CARTESIAN_POINT('Ctrl Pts',(-32.8618672807884,19.5681157030437,15.));
#26363=CARTESIAN_POINT('Ctrl Pts',(-32.7900335943248,19.5052640847974,15.));
#26364=CARTESIAN_POINT('Ctrl Pts',(-32.7178463324062,19.4429429601189,15.));
#26365=CARTESIAN_POINT('Ctrl Pts',(-32.6451434870609,19.381405831319,15.));
#26366=CARTESIAN_POINT('Ctrl Pts',(-32.5714771007861,19.3213180490743,15.));
#26367=CARTESIAN_POINT('Ctrl Pts',(-32.4962340238036,19.2635813403783,15.));
#26368=CARTESIAN_POINT('Ctrl Pts',(-32.4342791270009,19.2200039764927,15.));
#26369=CARTESIAN_POINT('Ctrl Pts',(-32.3866012518553,19.1891139208368,15.));
#26370=CARTESIAN_POINT('Ctrl Pts',(-32.3542491343753,19.1693587749508,15.));
#26371=CARTESIAN_POINT('Ctrl Pts',(-32.3379313568208,19.1596907609891,15.));
#26372=CARTESIAN_POINT('',(-36.3957374383337,24.7254989094229,0.));
#26373=CARTESIAN_POINT('Origin',(-9.16871631793044E-12,6.66146233219319E-12,
0.));
#26374=CARTESIAN_POINT('',(-34.762248247709,26.9738038986838,0.));
#26375=CARTESIAN_POINT('Origin',(-9.16871631793044E-12,6.66146233219319E-12,
0.));
#26376=CARTESIAN_POINT('',(-34.762248247709,26.9738038986838,15.));
#26377=CARTESIAN_POINT('Origin',(-9.16871631793044E-12,6.66146233219319E-12,
15.));
#26378=CARTESIAN_POINT('',(-34.762248247709,26.9738038986838,0.));
#26379=CARTESIAN_POINT('Ctrl Pts',(-28.2149191006268,24.8345302882955,0.));
#26380=CARTESIAN_POINT('Ctrl Pts',(-28.2149191006268,24.8345302882955,18.));
#26381=CARTESIAN_POINT('Ctrl Pts',(-28.2291563988795,24.8470618363541,0.));
#26382=CARTESIAN_POINT('Ctrl Pts',(-28.2291563988795,24.8470618363541,18.));
#26383=CARTESIAN_POINT('Ctrl Pts',(-28.2579420132101,24.8717258526943,0.));
#26384=CARTESIAN_POINT('Ctrl Pts',(-28.2579420132101,24.8717258526943,18.));
#26385=CARTESIAN_POINT('Ctrl Pts',(-28.302053475606,24.9075246543798,0.));
#26386=CARTESIAN_POINT('Ctrl Pts',(-28.302053475606,24.9075246543798,18.));
#26387=CARTESIAN_POINT('Ctrl Pts',(-28.3626431274892,24.9529811166897,0.));
#26388=CARTESIAN_POINT('Ctrl Pts',(-28.3626431274892,24.9529811166897,18.));
#26389=CARTESIAN_POINT('Ctrl Pts',(-28.4408053900206,25.0066999111736,0.));
#26390=CARTESIAN_POINT('Ctrl Pts',(-28.4408053900206,25.0066999111736,18.));
#26391=CARTESIAN_POINT('Ctrl Pts',(-28.5207164321473,25.0581926620043,0.));
#26392=CARTESIAN_POINT('Ctrl Pts',(-28.5207164321473,25.0581926620043,18.));
#26393=CARTESIAN_POINT('Ctrl Pts',(-28.6017081342376,25.108321158239,0.));
#26394=CARTESIAN_POINT('Ctrl Pts',(-28.6017081342376,25.108321158239,18.));
#26395=CARTESIAN_POINT('Ctrl Pts',(-28.6832861366762,25.1577170374459,0.));
#26396=CARTESIAN_POINT('Ctrl Pts',(-28.6832861366762,25.1577170374459,18.));
#26397=CARTESIAN_POINT('Ctrl Pts',(-28.7652594076549,25.2066127148845,0.));
#26398=CARTESIAN_POINT('Ctrl Pts',(-28.7652594076549,25.2066127148845,18.));
#26399=CARTESIAN_POINT('Ctrl Pts',(-28.8476372998748,25.2549775629725,0.));
#26400=CARTESIAN_POINT('Ctrl Pts',(-28.8476372998748,25.2549775629725,18.));
#26401=CARTESIAN_POINT('Ctrl Pts',(-28.9305499160476,25.3026235249214,0.));
#26402=CARTESIAN_POINT('Ctrl Pts',(-28.9305499160476,25.3026235249214,18.));
#26403=CARTESIAN_POINT('Ctrl Pts',(-29.0141637699076,25.3493168206005,0.));
#26404=CARTESIAN_POINT('Ctrl Pts',(-29.0141637699076,25.3493168206005,18.));
#26405=CARTESIAN_POINT('Ctrl Pts',(-29.098589927237,25.3948997321279,0.));
#26406=CARTESIAN_POINT('Ctrl Pts',(-29.098589927237,25.3948997321279,18.));
#26407=CARTESIAN_POINT('Ctrl Pts',(-29.183825549991,25.4393679214513,0.));
#26408=CARTESIAN_POINT('Ctrl Pts',(-29.183825549991,25.4393679214513,18.));
#26409=CARTESIAN_POINT('Ctrl Pts',(-29.2698007967907,25.4828076101654,0.));
#26410=CARTESIAN_POINT('Ctrl Pts',(-29.2698007967907,25.4828076101654,18.));
#26411=CARTESIAN_POINT('Ctrl Pts',(-29.356408021119,25.5253562922582,0.));
#26412=CARTESIAN_POINT('Ctrl Pts',(-29.356408021119,25.5253562922582,18.));
#26413=CARTESIAN_POINT('Ctrl Pts',(-29.443535683207,25.5671572096726,0.));
#26414=CARTESIAN_POINT('Ctrl Pts',(-29.443535683207,25.5671572096726,18.));
#26415=CARTESIAN_POINT('Ctrl Pts',(-29.5311055094509,25.6083094352667,0.));
#26416=CARTESIAN_POINT('Ctrl Pts',(-29.5311055094509,25.6083094352667,18.));
#26417=CARTESIAN_POINT('Ctrl Pts',(-29.6190903904157,25.6488438125835,0.));
#26418=CARTESIAN_POINT('Ctrl Pts',(-29.6190903904157,25.6488438125835,18.));
#26419=CARTESIAN_POINT('Ctrl Pts',(-29.7074935910931,25.6887507922748,0.));
#26420=CARTESIAN_POINT('Ctrl Pts',(-29.7074935910931,25.6887507922748,18.));
#26421=CARTESIAN_POINT('Ctrl Pts',(-29.7963360859334,25.7279973711305,0.));
#26422=CARTESIAN_POINT('Ctrl Pts',(-29.7963360859334,25.7279973711305,18.));
#26423=CARTESIAN_POINT('Ctrl Pts',(-29.8856417535786,25.7665469042913,0.));
#26424=CARTESIAN_POINT('Ctrl Pts',(-29.8856417535786,25.7665469042913,18.));
#26425=CARTESIAN_POINT('Ctrl Pts',(-29.9754208429384,25.8043812318215,0.));
#26426=CARTESIAN_POINT('Ctrl Pts',(-29.9754208429384,25.8043812318215,18.));
#26427=CARTESIAN_POINT('Ctrl Pts',(-30.0656638016321,25.8415089241134,0.));
#26428=CARTESIAN_POINT('Ctrl Pts',(-30.0656638016321,25.8415089241134,18.));
#26429=CARTESIAN_POINT('Ctrl Pts',(-30.1563500154165,25.8779535511028,0.));
#26430=CARTESIAN_POINT('Ctrl Pts',(-30.1563500154165,25.8779535511028,18.));
#26431=CARTESIAN_POINT('Ctrl Pts',(-30.2474530144827,25.9137466853317,0.));
#26432=CARTESIAN_POINT('Ctrl Pts',(-30.2474530144827,25.9137466853317,18.));
#26433=CARTESIAN_POINT('Ctrl Pts',(-30.3389466074503,25.9489196635424,0.));
#26434=CARTESIAN_POINT('Ctrl Pts',(-30.3389466074503,25.9489196635424,18.));
#26435=CARTESIAN_POINT('Ctrl Pts',(-30.4308118142473,25.9834942765902,0.));
#26436=CARTESIAN_POINT('Ctrl Pts',(-30.4308118142473,25.9834942765902,18.));
#26437=CARTESIAN_POINT('Ctrl Pts',(-30.5230388264271,26.0174801292225,0.));
#26438=CARTESIAN_POINT('Ctrl Pts',(-30.5230388264271,26.0174801292225,18.));
#26439=CARTESIAN_POINT('Ctrl Pts',(-30.6156232634061,26.0508796503166,0.));
#26440=CARTESIAN_POINT('Ctrl Pts',(-30.6156232634061,26.0508796503166,18.));
#26441=CARTESIAN_POINT('Ctrl Pts',(-30.7085638682391,26.0836911730968,0.));
#26442=CARTESIAN_POINT('Ctrl Pts',(-30.7085638682391,26.0836911730968,18.));
#26443=CARTESIAN_POINT('Ctrl Pts',(-30.8018598357461,26.1159125093178,0.));
#26444=CARTESIAN_POINT('Ctrl Pts',(-30.8018598357461,26.1159125093178,18.));
#26445=CARTESIAN_POINT('Ctrl Pts',(-30.8955077633644,26.1475450294082,0.));
#26446=CARTESIAN_POINT('Ctrl Pts',(-30.8955077633644,26.1475450294082,18.));
#26447=CARTESIAN_POINT('Ctrl Pts',(-30.9895009017073,26.1785946616165,0.));
#26448=CARTESIAN_POINT('Ctrl Pts',(-30.9895009017073,26.1785946616165,18.));
#26449=CARTESIAN_POINT('Ctrl Pts',(-31.0838307058369,26.2090698085494,0.));
#26450=CARTESIAN_POINT('Ctrl Pts',(-31.0838307058369,26.2090698085494,18.));
#26451=CARTESIAN_POINT('Ctrl Pts',(-31.1784877826858,26.2389800738215,0.));
#26452=CARTESIAN_POINT('Ctrl Pts',(-31.1784877826858,26.2389800738215,18.));
#26453=CARTESIAN_POINT('Ctrl Pts',(-31.2734629900041,26.2683347859175,0.));
#26454=CARTESIAN_POINT('Ctrl Pts',(-31.2734629900041,26.2683347859175,18.));
#26455=CARTESIAN_POINT('Ctrl Pts',(-31.3687486937246,26.2971413115295,0.));
#26456=CARTESIAN_POINT('Ctrl Pts',(-31.3687486937246,26.2971413115295,18.));
#26457=CARTESIAN_POINT('Ctrl Pts',(-31.4643390378084,26.3254046890485,0.));
#26458=CARTESIAN_POINT('Ctrl Pts',(-31.4643390378084,26.3254046890485,18.));
#26459=CARTESIAN_POINT('Ctrl Pts',(-31.5602292672984,26.353128528169,0.));
#26460=CARTESIAN_POINT('Ctrl Pts',(-31.5602292672984,26.353128528169,18.));
#26461=CARTESIAN_POINT('Ctrl Pts',(-31.6564152990236,26.3803155790949,0.));
#26462=CARTESIAN_POINT('Ctrl Pts',(-31.6564152990236,26.3803155790949,18.));
#26463=CARTESIAN_POINT('Ctrl Pts',(-31.7528932299312,26.4069683862785,0.));
#26464=CARTESIAN_POINT('Ctrl Pts',(-31.7528932299312,26.4069683862785,18.));
#26465=CARTESIAN_POINT('Ctrl Pts',(-31.849658771403,26.433090040836,0.));
#26466=CARTESIAN_POINT('Ctrl Pts',(-31.849658771403,26.433090040836,18.));
#26467=CARTESIAN_POINT('Ctrl Pts',(-31.9467071093816,26.4586843683627,0.));
#26468=CARTESIAN_POINT('Ctrl Pts',(-31.9467071093816,26.4586843683627,18.));
#26469=CARTESIAN_POINT('Ctrl Pts',(-32.0440331917233,26.4837555495616,0.));
#26470=CARTESIAN_POINT('Ctrl Pts',(-32.0440331917233,26.4837555495616,18.));
#26471=CARTESIAN_POINT('Ctrl Pts',(-32.1416319023705,26.5083078928862,0.));
#26472=CARTESIAN_POINT('Ctrl Pts',(-32.1416319023705,26.5083078928862,18.));
#26473=CARTESIAN_POINT('Ctrl Pts',(-32.2394982626669,26.5323455701117,0.));
#26474=CARTESIAN_POINT('Ctrl Pts',(-32.2394982626669,26.5323455701117,18.));
#26475=CARTESIAN_POINT('Ctrl Pts',(-32.3376276606981,26.5558723200361,0.));
#26476=CARTESIAN_POINT('Ctrl Pts',(-32.3376276606981,26.5558723200361,18.));
#26477=CARTESIAN_POINT('Ctrl Pts',(-32.4360159072985,26.5788913672813,0.));
#26478=CARTESIAN_POINT('Ctrl Pts',(-32.4360159072985,26.5788913672813,18.));
#26479=CARTESIAN_POINT('Ctrl Pts',(-32.5346590925498,26.6014055904817,0.));
#26480=CARTESIAN_POINT('Ctrl Pts',(-32.5346590925498,26.6014055904817,18.));
#26481=CARTESIAN_POINT('Ctrl Pts',(-32.6335534898935,26.6234176311245,0.));
#26482=CARTESIAN_POINT('Ctrl Pts',(-32.6335534898935,26.6234176311245,18.));
#26483=CARTESIAN_POINT('Ctrl Pts',(-32.7326954489334,26.6449300199764,0.));
#26484=CARTESIAN_POINT('Ctrl Pts',(-32.7326954489334,26.6449300199764,18.));
#26485=CARTESIAN_POINT('Ctrl Pts',(-32.8320812678271,26.6659453236976,0.));
#26486=CARTESIAN_POINT('Ctrl Pts',(-32.8320812678271,26.6659453236976,18.));
#26487=CARTESIAN_POINT('Ctrl Pts',(-32.9317071576181,26.6864661988935,0.));
#26488=CARTESIAN_POINT('Ctrl Pts',(-32.9317071576181,26.6864661988935,18.));
#26489=CARTESIAN_POINT('Ctrl Pts',(-33.03156933761,26.7064953106254,0.));
#26490=CARTESIAN_POINT('Ctrl Pts',(-33.03156933761,26.7064953106254,18.));
#26491=CARTESIAN_POINT('Ctrl Pts',(-33.131664100194,26.7260352861619,0.));
#26492=CARTESIAN_POINT('Ctrl Pts',(-33.131664100194,26.7260352861619,18.));
#26493=CARTESIAN_POINT('Ctrl Pts',(-33.2319878786519,26.7450886617884,0.));
#26494=CARTESIAN_POINT('Ctrl Pts',(-33.2319878786519,26.7450886617884,18.));
#26495=CARTESIAN_POINT('Ctrl Pts',(-33.3325373307046,26.7636578270526,0.));
#26496=CARTESIAN_POINT('Ctrl Pts',(-33.3325373307046,26.7636578270526,18.));
#26497=CARTESIAN_POINT('Ctrl Pts',(-33.4333093513694,26.7817450041181,0.));
#26498=CARTESIAN_POINT('Ctrl Pts',(-33.4333093513694,26.7817450041181,18.));
#26499=CARTESIAN_POINT('Ctrl Pts',(-33.5343009499673,26.7993522966985,0.));
#26500=CARTESIAN_POINT('Ctrl Pts',(-33.5343009499673,26.7993522966985,18.));
#26501=CARTESIAN_POINT('Ctrl Pts',(-33.6355091508895,26.8164817280846,0.));
#26502=CARTESIAN_POINT('Ctrl Pts',(-33.6355091508895,26.8164817280846,18.));
#26503=CARTESIAN_POINT('Ctrl Pts',(-33.7369308933173,26.8331352836667,0.));
#26504=CARTESIAN_POINT('Ctrl Pts',(-33.7369308933173,26.8331352836667,18.));
#26505=CARTESIAN_POINT('Ctrl Pts',(-33.838562905895,26.8493149627661,0.));
#26506=CARTESIAN_POINT('Ctrl Pts',(-33.838562905895,26.8493149627661,18.));
#26507=CARTESIAN_POINT('Ctrl Pts',(-33.9404016650487,26.8650228056313,0.));
#26508=CARTESIAN_POINT('Ctrl Pts',(-33.9404016650487,26.8650228056313,18.));
#26509=CARTESIAN_POINT('Ctrl Pts',(-34.0424436187397,26.880260834701,0.));
#26510=CARTESIAN_POINT('Ctrl Pts',(-34.0424436187397,26.880260834701,18.));
#26511=CARTESIAN_POINT('Ctrl Pts',(-34.1446853651051,26.895031013894,0.));
#26512=CARTESIAN_POINT('Ctrl Pts',(-34.1446853651051,26.895031013894,18.));
#26513=CARTESIAN_POINT('Ctrl Pts',(-34.2471238425419,26.9093352037262,0.));
#26514=CARTESIAN_POINT('Ctrl Pts',(-34.2471238425419,26.9093352037262,18.));
#26515=CARTESIAN_POINT('Ctrl Pts',(-34.3497565255724,26.9231751225177,0.));
#26516=CARTESIAN_POINT('Ctrl Pts',(-34.3497565255724,26.9231751225177,18.));
#26517=CARTESIAN_POINT('Ctrl Pts',(-34.4525815829097,26.9365523054581,0.));
#26518=CARTESIAN_POINT('Ctrl Pts',(-34.4525815829097,26.9365523054581,18.));
#26519=CARTESIAN_POINT('Ctrl Pts',(-34.5555977590573,26.9494680440307,0.));
#26520=CARTESIAN_POINT('Ctrl Pts',(-34.5555977590573,26.9494680440307,18.));
#26521=CARTESIAN_POINT('Ctrl Pts',(-34.6381629799782,26.9594322726214,0.));
#26522=CARTESIAN_POINT('Ctrl Pts',(-34.6381629799782,26.9594322726214,18.));
#26523=CARTESIAN_POINT('Ctrl Pts',(-34.700172380686,26.9666985267609,0.));
#26524=CARTESIAN_POINT('Ctrl Pts',(-34.700172380686,26.9666985267609,18.));
#26525=CARTESIAN_POINT('Ctrl Pts',(-34.7415499619104,26.9714507634923,0.));
#26526=CARTESIAN_POINT('Ctrl Pts',(-34.7415499619104,26.9714507634923,18.));
#26527=CARTESIAN_POINT('Ctrl Pts',(-34.7622482477091,26.9738038986838,0.));
#26528=CARTESIAN_POINT('Ctrl Pts',(-34.7622482477091,26.9738038986838,18.));
#26529=CARTESIAN_POINT('Ctrl Pts',(-28.2149191006268,24.8345302882955,0.));
#26530=CARTESIAN_POINT('Ctrl Pts',(-28.2291563988795,24.8470618363541,0.));
#26531=CARTESIAN_POINT('Ctrl Pts',(-28.2579420132101,24.8717258526943,0.));
#26532=CARTESIAN_POINT('Ctrl Pts',(-28.302053475606,24.9075246543798,0.));
#26533=CARTESIAN_POINT('Ctrl Pts',(-28.3626431274892,24.9529811166897,0.));
#26534=CARTESIAN_POINT('Ctrl Pts',(-28.4408053900206,25.0066999111736,0.));
#26535=CARTESIAN_POINT('Ctrl Pts',(-28.5207164321473,25.0581926620043,0.));
#26536=CARTESIAN_POINT('Ctrl Pts',(-28.6017081342376,25.108321158239,0.));
#26537=CARTESIAN_POINT('Ctrl Pts',(-28.6832861366762,25.1577170374459,0.));
#26538=CARTESIAN_POINT('Ctrl Pts',(-28.7652594076549,25.2066127148845,0.));
#26539=CARTESIAN_POINT('Ctrl Pts',(-28.8476372998748,25.2549775629725,0.));
#26540=CARTESIAN_POINT('Ctrl Pts',(-28.9305499160476,25.3026235249214,0.));
#26541=CARTESIAN_POINT('Ctrl Pts',(-29.0141637699076,25.3493168206005,0.));
#26542=CARTESIAN_POINT('Ctrl Pts',(-29.098589927237,25.3948997321279,0.));
#26543=CARTESIAN_POINT('Ctrl Pts',(-29.183825549991,25.4393679214513,0.));
#26544=CARTESIAN_POINT('Ctrl Pts',(-29.2698007967907,25.4828076101654,0.));
#26545=CARTESIAN_POINT('Ctrl Pts',(-29.356408021119,25.5253562922582,0.));
#26546=CARTESIAN_POINT('Ctrl Pts',(-29.443535683207,25.5671572096726,0.));
#26547=CARTESIAN_POINT('Ctrl Pts',(-29.5311055094509,25.6083094352667,0.));
#26548=CARTESIAN_POINT('Ctrl Pts',(-29.6190903904157,25.6488438125835,0.));
#26549=CARTESIAN_POINT('Ctrl Pts',(-29.7074935910931,25.6887507922748,0.));
#26550=CARTESIAN_POINT('Ctrl Pts',(-29.7963360859334,25.7279973711305,0.));
#26551=CARTESIAN_POINT('Ctrl Pts',(-29.8856417535786,25.7665469042913,0.));
#26552=CARTESIAN_POINT('Ctrl Pts',(-29.9754208429384,25.8043812318215,0.));
#26553=CARTESIAN_POINT('Ctrl Pts',(-30.0656638016321,25.8415089241134,0.));
#26554=CARTESIAN_POINT('Ctrl Pts',(-30.1563500154165,25.8779535511028,0.));
#26555=CARTESIAN_POINT('Ctrl Pts',(-30.2474530144827,25.9137466853317,0.));
#26556=CARTESIAN_POINT('Ctrl Pts',(-30.3389466074503,25.9489196635424,0.));
#26557=CARTESIAN_POINT('Ctrl Pts',(-30.4308118142473,25.9834942765902,0.));
#26558=CARTESIAN_POINT('Ctrl Pts',(-30.5230388264271,26.0174801292225,0.));
#26559=CARTESIAN_POINT('Ctrl Pts',(-30.6156232634061,26.0508796503166,0.));
#26560=CARTESIAN_POINT('Ctrl Pts',(-30.7085638682391,26.0836911730968,0.));
#26561=CARTESIAN_POINT('Ctrl Pts',(-30.8018598357461,26.1159125093178,0.));
#26562=CARTESIAN_POINT('Ctrl Pts',(-30.8955077633644,26.1475450294082,0.));
#26563=CARTESIAN_POINT('Ctrl Pts',(-30.9895009017073,26.1785946616165,0.));
#26564=CARTESIAN_POINT('Ctrl Pts',(-31.0838307058369,26.2090698085494,0.));
#26565=CARTESIAN_POINT('Ctrl Pts',(-31.1784877826858,26.2389800738215,0.));
#26566=CARTESIAN_POINT('Ctrl Pts',(-31.2734629900041,26.2683347859175,0.));
#26567=CARTESIAN_POINT('Ctrl Pts',(-31.3687486937246,26.2971413115295,0.));
#26568=CARTESIAN_POINT('Ctrl Pts',(-31.4643390378084,26.3254046890485,0.));
#26569=CARTESIAN_POINT('Ctrl Pts',(-31.5602292672984,26.353128528169,0.));
#26570=CARTESIAN_POINT('Ctrl Pts',(-31.6564152990236,26.3803155790949,0.));
#26571=CARTESIAN_POINT('Ctrl Pts',(-31.7528932299312,26.4069683862785,0.));
#26572=CARTESIAN_POINT('Ctrl Pts',(-31.849658771403,26.433090040836,0.));
#26573=CARTESIAN_POINT('Ctrl Pts',(-31.9467071093816,26.4586843683627,0.));
#26574=CARTESIAN_POINT('Ctrl Pts',(-32.0440331917233,26.4837555495616,0.));
#26575=CARTESIAN_POINT('Ctrl Pts',(-32.1416319023705,26.5083078928862,0.));
#26576=CARTESIAN_POINT('Ctrl Pts',(-32.2394982626669,26.5323455701117,0.));
#26577=CARTESIAN_POINT('Ctrl Pts',(-32.3376276606981,26.5558723200361,0.));
#26578=CARTESIAN_POINT('Ctrl Pts',(-32.4360159072985,26.5788913672813,0.));
#26579=CARTESIAN_POINT('Ctrl Pts',(-32.5346590925498,26.6014055904817,0.));
#26580=CARTESIAN_POINT('Ctrl Pts',(-32.6335534898935,26.6234176311245,0.));
#26581=CARTESIAN_POINT('Ctrl Pts',(-32.7326954489334,26.6449300199764,0.));
#26582=CARTESIAN_POINT('Ctrl Pts',(-32.8320812678271,26.6659453236976,0.));
#26583=CARTESIAN_POINT('Ctrl Pts',(-32.9317071576181,26.6864661988935,0.));
#26584=CARTESIAN_POINT('Ctrl Pts',(-33.03156933761,26.7064953106254,0.));
#26585=CARTESIAN_POINT('Ctrl Pts',(-33.131664100194,26.7260352861619,0.));
#26586=CARTESIAN_POINT('Ctrl Pts',(-33.2319878786519,26.7450886617884,0.));
#26587=CARTESIAN_POINT('Ctrl Pts',(-33.3325373307046,26.7636578270526,0.));
#26588=CARTESIAN_POINT('Ctrl Pts',(-33.4333093513694,26.7817450041181,0.));
#26589=CARTESIAN_POINT('Ctrl Pts',(-33.5343009499673,26.7993522966985,0.));
#26590=CARTESIAN_POINT('Ctrl Pts',(-33.6355091508895,26.8164817280846,0.));
#26591=CARTESIAN_POINT('Ctrl Pts',(-33.7369308933173,26.8331352836667,0.));
#26592=CARTESIAN_POINT('Ctrl Pts',(-33.838562905895,26.8493149627661,0.));
#26593=CARTESIAN_POINT('Ctrl Pts',(-33.9404016650487,26.8650228056313,0.));
#26594=CARTESIAN_POINT('Ctrl Pts',(-34.0424436187397,26.880260834701,0.));
#26595=CARTESIAN_POINT('Ctrl Pts',(-34.1446853651051,26.895031013894,0.));
#26596=CARTESIAN_POINT('Ctrl Pts',(-34.2471238425419,26.9093352037262,0.));
#26597=CARTESIAN_POINT('Ctrl Pts',(-34.3497565255724,26.9231751225177,0.));
#26598=CARTESIAN_POINT('Ctrl Pts',(-34.4731465943772,26.9392277420462,0.));
#26599=CARTESIAN_POINT('Ctrl Pts',(-34.5762105502273,26.9520281195268,0.));
#26600=CARTESIAN_POINT('Ctrl Pts',(-34.6588137898952,26.9619003236529,0.));
#26601=CARTESIAN_POINT('Ctrl Pts',(-34.7208516760814,26.9690976283149,0.));
#26602=CARTESIAN_POINT('Ctrl Pts',(-34.7622482477091,26.9738038986838,0.));
#26603=CARTESIAN_POINT('Ctrl Pts',(-28.2149191006268,24.8345302882955,15.));
#26604=CARTESIAN_POINT('Ctrl Pts',(-28.2291563988795,24.8470618363541,15.));
#26605=CARTESIAN_POINT('Ctrl Pts',(-28.2579420132101,24.8717258526943,15.));
#26606=CARTESIAN_POINT('Ctrl Pts',(-28.302053475606,24.9075246543798,15.));
#26607=CARTESIAN_POINT('Ctrl Pts',(-28.3626431274892,24.9529811166897,15.));
#26608=CARTESIAN_POINT('Ctrl Pts',(-28.4408053900206,25.0066999111736,15.));
#26609=CARTESIAN_POINT('Ctrl Pts',(-28.5207164321473,25.0581926620043,15.));
#26610=CARTESIAN_POINT('Ctrl Pts',(-28.6017081342376,25.108321158239,15.));
#26611=CARTESIAN_POINT('Ctrl Pts',(-28.6832861366762,25.1577170374459,15.));
#26612=CARTESIAN_POINT('Ctrl Pts',(-28.7652594076549,25.2066127148845,15.));
#26613=CARTESIAN_POINT('Ctrl Pts',(-28.8476372998748,25.2549775629725,15.));
#26614=CARTESIAN_POINT('Ctrl Pts',(-28.9305499160476,25.3026235249214,15.));
#26615=CARTESIAN_POINT('Ctrl Pts',(-29.0141637699076,25.3493168206005,15.));
#26616=CARTESIAN_POINT('Ctrl Pts',(-29.098589927237,25.3948997321279,15.));
#26617=CARTESIAN_POINT('Ctrl Pts',(-29.183825549991,25.4393679214513,15.));
#26618=CARTESIAN_POINT('Ctrl Pts',(-29.2698007967907,25.4828076101654,15.));
#26619=CARTESIAN_POINT('Ctrl Pts',(-29.356408021119,25.5253562922582,15.));
#26620=CARTESIAN_POINT('Ctrl Pts',(-29.443535683207,25.5671572096726,15.));
#26621=CARTESIAN_POINT('Ctrl Pts',(-29.5311055094509,25.6083094352667,15.));
#26622=CARTESIAN_POINT('Ctrl Pts',(-29.6190903904157,25.6488438125835,15.));
#26623=CARTESIAN_POINT('Ctrl Pts',(-29.7074935910931,25.6887507922748,15.));
#26624=CARTESIAN_POINT('Ctrl Pts',(-29.7963360859334,25.7279973711305,15.));
#26625=CARTESIAN_POINT('Ctrl Pts',(-29.8856417535786,25.7665469042913,15.));
#26626=CARTESIAN_POINT('Ctrl Pts',(-29.9754208429384,25.8043812318215,15.));
#26627=CARTESIAN_POINT('Ctrl Pts',(-30.0656638016321,25.8415089241134,15.));
#26628=CARTESIAN_POINT('Ctrl Pts',(-30.1563500154165,25.8779535511028,15.));
#26629=CARTESIAN_POINT('Ctrl Pts',(-30.2474530144827,25.9137466853317,15.));
#26630=CARTESIAN_POINT('Ctrl Pts',(-30.3389466074503,25.9489196635424,15.));
#26631=CARTESIAN_POINT('Ctrl Pts',(-30.4308118142473,25.9834942765902,15.));
#26632=CARTESIAN_POINT('Ctrl Pts',(-30.5230388264271,26.0174801292225,15.));
#26633=CARTESIAN_POINT('Ctrl Pts',(-30.6156232634061,26.0508796503166,15.));
#26634=CARTESIAN_POINT('Ctrl Pts',(-30.7085638682391,26.0836911730968,15.));
#26635=CARTESIAN_POINT('Ctrl Pts',(-30.8018598357461,26.1159125093178,15.));
#26636=CARTESIAN_POINT('Ctrl Pts',(-30.8955077633644,26.1475450294082,15.));
#26637=CARTESIAN_POINT('Ctrl Pts',(-30.9895009017073,26.1785946616165,15.));
#26638=CARTESIAN_POINT('Ctrl Pts',(-31.0838307058369,26.2090698085494,15.));
#26639=CARTESIAN_POINT('Ctrl Pts',(-31.1784877826858,26.2389800738215,15.));
#26640=CARTESIAN_POINT('Ctrl Pts',(-31.2734629900041,26.2683347859175,15.));
#26641=CARTESIAN_POINT('Ctrl Pts',(-31.3687486937246,26.2971413115295,15.));
#26642=CARTESIAN_POINT('Ctrl Pts',(-31.4643390378084,26.3254046890485,15.));
#26643=CARTESIAN_POINT('Ctrl Pts',(-31.5602292672984,26.353128528169,15.));
#26644=CARTESIAN_POINT('Ctrl Pts',(-31.6564152990236,26.3803155790949,15.));
#26645=CARTESIAN_POINT('Ctrl Pts',(-31.7528932299312,26.4069683862785,15.));
#26646=CARTESIAN_POINT('Ctrl Pts',(-31.849658771403,26.433090040836,15.));
#26647=CARTESIAN_POINT('Ctrl Pts',(-31.9467071093816,26.4586843683627,15.));
#26648=CARTESIAN_POINT('Ctrl Pts',(-32.0440331917233,26.4837555495616,15.));
#26649=CARTESIAN_POINT('Ctrl Pts',(-32.1416319023705,26.5083078928862,15.));
#26650=CARTESIAN_POINT('Ctrl Pts',(-32.2394982626669,26.5323455701117,15.));
#26651=CARTESIAN_POINT('Ctrl Pts',(-32.3376276606981,26.5558723200361,15.));
#26652=CARTESIAN_POINT('Ctrl Pts',(-32.4360159072985,26.5788913672813,15.));
#26653=CARTESIAN_POINT('Ctrl Pts',(-32.5346590925498,26.6014055904817,15.));
#26654=CARTESIAN_POINT('Ctrl Pts',(-32.6335534898935,26.6234176311245,15.));
#26655=CARTESIAN_POINT('Ctrl Pts',(-32.7326954489334,26.6449300199764,15.));
#26656=CARTESIAN_POINT('Ctrl Pts',(-32.8320812678271,26.6659453236976,15.));
#26657=CARTESIAN_POINT('Ctrl Pts',(-32.9317071576181,26.6864661988935,15.));
#26658=CARTESIAN_POINT('Ctrl Pts',(-33.03156933761,26.7064953106254,15.));
#26659=CARTESIAN_POINT('Ctrl Pts',(-33.131664100194,26.7260352861619,15.));
#26660=CARTESIAN_POINT('Ctrl Pts',(-33.2319878786519,26.7450886617884,15.));
#26661=CARTESIAN_POINT('Ctrl Pts',(-33.3325373307046,26.7636578270526,15.));
#26662=CARTESIAN_POINT('Ctrl Pts',(-33.4333093513694,26.7817450041181,15.));
#26663=CARTESIAN_POINT('Ctrl Pts',(-33.5343009499673,26.7993522966985,15.));
#26664=CARTESIAN_POINT('Ctrl Pts',(-33.6355091508895,26.8164817280846,15.));
#26665=CARTESIAN_POINT('Ctrl Pts',(-33.7369308933173,26.8331352836667,15.));
#26666=CARTESIAN_POINT('Ctrl Pts',(-33.838562905895,26.8493149627661,15.));
#26667=CARTESIAN_POINT('Ctrl Pts',(-33.9404016650487,26.8650228056313,15.));
#26668=CARTESIAN_POINT('Ctrl Pts',(-34.0424436187397,26.880260834701,15.));
#26669=CARTESIAN_POINT('Ctrl Pts',(-34.1446853651051,26.895031013894,15.));
#26670=CARTESIAN_POINT('Ctrl Pts',(-34.2471238425419,26.9093352037262,15.));
#26671=CARTESIAN_POINT('Ctrl Pts',(-34.3497565255724,26.9231751225177,15.));
#26672=CARTESIAN_POINT('Ctrl Pts',(-34.4731465943772,26.9392277420462,15.));
#26673=CARTESIAN_POINT('Ctrl Pts',(-34.5762105502273,26.9520281195268,15.));
#26674=CARTESIAN_POINT('Ctrl Pts',(-34.6588137898952,26.9619003236529,15.));
#26675=CARTESIAN_POINT('Ctrl Pts',(-34.7208516760814,26.9690976283149,15.));
#26676=CARTESIAN_POINT('Ctrl Pts',(-34.7622482477091,26.9738038986838,15.));
#26677=CARTESIAN_POINT('Ctrl Pts',(-26.9738038986838,34.7622482477091,0.));
#26678=CARTESIAN_POINT('Ctrl Pts',(-26.9738038986838,34.7622482477091,18.));
#26679=CARTESIAN_POINT('Ctrl Pts',(-26.9714507634923,34.7415499619104,0.));
#26680=CARTESIAN_POINT('Ctrl Pts',(-26.9714507634923,34.7415499619104,18.));
#26681=CARTESIAN_POINT('Ctrl Pts',(-26.9666985267608,34.700172380686,0.));
#26682=CARTESIAN_POINT('Ctrl Pts',(-26.9666985267608,34.700172380686,18.));
#26683=CARTESIAN_POINT('Ctrl Pts',(-26.9594322726214,34.6381629799782,0.));
#26684=CARTESIAN_POINT('Ctrl Pts',(-26.9594322726214,34.6381629799782,18.));
#26685=CARTESIAN_POINT('Ctrl Pts',(-26.9494680440307,34.5555977590573,0.));
#26686=CARTESIAN_POINT('Ctrl Pts',(-26.9494680440307,34.5555977590573,18.));
#26687=CARTESIAN_POINT('Ctrl Pts',(-26.9365523054581,34.4525815829097,0.));
#26688=CARTESIAN_POINT('Ctrl Pts',(-26.9365523054581,34.4525815829097,18.));
#26689=CARTESIAN_POINT('Ctrl Pts',(-26.9231751225177,34.3497565255724,0.));
#26690=CARTESIAN_POINT('Ctrl Pts',(-26.9231751225177,34.3497565255724,18.));
#26691=CARTESIAN_POINT('Ctrl Pts',(-26.9093352037262,34.2471238425419,0.));
#26692=CARTESIAN_POINT('Ctrl Pts',(-26.9093352037262,34.2471238425419,18.));
#26693=CARTESIAN_POINT('Ctrl Pts',(-26.8950310138939,34.1446853651051,0.));
#26694=CARTESIAN_POINT('Ctrl Pts',(-26.8950310138939,34.1446853651051,18.));
#26695=CARTESIAN_POINT('Ctrl Pts',(-26.880260834701,34.0424436187397,0.));
#26696=CARTESIAN_POINT('Ctrl Pts',(-26.880260834701,34.0424436187397,18.));
#26697=CARTESIAN_POINT('Ctrl Pts',(-26.8650228056313,33.9404016650487,0.));
#26698=CARTESIAN_POINT('Ctrl Pts',(-26.8650228056313,33.9404016650487,18.));
#26699=CARTESIAN_POINT('Ctrl Pts',(-26.8493149627661,33.838562905895,0.));
#26700=CARTESIAN_POINT('Ctrl Pts',(-26.8493149627661,33.838562905895,18.));
#26701=CARTESIAN_POINT('Ctrl Pts',(-26.8331352836666,33.7369308933173,0.));
#26702=CARTESIAN_POINT('Ctrl Pts',(-26.8331352836666,33.7369308933173,18.));
#26703=CARTESIAN_POINT('Ctrl Pts',(-26.8164817280846,33.6355091508895,0.));
#26704=CARTESIAN_POINT('Ctrl Pts',(-26.8164817280846,33.6355091508895,18.));
#26705=CARTESIAN_POINT('Ctrl Pts',(-26.7993522966985,33.5343009499673,0.));
#26706=CARTESIAN_POINT('Ctrl Pts',(-26.7993522966985,33.5343009499673,18.));
#26707=CARTESIAN_POINT('Ctrl Pts',(-26.7817450041181,33.4333093513694,0.));
#26708=CARTESIAN_POINT('Ctrl Pts',(-26.7817450041181,33.4333093513694,18.));
#26709=CARTESIAN_POINT('Ctrl Pts',(-26.7636578270526,33.3325373307046,0.));
#26710=CARTESIAN_POINT('Ctrl Pts',(-26.7636578270526,33.3325373307046,18.));
#26711=CARTESIAN_POINT('Ctrl Pts',(-26.7450886617884,33.2319878786519,0.));
#26712=CARTESIAN_POINT('Ctrl Pts',(-26.7450886617884,33.2319878786519,18.));
#26713=CARTESIAN_POINT('Ctrl Pts',(-26.7260352861619,33.131664100194,0.));
#26714=CARTESIAN_POINT('Ctrl Pts',(-26.7260352861619,33.131664100194,18.));
#26715=CARTESIAN_POINT('Ctrl Pts',(-26.7064953106254,33.03156933761,0.));
#26716=CARTESIAN_POINT('Ctrl Pts',(-26.7064953106254,33.03156933761,18.));
#26717=CARTESIAN_POINT('Ctrl Pts',(-26.6864661988935,32.9317071576181,0.));
#26718=CARTESIAN_POINT('Ctrl Pts',(-26.6864661988935,32.9317071576181,18.));
#26719=CARTESIAN_POINT('Ctrl Pts',(-26.6659453236976,32.8320812678271,0.));
#26720=CARTESIAN_POINT('Ctrl Pts',(-26.6659453236976,32.8320812678271,18.));
#26721=CARTESIAN_POINT('Ctrl Pts',(-26.6449300199763,32.7326954489334,0.));
#26722=CARTESIAN_POINT('Ctrl Pts',(-26.6449300199763,32.7326954489334,18.));
#26723=CARTESIAN_POINT('Ctrl Pts',(-26.6234176311245,32.6335534898936,0.));
#26724=CARTESIAN_POINT('Ctrl Pts',(-26.6234176311245,32.6335534898936,18.));
#26725=CARTESIAN_POINT('Ctrl Pts',(-26.6014055904817,32.5346590925498,0.));
#26726=CARTESIAN_POINT('Ctrl Pts',(-26.6014055904817,32.5346590925498,18.));
#26727=CARTESIAN_POINT('Ctrl Pts',(-26.5788913672813,32.4360159072985,0.));
#26728=CARTESIAN_POINT('Ctrl Pts',(-26.5788913672813,32.4360159072985,18.));
#26729=CARTESIAN_POINT('Ctrl Pts',(-26.5558723200361,32.3376276606981,0.));
#26730=CARTESIAN_POINT('Ctrl Pts',(-26.5558723200361,32.3376276606981,18.));
#26731=CARTESIAN_POINT('Ctrl Pts',(-26.5323455701117,32.2394982626669,0.));
#26732=CARTESIAN_POINT('Ctrl Pts',(-26.5323455701117,32.2394982626669,18.));
#26733=CARTESIAN_POINT('Ctrl Pts',(-26.5083078928862,32.1416319023705,0.));
#26734=CARTESIAN_POINT('Ctrl Pts',(-26.5083078928862,32.1416319023705,18.));
#26735=CARTESIAN_POINT('Ctrl Pts',(-26.4837555495616,32.0440331917233,0.));
#26736=CARTESIAN_POINT('Ctrl Pts',(-26.4837555495616,32.0440331917233,18.));
#26737=CARTESIAN_POINT('Ctrl Pts',(-26.4586843683627,31.9467071093816,0.));
#26738=CARTESIAN_POINT('Ctrl Pts',(-26.4586843683627,31.9467071093816,18.));
#26739=CARTESIAN_POINT('Ctrl Pts',(-26.433090040836,31.849658771403,0.));
#26740=CARTESIAN_POINT('Ctrl Pts',(-26.433090040836,31.849658771403,18.));
#26741=CARTESIAN_POINT('Ctrl Pts',(-26.4069683862784,31.7528932299312,0.));
#26742=CARTESIAN_POINT('Ctrl Pts',(-26.4069683862784,31.7528932299312,18.));
#26743=CARTESIAN_POINT('Ctrl Pts',(-26.3803155790949,31.6564152990236,0.));
#26744=CARTESIAN_POINT('Ctrl Pts',(-26.3803155790949,31.6564152990236,18.));
#26745=CARTESIAN_POINT('Ctrl Pts',(-26.353128528169,31.5602292672984,0.));
#26746=CARTESIAN_POINT('Ctrl Pts',(-26.353128528169,31.5602292672984,18.));
#26747=CARTESIAN_POINT('Ctrl Pts',(-26.3254046890485,31.4643390378084,0.));
#26748=CARTESIAN_POINT('Ctrl Pts',(-26.3254046890485,31.4643390378084,18.));
#26749=CARTESIAN_POINT('Ctrl Pts',(-26.2971413115295,31.3687486937246,0.));
#26750=CARTESIAN_POINT('Ctrl Pts',(-26.2971413115295,31.3687486937246,18.));
#26751=CARTESIAN_POINT('Ctrl Pts',(-26.2683347859175,31.2734629900041,0.));
#26752=CARTESIAN_POINT('Ctrl Pts',(-26.2683347859175,31.2734629900041,18.));
#26753=CARTESIAN_POINT('Ctrl Pts',(-26.2389800738215,31.1784877826858,0.));
#26754=CARTESIAN_POINT('Ctrl Pts',(-26.2389800738215,31.1784877826858,18.));
#26755=CARTESIAN_POINT('Ctrl Pts',(-26.2090698085494,31.0838307058369,0.));
#26756=CARTESIAN_POINT('Ctrl Pts',(-26.2090698085494,31.0838307058369,18.));
#26757=CARTESIAN_POINT('Ctrl Pts',(-26.1785946616165,30.9895009017073,0.));
#26758=CARTESIAN_POINT('Ctrl Pts',(-26.1785946616165,30.9895009017073,18.));
#26759=CARTESIAN_POINT('Ctrl Pts',(-26.1475450294082,30.8955077633644,0.));
#26760=CARTESIAN_POINT('Ctrl Pts',(-26.1475450294082,30.8955077633644,18.));
#26761=CARTESIAN_POINT('Ctrl Pts',(-26.1159125093178,30.8018598357461,0.));
#26762=CARTESIAN_POINT('Ctrl Pts',(-26.1159125093178,30.8018598357461,18.));
#26763=CARTESIAN_POINT('Ctrl Pts',(-26.0836911730968,30.7085638682391,0.));
#26764=CARTESIAN_POINT('Ctrl Pts',(-26.0836911730968,30.7085638682391,18.));
#26765=CARTESIAN_POINT('Ctrl Pts',(-26.0508796503166,30.6156232634061,0.));
#26766=CARTESIAN_POINT('Ctrl Pts',(-26.0508796503166,30.6156232634061,18.));
#26767=CARTESIAN_POINT('Ctrl Pts',(-26.0174801292225,30.5230388264271,0.));
#26768=CARTESIAN_POINT('Ctrl Pts',(-26.0174801292225,30.5230388264271,18.));
#26769=CARTESIAN_POINT('Ctrl Pts',(-25.9834942765902,30.4308118142473,0.));
#26770=CARTESIAN_POINT('Ctrl Pts',(-25.9834942765902,30.4308118142473,18.));
#26771=CARTESIAN_POINT('Ctrl Pts',(-25.9489196635424,30.3389466074503,0.));
#26772=CARTESIAN_POINT('Ctrl Pts',(-25.9489196635424,30.3389466074503,18.));
#26773=CARTESIAN_POINT('Ctrl Pts',(-25.9137466853317,30.2474530144827,0.));
#26774=CARTESIAN_POINT('Ctrl Pts',(-25.9137466853317,30.2474530144827,18.));
#26775=CARTESIAN_POINT('Ctrl Pts',(-25.8779535511027,30.1563500154165,0.));
#26776=CARTESIAN_POINT('Ctrl Pts',(-25.8779535511027,30.1563500154165,18.));
#26777=CARTESIAN_POINT('Ctrl Pts',(-25.8415089241134,30.0656638016321,0.));
#26778=CARTESIAN_POINT('Ctrl Pts',(-25.8415089241134,30.0656638016321,18.));
#26779=CARTESIAN_POINT('Ctrl Pts',(-25.8043812318214,29.9754208429384,0.));
#26780=CARTESIAN_POINT('Ctrl Pts',(-25.8043812318214,29.9754208429384,18.));
#26781=CARTESIAN_POINT('Ctrl Pts',(-25.7665469042913,29.8856417535786,0.));
#26782=CARTESIAN_POINT('Ctrl Pts',(-25.7665469042913,29.8856417535786,18.));
#26783=CARTESIAN_POINT('Ctrl Pts',(-25.7279973711305,29.7963360859334,0.));
#26784=CARTESIAN_POINT('Ctrl Pts',(-25.7279973711305,29.7963360859334,18.));
#26785=CARTESIAN_POINT('Ctrl Pts',(-25.6887507922748,29.7074935910931,0.));
#26786=CARTESIAN_POINT('Ctrl Pts',(-25.6887507922748,29.7074935910931,18.));
#26787=CARTESIAN_POINT('Ctrl Pts',(-25.6488438125835,29.6190903904157,0.));
#26788=CARTESIAN_POINT('Ctrl Pts',(-25.6488438125835,29.6190903904157,18.));
#26789=CARTESIAN_POINT('Ctrl Pts',(-25.6083094352667,29.5311055094509,0.));
#26790=CARTESIAN_POINT('Ctrl Pts',(-25.6083094352667,29.5311055094509,18.));
#26791=CARTESIAN_POINT('Ctrl Pts',(-25.5671572096726,29.443535683207,0.));
#26792=CARTESIAN_POINT('Ctrl Pts',(-25.5671572096726,29.443535683207,18.));
#26793=CARTESIAN_POINT('Ctrl Pts',(-25.5253562922582,29.356408021119,0.));
#26794=CARTESIAN_POINT('Ctrl Pts',(-25.5253562922582,29.356408021119,18.));
#26795=CARTESIAN_POINT('Ctrl Pts',(-25.4828076101654,29.2698007967907,0.));
#26796=CARTESIAN_POINT('Ctrl Pts',(-25.4828076101654,29.2698007967907,18.));
#26797=CARTESIAN_POINT('Ctrl Pts',(-25.4393679214513,29.183825549991,0.));
#26798=CARTESIAN_POINT('Ctrl Pts',(-25.4393679214513,29.183825549991,18.));
#26799=CARTESIAN_POINT('Ctrl Pts',(-25.3948997321279,29.098589927237,0.));
#26800=CARTESIAN_POINT('Ctrl Pts',(-25.3948997321279,29.098589927237,18.));
#26801=CARTESIAN_POINT('Ctrl Pts',(-25.3493168206005,29.0141637699076,0.));
#26802=CARTESIAN_POINT('Ctrl Pts',(-25.3493168206005,29.0141637699076,18.));
#26803=CARTESIAN_POINT('Ctrl Pts',(-25.3026235249214,28.9305499160476,0.));
#26804=CARTESIAN_POINT('Ctrl Pts',(-25.3026235249214,28.9305499160476,18.));
#26805=CARTESIAN_POINT('Ctrl Pts',(-25.2549775629725,28.8476372998748,0.));
#26806=CARTESIAN_POINT('Ctrl Pts',(-25.2549775629725,28.8476372998748,18.));
#26807=CARTESIAN_POINT('Ctrl Pts',(-25.2066127148845,28.7652594076549,0.));
#26808=CARTESIAN_POINT('Ctrl Pts',(-25.2066127148845,28.7652594076549,18.));
#26809=CARTESIAN_POINT('Ctrl Pts',(-25.1577170374459,28.6832861366762,0.));
#26810=CARTESIAN_POINT('Ctrl Pts',(-25.1577170374459,28.6832861366762,18.));
#26811=CARTESIAN_POINT('Ctrl Pts',(-25.108321158239,28.6017081342376,0.));
#26812=CARTESIAN_POINT('Ctrl Pts',(-25.108321158239,28.6017081342376,18.));
#26813=CARTESIAN_POINT('Ctrl Pts',(-25.0581926620043,28.5207164321473,0.));
#26814=CARTESIAN_POINT('Ctrl Pts',(-25.0581926620043,28.5207164321473,18.));
#26815=CARTESIAN_POINT('Ctrl Pts',(-25.0066999111736,28.4408053900206,0.));
#26816=CARTESIAN_POINT('Ctrl Pts',(-25.0066999111736,28.4408053900206,18.));
#26817=CARTESIAN_POINT('Ctrl Pts',(-24.9529811166897,28.3626431274892,0.));
#26818=CARTESIAN_POINT('Ctrl Pts',(-24.9529811166897,28.3626431274892,18.));
#26819=CARTESIAN_POINT('Ctrl Pts',(-24.9075246543798,28.3020534756061,0.));
#26820=CARTESIAN_POINT('Ctrl Pts',(-24.9075246543798,28.3020534756061,18.));
#26821=CARTESIAN_POINT('Ctrl Pts',(-24.8717258526943,28.2579420132101,0.));
#26822=CARTESIAN_POINT('Ctrl Pts',(-24.8717258526943,28.2579420132101,18.));
#26823=CARTESIAN_POINT('Ctrl Pts',(-24.8470618363541,28.2291563988796,0.));
#26824=CARTESIAN_POINT('Ctrl Pts',(-24.8470618363541,28.2291563988796,18.));
#26825=CARTESIAN_POINT('Ctrl Pts',(-24.8345302882955,28.2149191006269,0.));
#26826=CARTESIAN_POINT('Ctrl Pts',(-24.8345302882955,28.2149191006269,18.));
#26827=CARTESIAN_POINT('',(-26.9738038986839,34.762248247709,0.));
#26828=CARTESIAN_POINT('Ctrl Pts',(-24.8345302882955,28.2149191006269,0.));
#26829=CARTESIAN_POINT('Ctrl Pts',(-24.8470618363541,28.2291563988796,0.));
#26830=CARTESIAN_POINT('Ctrl Pts',(-24.8717258526943,28.2579420132101,0.));
#26831=CARTESIAN_POINT('Ctrl Pts',(-24.9075246543798,28.3020534756061,0.));
#26832=CARTESIAN_POINT('Ctrl Pts',(-24.9529811166897,28.3626431274892,0.));
#26833=CARTESIAN_POINT('Ctrl Pts',(-25.0066999111736,28.4408053900206,0.));
#26834=CARTESIAN_POINT('Ctrl Pts',(-25.0581926620043,28.5207164321473,0.));
#26835=CARTESIAN_POINT('Ctrl Pts',(-25.108321158239,28.6017081342376,0.));
#26836=CARTESIAN_POINT('Ctrl Pts',(-25.1577170374459,28.6832861366762,0.));
#26837=CARTESIAN_POINT('Ctrl Pts',(-25.2066127148845,28.7652594076549,0.));
#26838=CARTESIAN_POINT('Ctrl Pts',(-25.2549775629725,28.8476372998748,0.));
#26839=CARTESIAN_POINT('Ctrl Pts',(-25.3026235249214,28.9305499160476,0.));
#26840=CARTESIAN_POINT('Ctrl Pts',(-25.3493168206005,29.0141637699076,0.));
#26841=CARTESIAN_POINT('Ctrl Pts',(-25.3948997321279,29.098589927237,0.));
#26842=CARTESIAN_POINT('Ctrl Pts',(-25.4393679214513,29.183825549991,0.));
#26843=CARTESIAN_POINT('Ctrl Pts',(-25.4828076101654,29.2698007967907,0.));
#26844=CARTESIAN_POINT('Ctrl Pts',(-25.5253562922582,29.356408021119,0.));
#26845=CARTESIAN_POINT('Ctrl Pts',(-25.5671572096726,29.443535683207,0.));
#26846=CARTESIAN_POINT('Ctrl Pts',(-25.6083094352667,29.5311055094509,0.));
#26847=CARTESIAN_POINT('Ctrl Pts',(-25.6488438125835,29.6190903904157,0.));
#26848=CARTESIAN_POINT('Ctrl Pts',(-25.6887507922748,29.7074935910931,0.));
#26849=CARTESIAN_POINT('Ctrl Pts',(-25.7279973711305,29.7963360859334,0.));
#26850=CARTESIAN_POINT('Ctrl Pts',(-25.7665469042913,29.8856417535786,0.));
#26851=CARTESIAN_POINT('Ctrl Pts',(-25.8043812318214,29.9754208429384,0.));
#26852=CARTESIAN_POINT('Ctrl Pts',(-25.8415089241134,30.0656638016321,0.));
#26853=CARTESIAN_POINT('Ctrl Pts',(-25.8779535511027,30.1563500154165,0.));
#26854=CARTESIAN_POINT('Ctrl Pts',(-25.9137466853317,30.2474530144827,0.));
#26855=CARTESIAN_POINT('Ctrl Pts',(-25.9489196635424,30.3389466074503,0.));
#26856=CARTESIAN_POINT('Ctrl Pts',(-25.9834942765902,30.4308118142473,0.));
#26857=CARTESIAN_POINT('Ctrl Pts',(-26.0174801292225,30.5230388264271,0.));
#26858=CARTESIAN_POINT('Ctrl Pts',(-26.0508796503166,30.6156232634061,0.));
#26859=CARTESIAN_POINT('Ctrl Pts',(-26.0836911730968,30.7085638682391,0.));
#26860=CARTESIAN_POINT('Ctrl Pts',(-26.1159125093178,30.8018598357461,0.));
#26861=CARTESIAN_POINT('Ctrl Pts',(-26.1475450294082,30.8955077633644,0.));
#26862=CARTESIAN_POINT('Ctrl Pts',(-26.1785946616165,30.9895009017073,0.));
#26863=CARTESIAN_POINT('Ctrl Pts',(-26.2090698085494,31.0838307058369,0.));
#26864=CARTESIAN_POINT('Ctrl Pts',(-26.2389800738215,31.1784877826858,0.));
#26865=CARTESIAN_POINT('Ctrl Pts',(-26.2683347859175,31.2734629900041,0.));
#26866=CARTESIAN_POINT('Ctrl Pts',(-26.2971413115295,31.3687486937246,0.));
#26867=CARTESIAN_POINT('Ctrl Pts',(-26.3254046890485,31.4643390378084,0.));
#26868=CARTESIAN_POINT('Ctrl Pts',(-26.353128528169,31.5602292672984,0.));
#26869=CARTESIAN_POINT('Ctrl Pts',(-26.3803155790949,31.6564152990236,0.));
#26870=CARTESIAN_POINT('Ctrl Pts',(-26.4069683862784,31.7528932299312,0.));
#26871=CARTESIAN_POINT('Ctrl Pts',(-26.433090040836,31.849658771403,0.));
#26872=CARTESIAN_POINT('Ctrl Pts',(-26.4586843683627,31.9467071093816,0.));
#26873=CARTESIAN_POINT('Ctrl Pts',(-26.4837555495616,32.0440331917233,0.));
#26874=CARTESIAN_POINT('Ctrl Pts',(-26.5083078928862,32.1416319023705,0.));
#26875=CARTESIAN_POINT('Ctrl Pts',(-26.5323455701117,32.2394982626669,0.));
#26876=CARTESIAN_POINT('Ctrl Pts',(-26.5558723200361,32.3376276606981,0.));
#26877=CARTESIAN_POINT('Ctrl Pts',(-26.5788913672813,32.4360159072985,0.));
#26878=CARTESIAN_POINT('Ctrl Pts',(-26.6014055904817,32.5346590925498,0.));
#26879=CARTESIAN_POINT('Ctrl Pts',(-26.6234176311245,32.6335534898936,0.));
#26880=CARTESIAN_POINT('Ctrl Pts',(-26.6449300199763,32.7326954489334,0.));
#26881=CARTESIAN_POINT('Ctrl Pts',(-26.6659453236976,32.8320812678271,0.));
#26882=CARTESIAN_POINT('Ctrl Pts',(-26.6864661988935,32.9317071576181,0.));
#26883=CARTESIAN_POINT('Ctrl Pts',(-26.7064953106254,33.03156933761,0.));
#26884=CARTESIAN_POINT('Ctrl Pts',(-26.7260352861619,33.131664100194,0.));
#26885=CARTESIAN_POINT('Ctrl Pts',(-26.7450886617884,33.2319878786519,0.));
#26886=CARTESIAN_POINT('Ctrl Pts',(-26.7636578270526,33.3325373307046,0.));
#26887=CARTESIAN_POINT('Ctrl Pts',(-26.7817450041181,33.4333093513694,0.));
#26888=CARTESIAN_POINT('Ctrl Pts',(-26.7993522966985,33.5343009499673,0.));
#26889=CARTESIAN_POINT('Ctrl Pts',(-26.8164817280846,33.6355091508895,0.));
#26890=CARTESIAN_POINT('Ctrl Pts',(-26.8331352836666,33.7369308933173,0.));
#26891=CARTESIAN_POINT('Ctrl Pts',(-26.8493149627661,33.838562905895,0.));
#26892=CARTESIAN_POINT('Ctrl Pts',(-26.8650228056313,33.9404016650487,0.));
#26893=CARTESIAN_POINT('Ctrl Pts',(-26.880260834701,34.0424436187397,0.));
#26894=CARTESIAN_POINT('Ctrl Pts',(-26.8950310138939,34.1446853651051,0.));
#26895=CARTESIAN_POINT('Ctrl Pts',(-26.9093352037262,34.2471238425419,0.));
#26896=CARTESIAN_POINT('Ctrl Pts',(-26.9231751225177,34.3497565255724,0.));
#26897=CARTESIAN_POINT('Ctrl Pts',(-26.9392277420462,34.4731465943772,0.));
#26898=CARTESIAN_POINT('Ctrl Pts',(-26.9520281195268,34.5762105502273,0.));
#26899=CARTESIAN_POINT('Ctrl Pts',(-26.9619003236529,34.6588137898952,0.));
#26900=CARTESIAN_POINT('Ctrl Pts',(-26.9690976283147,34.7208516760814,0.));
#26901=CARTESIAN_POINT('Ctrl Pts',(-26.9738038986838,34.7622482477091,0.));
#26902=CARTESIAN_POINT('',(-26.9738038986839,34.762248247709,15.));
#26903=CARTESIAN_POINT('Ctrl Pts',(-26.9738038986838,34.7622482477091,15.));
#26904=CARTESIAN_POINT('Ctrl Pts',(-26.9714507634923,34.7415499619104,15.));
#26905=CARTESIAN_POINT('Ctrl Pts',(-26.9666985267608,34.700172380686,15.));
#26906=CARTESIAN_POINT('Ctrl Pts',(-26.9594322726214,34.6381629799782,15.));
#26907=CARTESIAN_POINT('Ctrl Pts',(-26.9494680440307,34.5555977590573,15.));
#26908=CARTESIAN_POINT('Ctrl Pts',(-26.9365523054581,34.4525815829097,15.));
#26909=CARTESIAN_POINT('Ctrl Pts',(-26.9231751225177,34.3497565255724,15.));
#26910=CARTESIAN_POINT('Ctrl Pts',(-26.9093352037262,34.2471238425419,15.));
#26911=CARTESIAN_POINT('Ctrl Pts',(-26.8950310138939,34.1446853651051,15.));
#26912=CARTESIAN_POINT('Ctrl Pts',(-26.880260834701,34.0424436187397,15.));
#26913=CARTESIAN_POINT('Ctrl Pts',(-26.8650228056313,33.9404016650487,15.));
#26914=CARTESIAN_POINT('Ctrl Pts',(-26.8493149627661,33.838562905895,15.));
#26915=CARTESIAN_POINT('Ctrl Pts',(-26.8331352836666,33.7369308933173,15.));
#26916=CARTESIAN_POINT('Ctrl Pts',(-26.8164817280846,33.6355091508895,15.));
#26917=CARTESIAN_POINT('Ctrl Pts',(-26.7993522966985,33.5343009499673,15.));
#26918=CARTESIAN_POINT('Ctrl Pts',(-26.7817450041181,33.4333093513694,15.));
#26919=CARTESIAN_POINT('Ctrl Pts',(-26.7636578270526,33.3325373307046,15.));
#26920=CARTESIAN_POINT('Ctrl Pts',(-26.7450886617884,33.2319878786519,15.));
#26921=CARTESIAN_POINT('Ctrl Pts',(-26.7260352861619,33.131664100194,15.));
#26922=CARTESIAN_POINT('Ctrl Pts',(-26.7064953106254,33.03156933761,15.));
#26923=CARTESIAN_POINT('Ctrl Pts',(-26.6864661988935,32.9317071576181,15.));
#26924=CARTESIAN_POINT('Ctrl Pts',(-26.6659453236976,32.8320812678271,15.));
#26925=CARTESIAN_POINT('Ctrl Pts',(-26.6449300199763,32.7326954489334,15.));
#26926=CARTESIAN_POINT('Ctrl Pts',(-26.6234176311245,32.6335534898936,15.));
#26927=CARTESIAN_POINT('Ctrl Pts',(-26.6014055904817,32.5346590925498,15.));
#26928=CARTESIAN_POINT('Ctrl Pts',(-26.5788913672813,32.4360159072985,15.));
#26929=CARTESIAN_POINT('Ctrl Pts',(-26.5558723200361,32.3376276606981,15.));
#26930=CARTESIAN_POINT('Ctrl Pts',(-26.5323455701117,32.2394982626669,15.));
#26931=CARTESIAN_POINT('Ctrl Pts',(-26.5083078928862,32.1416319023705,15.));
#26932=CARTESIAN_POINT('Ctrl Pts',(-26.4837555495616,32.0440331917233,15.));
#26933=CARTESIAN_POINT('Ctrl Pts',(-26.4586843683627,31.9467071093816,15.));
#26934=CARTESIAN_POINT('Ctrl Pts',(-26.433090040836,31.849658771403,15.));
#26935=CARTESIAN_POINT('Ctrl Pts',(-26.4069683862784,31.7528932299312,15.));
#26936=CARTESIAN_POINT('Ctrl Pts',(-26.3803155790949,31.6564152990236,15.));
#26937=CARTESIAN_POINT('Ctrl Pts',(-26.353128528169,31.5602292672984,15.));
#26938=CARTESIAN_POINT('Ctrl Pts',(-26.3254046890485,31.4643390378084,15.));
#26939=CARTESIAN_POINT('Ctrl Pts',(-26.2971413115295,31.3687486937246,15.));
#26940=CARTESIAN_POINT('Ctrl Pts',(-26.2683347859175,31.2734629900041,15.));
#26941=CARTESIAN_POINT('Ctrl Pts',(-26.2389800738215,31.1784877826858,15.));
#26942=CARTESIAN_POINT('Ctrl Pts',(-26.2090698085494,31.0838307058369,15.));
#26943=CARTESIAN_POINT('Ctrl Pts',(-26.1785946616165,30.9895009017073,15.));
#26944=CARTESIAN_POINT('Ctrl Pts',(-26.1475450294082,30.8955077633644,15.));
#26945=CARTESIAN_POINT('Ctrl Pts',(-26.1159125093178,30.8018598357461,15.));
#26946=CARTESIAN_POINT('Ctrl Pts',(-26.0836911730968,30.7085638682391,15.));
#26947=CARTESIAN_POINT('Ctrl Pts',(-26.0508796503166,30.6156232634061,15.));
#26948=CARTESIAN_POINT('Ctrl Pts',(-26.0174801292225,30.5230388264271,15.));
#26949=CARTESIAN_POINT('Ctrl Pts',(-25.9834942765902,30.4308118142473,15.));
#26950=CARTESIAN_POINT('Ctrl Pts',(-25.9489196635424,30.3389466074503,15.));
#26951=CARTESIAN_POINT('Ctrl Pts',(-25.9137466853317,30.2474530144827,15.));
#26952=CARTESIAN_POINT('Ctrl Pts',(-25.8779535511027,30.1563500154165,15.));
#26953=CARTESIAN_POINT('Ctrl Pts',(-25.8415089241134,30.0656638016321,15.));
#26954=CARTESIAN_POINT('Ctrl Pts',(-25.8043812318214,29.9754208429384,15.));
#26955=CARTESIAN_POINT('Ctrl Pts',(-25.7665469042913,29.8856417535786,15.));
#26956=CARTESIAN_POINT('Ctrl Pts',(-25.7279973711305,29.7963360859334,15.));
#26957=CARTESIAN_POINT('Ctrl Pts',(-25.6887507922748,29.7074935910931,15.));
#26958=CARTESIAN_POINT('Ctrl Pts',(-25.6488438125835,29.6190903904157,15.));
#26959=CARTESIAN_POINT('Ctrl Pts',(-25.6083094352667,29.5311055094509,15.));
#26960=CARTESIAN_POINT('Ctrl Pts',(-25.5671572096726,29.443535683207,15.));
#26961=CARTESIAN_POINT('Ctrl Pts',(-25.5253562922582,29.356408021119,15.));
#26962=CARTESIAN_POINT('Ctrl Pts',(-25.4828076101654,29.2698007967907,15.));
#26963=CARTESIAN_POINT('Ctrl Pts',(-25.4393679214513,29.183825549991,15.));
#26964=CARTESIAN_POINT('Ctrl Pts',(-25.3948997321279,29.098589927237,15.));
#26965=CARTESIAN_POINT('Ctrl Pts',(-25.3493168206005,29.0141637699076,15.));
#26966=CARTESIAN_POINT('Ctrl Pts',(-25.3026235249214,28.9305499160476,15.));
#26967=CARTESIAN_POINT('Ctrl Pts',(-25.2549775629725,28.8476372998748,15.));
#26968=CARTESIAN_POINT('Ctrl Pts',(-25.2066127148845,28.7652594076549,15.));
#26969=CARTESIAN_POINT('Ctrl Pts',(-25.1577170374459,28.6832861366762,15.));
#26970=CARTESIAN_POINT('Ctrl Pts',(-25.108321158239,28.6017081342376,15.));
#26971=CARTESIAN_POINT('Ctrl Pts',(-25.0581926620043,28.5207164321473,15.));
#26972=CARTESIAN_POINT('Ctrl Pts',(-25.0066999111736,28.4408053900206,15.));
#26973=CARTESIAN_POINT('Ctrl Pts',(-24.9529811166897,28.3626431274892,15.));
#26974=CARTESIAN_POINT('Ctrl Pts',(-24.9075246543798,28.3020534756061,15.));
#26975=CARTESIAN_POINT('Ctrl Pts',(-24.8717258526943,28.2579420132101,15.));
#26976=CARTESIAN_POINT('Ctrl Pts',(-24.8470618363541,28.2291563988796,15.));
#26977=CARTESIAN_POINT('Ctrl Pts',(-24.8345302882955,28.2149191006269,15.));
#26978=CARTESIAN_POINT('',(-26.9738038986839,34.762248247709,0.));
#26979=CARTESIAN_POINT('Origin',(-6.66146233219319E-12,9.16871631793044E-12,
0.));
#26980=CARTESIAN_POINT('',(-24.725498909423,36.3957374383337,0.));
#26981=CARTESIAN_POINT('Origin',(-6.66146233219319E-12,9.16871631793044E-12,
0.));
#26982=CARTESIAN_POINT('',(-24.725498909423,36.3957374383337,15.));
#26983=CARTESIAN_POINT('Origin',(-6.66146233219319E-12,9.16871631793044E-12,
15.));
#26984=CARTESIAN_POINT('',(-24.725498909423,36.3957374383337,0.));
#26985=CARTESIAN_POINT('Ctrl Pts',(-19.1596907609891,32.3379313568208,0.));
#26986=CARTESIAN_POINT('Ctrl Pts',(-19.1596907609891,32.3379313568208,18.));
#26987=CARTESIAN_POINT('Ctrl Pts',(-19.1693587749508,32.3542491343753,0.));
#26988=CARTESIAN_POINT('Ctrl Pts',(-19.1693587749508,32.3542491343753,18.));
#26989=CARTESIAN_POINT('Ctrl Pts',(-19.1891139208368,32.3866012518553,0.));
#26990=CARTESIAN_POINT('Ctrl Pts',(-19.1891139208368,32.3866012518553,18.));
#26991=CARTESIAN_POINT('Ctrl Pts',(-19.2200039764927,32.4342791270009,0.));
#26992=CARTESIAN_POINT('Ctrl Pts',(-19.2200039764927,32.4342791270009,18.));
#26993=CARTESIAN_POINT('Ctrl Pts',(-19.2635813403783,32.4962340238036,0.));
#26994=CARTESIAN_POINT('Ctrl Pts',(-19.2635813403783,32.4962340238036,18.));
#26995=CARTESIAN_POINT('Ctrl Pts',(-19.3213180490743,32.5714771007861,0.));
#26996=CARTESIAN_POINT('Ctrl Pts',(-19.3213180490743,32.5714771007861,18.));
#26997=CARTESIAN_POINT('Ctrl Pts',(-19.381405831319,32.6451434870609,0.));
#26998=CARTESIAN_POINT('Ctrl Pts',(-19.381405831319,32.6451434870609,18.));
#26999=CARTESIAN_POINT('Ctrl Pts',(-19.4429429601189,32.7178463324062,0.));
#27000=CARTESIAN_POINT('Ctrl Pts',(-19.4429429601189,32.7178463324062,18.));
#27001=CARTESIAN_POINT('Ctrl Pts',(-19.5052640847974,32.7900335943248,0.));
#27002=CARTESIAN_POINT('Ctrl Pts',(-19.5052640847974,32.7900335943248,18.));
#27003=CARTESIAN_POINT('Ctrl Pts',(-19.5681157030437,32.8618672807884,0.));
#27004=CARTESIAN_POINT('Ctrl Pts',(-19.5681157030437,32.8618672807884,18.));
#27005=CARTESIAN_POINT('Ctrl Pts',(-19.6315161742485,32.9333211533788,0.));
#27006=CARTESIAN_POINT('Ctrl Pts',(-19.6315161742485,32.9333211533788,18.));
#27007=CARTESIAN_POINT('Ctrl Pts',(-19.6956473461873,33.004256563411,0.));
#27008=CARTESIAN_POINT('Ctrl Pts',(-19.6956473461873,33.004256563411,18.));
#27009=CARTESIAN_POINT('Ctrl Pts',(-19.7607398248651,33.0745026283418,0.));
#27010=CARTESIAN_POINT('Ctrl Pts',(-19.7607398248651,33.0745026283418,18.));
#27011=CARTESIAN_POINT('Ctrl Pts',(-19.8269479776239,33.1439436707661,0.));
#27012=CARTESIAN_POINT('Ctrl Pts',(-19.8269479776239,33.1439436707661,18.));
#27013=CARTESIAN_POINT('Ctrl Pts',(-19.8942704458546,33.2125746879472,0.));
#27014=CARTESIAN_POINT('Ctrl Pts',(-19.8942704458546,33.2125746879472,18.));
#27015=CARTESIAN_POINT('Ctrl Pts',(-19.9626141625205,33.2804560993213,0.));
#27016=CARTESIAN_POINT('Ctrl Pts',(-19.9626141625205,33.2804560993213,18.));
#27017=CARTESIAN_POINT('Ctrl Pts',(-20.0318342617212,33.3476854048385,0.));
#27018=CARTESIAN_POINT('Ctrl Pts',(-20.0318342617212,33.3476854048385,18.));
#27019=CARTESIAN_POINT('Ctrl Pts',(-20.1017803986381,33.4143643679979,0.));
#27020=CARTESIAN_POINT('Ctrl Pts',(-20.1017803986381,33.4143643679979,18.));
#27021=CARTESIAN_POINT('Ctrl Pts',(-20.1723475154533,33.480563024813,0.));
#27022=CARTESIAN_POINT('Ctrl Pts',(-20.1723475154533,33.480563024813,18.));
#27023=CARTESIAN_POINT('Ctrl Pts',(-20.243500298383,33.5463023319603,0.));
#27024=CARTESIAN_POINT('Ctrl Pts',(-20.243500298383,33.5463023319603,18.));
#27025=CARTESIAN_POINT('Ctrl Pts',(-20.3152448035298,33.6115742164079,0.));
#27026=CARTESIAN_POINT('Ctrl Pts',(-20.3152448035298,33.6115742164079,18.));
#27027=CARTESIAN_POINT('Ctrl Pts',(-20.3876111773341,33.6763537716992,0.));
#27028=CARTESIAN_POINT('Ctrl Pts',(-20.3876111773341,33.6763537716992,18.));
#27029=CARTESIAN_POINT('Ctrl Pts',(-20.4606334536183,33.7406135254083,0.));
#27030=CARTESIAN_POINT('Ctrl Pts',(-20.4606334536183,33.7406135254083,18.));
#27031=CARTESIAN_POINT('Ctrl Pts',(-20.5343269914034,33.8043393734971,0.));
#27032=CARTESIAN_POINT('Ctrl Pts',(-20.5343269914034,33.8043393734971,18.));
#27033=CARTESIAN_POINT('Ctrl Pts',(-20.6086800574386,33.8675365150454,0.));
#27034=CARTESIAN_POINT('Ctrl Pts',(-20.6086800574386,33.8675365150454,18.));
#27035=CARTESIAN_POINT('Ctrl Pts',(-20.683665762903,33.9302209962425,0.));
#27036=CARTESIAN_POINT('Ctrl Pts',(-20.683665762903,33.9302209962425,18.));
#27037=CARTESIAN_POINT('Ctrl Pts',(-20.7592491770603,33.9924146647395,0.));
#27038=CARTESIAN_POINT('Ctrl Pts',(-20.7592491770603,33.9924146647395,18.));
#27039=CARTESIAN_POINT('Ctrl Pts',(-20.8353957068415,34.0541392299678,0.));
#27040=CARTESIAN_POINT('Ctrl Pts',(-20.8353957068415,34.0541392299678,18.));
#27041=CARTESIAN_POINT('Ctrl Pts',(-20.9120805673809,34.1154095510973,0.));
#27042=CARTESIAN_POINT('Ctrl Pts',(-20.9120805673809,34.1154095510973,18.));
#27043=CARTESIAN_POINT('Ctrl Pts',(-20.9892914622612,34.176231731809,0.));
#27044=CARTESIAN_POINT('Ctrl Pts',(-20.9892914622612,34.176231731809,18.));
#27045=CARTESIAN_POINT('Ctrl Pts',(-21.0670234747355,34.2366067284279,0.));
#27046=CARTESIAN_POINT('Ctrl Pts',(-21.0670234747355,34.2366067284279,18.));
#27047=CARTESIAN_POINT('Ctrl Pts',(-21.1452759244399,34.2965325673384,0.));
#27048=CARTESIAN_POINT('Ctrl Pts',(-21.1452759244399,34.2965325673384,18.));
#27049=CARTESIAN_POINT('Ctrl Pts',(-21.2240487218079,34.3560069185815,0.));
#27050=CARTESIAN_POINT('Ctrl Pts',(-21.2240487218079,34.3560069185815,18.));
#27051=CARTESIAN_POINT('Ctrl Pts',(-21.3033382073239,34.4150300340623,0.));
#27052=CARTESIAN_POINT('Ctrl Pts',(-21.3033382073239,34.4150300340623,18.));
#27053=CARTESIAN_POINT('Ctrl Pts',(-21.3831361300104,34.4736054662052,0.));
#27054=CARTESIAN_POINT('Ctrl Pts',(-21.3831361300104,34.4736054662052,18.));
#27055=CARTESIAN_POINT('Ctrl Pts',(-21.4634317666005,34.5317385658329,0.));
#27056=CARTESIAN_POINT('Ctrl Pts',(-21.4634317666005,34.5317385658329,18.));
#27057=CARTESIAN_POINT('Ctrl Pts',(-21.5442132160757,34.5894355639082,0.));
#27058=CARTESIAN_POINT('Ctrl Pts',(-21.5442132160757,34.5894355639082,18.));
#27059=CARTESIAN_POINT('Ctrl Pts',(-21.6254689009796,34.6467025072367,0.));
#27060=CARTESIAN_POINT('Ctrl Pts',(-21.6254689009796,34.6467025072367,18.));
#27061=CARTESIAN_POINT('Ctrl Pts',(-21.7071892844497,34.7035440429025,0.));
#27062=CARTESIAN_POINT('Ctrl Pts',(-21.7071892844497,34.7035440429025,18.));
#27063=CARTESIAN_POINT('Ctrl Pts',(-21.7893672401137,34.7599631530844,0.));
#27064=CARTESIAN_POINT('Ctrl Pts',(-21.7893672401137,34.7599631530844,18.));
#27065=CARTESIAN_POINT('Ctrl Pts',(-21.8719971302817,34.8159618014436,0.));
#27066=CARTESIAN_POINT('Ctrl Pts',(-21.8719971302817,34.8159618014436,18.));
#27067=CARTESIAN_POINT('Ctrl Pts',(-21.9550742217675,34.8715413418101,0.));
#27068=CARTESIAN_POINT('Ctrl Pts',(-21.9550742217675,34.8715413418101,18.));
#27069=CARTESIAN_POINT('Ctrl Pts',(-22.0385940162683,34.9267029879922,0.));
#27070=CARTESIAN_POINT('Ctrl Pts',(-22.0385940162683,34.9267029879922,18.));
#27071=CARTESIAN_POINT('Ctrl Pts',(-22.1225514798584,34.9814483545602,0.));
#27072=CARTESIAN_POINT('Ctrl Pts',(-22.1225514798584,34.9814483545602,18.));
#27073=CARTESIAN_POINT('Ctrl Pts',(-22.2069408519232,35.0357795922459,0.));
#27074=CARTESIAN_POINT('Ctrl Pts',(-22.2069408519232,35.0357795922459,18.));
#27075=CARTESIAN_POINT('Ctrl Pts',(-22.2917560356803,35.0896991159359,0.));
#27076=CARTESIAN_POINT('Ctrl Pts',(-22.2917560356803,35.0896991159359,18.));
#27077=CARTESIAN_POINT('Ctrl Pts',(-22.3769908340843,35.1432094422642,0.));
#27078=CARTESIAN_POINT('Ctrl Pts',(-22.3769908340843,35.1432094422642,18.));
#27079=CARTESIAN_POINT('Ctrl Pts',(-22.4626392230023,35.1963130003352,0.));
#27080=CARTESIAN_POINT('Ctrl Pts',(-22.4626392230023,35.1963130003352,18.));
#27081=CARTESIAN_POINT('Ctrl Pts',(-22.5486956608909,35.2490119207975,0.));
#27082=CARTESIAN_POINT('Ctrl Pts',(-22.5486956608909,35.2490119207975,18.));
#27083=CARTESIAN_POINT('Ctrl Pts',(-22.635155167154,35.3013079759252,0.));
#27084=CARTESIAN_POINT('Ctrl Pts',(-22.635155167154,35.3013079759252,18.));
#27085=CARTESIAN_POINT('Ctrl Pts',(-22.7220131336912,35.3532026952313,0.));
#27086=CARTESIAN_POINT('Ctrl Pts',(-22.7220131336912,35.3532026952313,18.));
#27087=CARTESIAN_POINT('Ctrl Pts',(-22.8092652000706,35.4046974393492,0.));
#27088=CARTESIAN_POINT('Ctrl Pts',(-22.8092652000706,35.4046974393492,18.));
#27089=CARTESIAN_POINT('Ctrl Pts',(-22.8969071125089,35.4557934871468,0.));
#27090=CARTESIAN_POINT('Ctrl Pts',(-22.8969071125089,35.4557934871468,18.));
#27091=CARTESIAN_POINT('Ctrl Pts',(-22.9849345572033,35.5064921357308,0.));
#27092=CARTESIAN_POINT('Ctrl Pts',(-22.9849345572033,35.5064921357308,18.));
#27093=CARTESIAN_POINT('Ctrl Pts',(-23.0733431097058,35.5567947408311,0.));
#27094=CARTESIAN_POINT('Ctrl Pts',(-23.0733431097058,35.5567947408311,18.));
#27095=CARTESIAN_POINT('Ctrl Pts',(-23.1621283508111,35.6067026687722,0.));
#27096=CARTESIAN_POINT('Ctrl Pts',(-23.1621283508111,35.6067026687722,18.));
#27097=CARTESIAN_POINT('Ctrl Pts',(-23.2512859425032,35.6562172725207,0.));
#27098=CARTESIAN_POINT('Ctrl Pts',(-23.2512859425032,35.6562172725207,18.));
#27099=CARTESIAN_POINT('Ctrl Pts',(-23.3408117088761,35.7053398620512,0.));
#27100=CARTESIAN_POINT('Ctrl Pts',(-23.3408117088761,35.7053398620512,18.));
#27101=CARTESIAN_POINT('Ctrl Pts',(-23.4307017328227,35.7540716771372,0.));
#27102=CARTESIAN_POINT('Ctrl Pts',(-23.4307017328227,35.7540716771372,18.));
#27103=CARTESIAN_POINT('Ctrl Pts',(-23.5209523746427,35.8024138716897,0.));
#27104=CARTESIAN_POINT('Ctrl Pts',(-23.5209523746427,35.8024138716897,18.));
#27105=CARTESIAN_POINT('Ctrl Pts',(-23.611560139948,35.8503675222885,0.));
#27106=CARTESIAN_POINT('Ctrl Pts',(-23.611560139948,35.8503675222885,18.));
#27107=CARTESIAN_POINT('Ctrl Pts',(-23.7025215735353,35.8979336336837,0.));
#27108=CARTESIAN_POINT('Ctrl Pts',(-23.7025215735353,35.8979336336837,18.));
#27109=CARTESIAN_POINT('Ctrl Pts',(-23.7938331508737,35.9451131482488,0.));
#27110=CARTESIAN_POINT('Ctrl Pts',(-23.7938331508737,35.9451131482488,18.));
#27111=CARTESIAN_POINT('Ctrl Pts',(-23.8854911428946,35.991906956547,0.));
#27112=CARTESIAN_POINT('Ctrl Pts',(-23.8854911428946,35.991906956547,18.));
#27113=CARTESIAN_POINT('Ctrl Pts',(-23.9774915680089,36.0383159101254,0.));
#27114=CARTESIAN_POINT('Ctrl Pts',(-23.9774915680089,36.0383159101254,18.));
#27115=CARTESIAN_POINT('Ctrl Pts',(-24.0698304230588,36.0843408347974,0.));
#27116=CARTESIAN_POINT('Ctrl Pts',(-24.0698304230588,36.0843408347974,18.));
#27117=CARTESIAN_POINT('Ctrl Pts',(-24.1625038657964,36.1299825471271,0.));
#27118=CARTESIAN_POINT('Ctrl Pts',(-24.1625038657964,36.1299825471271,18.));
#27119=CARTESIAN_POINT('Ctrl Pts',(-24.2555084095332,36.1752418704833,0.));
#27120=CARTESIAN_POINT('Ctrl Pts',(-24.2555084095332,36.1752418704833,18.));
#27121=CARTESIAN_POINT('Ctrl Pts',(-24.3488411214068,36.2201196586697,0.));
#27122=CARTESIAN_POINT('Ctrl Pts',(-24.3488411214068,36.2201196586697,18.));
#27123=CARTESIAN_POINT('Ctrl Pts',(-24.4424997853605,36.2646168058396,0.));
#27124=CARTESIAN_POINT('Ctrl Pts',(-24.4424997853605,36.2646168058396,18.));
#27125=CARTESIAN_POINT('Ctrl Pts',(-24.5364828082556,36.308734152297,0.));
#27126=CARTESIAN_POINT('Ctrl Pts',(-24.5364828082556,36.308734152297,18.));
#27127=CARTESIAN_POINT('Ctrl Pts',(-24.6119278836614,36.3437247532369,0.));
#27128=CARTESIAN_POINT('Ctrl Pts',(-24.6119278836614,36.3437247532369,18.));
#27129=CARTESIAN_POINT('Ctrl Pts',(-24.6686569322616,36.369797330215,0.));
#27130=CARTESIAN_POINT('Ctrl Pts',(-24.6686569322616,36.369797330215,18.));
#27131=CARTESIAN_POINT('Ctrl Pts',(-24.7065408286023,36.3871033517098,0.));
#27132=CARTESIAN_POINT('Ctrl Pts',(-24.7065408286023,36.3871033517098,18.));
#27133=CARTESIAN_POINT('Ctrl Pts',(-24.725498909423,36.3957374383337,0.));
#27134=CARTESIAN_POINT('Ctrl Pts',(-24.725498909423,36.3957374383337,18.));
#27135=CARTESIAN_POINT('Ctrl Pts',(-19.1596907609891,32.3379313568208,0.));
#27136=CARTESIAN_POINT('Ctrl Pts',(-19.1693587749508,32.3542491343753,0.));
#27137=CARTESIAN_POINT('Ctrl Pts',(-19.1891139208368,32.3866012518553,0.));
#27138=CARTESIAN_POINT('Ctrl Pts',(-19.2200039764927,32.4342791270009,0.));
#27139=CARTESIAN_POINT('Ctrl Pts',(-19.2635813403783,32.4962340238036,0.));
#27140=CARTESIAN_POINT('Ctrl Pts',(-19.3213180490743,32.5714771007861,0.));
#27141=CARTESIAN_POINT('Ctrl Pts',(-19.381405831319,32.6451434870609,0.));
#27142=CARTESIAN_POINT('Ctrl Pts',(-19.4429429601189,32.7178463324062,0.));
#27143=CARTESIAN_POINT('Ctrl Pts',(-19.5052640847974,32.7900335943248,0.));
#27144=CARTESIAN_POINT('Ctrl Pts',(-19.5681157030437,32.8618672807884,0.));
#27145=CARTESIAN_POINT('Ctrl Pts',(-19.6315161742485,32.9333211533788,0.));
#27146=CARTESIAN_POINT('Ctrl Pts',(-19.6956473461873,33.004256563411,0.));
#27147=CARTESIAN_POINT('Ctrl Pts',(-19.7607398248651,33.0745026283418,0.));
#27148=CARTESIAN_POINT('Ctrl Pts',(-19.8269479776239,33.1439436707661,0.));
#27149=CARTESIAN_POINT('Ctrl Pts',(-19.8942704458546,33.2125746879472,0.));
#27150=CARTESIAN_POINT('Ctrl Pts',(-19.9626141625205,33.2804560993213,0.));
#27151=CARTESIAN_POINT('Ctrl Pts',(-20.0318342617212,33.3476854048385,0.));
#27152=CARTESIAN_POINT('Ctrl Pts',(-20.1017803986381,33.4143643679979,0.));
#27153=CARTESIAN_POINT('Ctrl Pts',(-20.1723475154533,33.480563024813,0.));
#27154=CARTESIAN_POINT('Ctrl Pts',(-20.243500298383,33.5463023319603,0.));
#27155=CARTESIAN_POINT('Ctrl Pts',(-20.3152448035298,33.6115742164079,0.));
#27156=CARTESIAN_POINT('Ctrl Pts',(-20.3876111773341,33.6763537716992,0.));
#27157=CARTESIAN_POINT('Ctrl Pts',(-20.4606334536183,33.7406135254083,0.));
#27158=CARTESIAN_POINT('Ctrl Pts',(-20.5343269914034,33.8043393734971,0.));
#27159=CARTESIAN_POINT('Ctrl Pts',(-20.6086800574386,33.8675365150454,0.));
#27160=CARTESIAN_POINT('Ctrl Pts',(-20.683665762903,33.9302209962425,0.));
#27161=CARTESIAN_POINT('Ctrl Pts',(-20.7592491770603,33.9924146647395,0.));
#27162=CARTESIAN_POINT('Ctrl Pts',(-20.8353957068415,34.0541392299678,0.));
#27163=CARTESIAN_POINT('Ctrl Pts',(-20.9120805673809,34.1154095510973,0.));
#27164=CARTESIAN_POINT('Ctrl Pts',(-20.9892914622612,34.176231731809,0.));
#27165=CARTESIAN_POINT('Ctrl Pts',(-21.0670234747355,34.2366067284279,0.));
#27166=CARTESIAN_POINT('Ctrl Pts',(-21.1452759244399,34.2965325673384,0.));
#27167=CARTESIAN_POINT('Ctrl Pts',(-21.2240487218079,34.3560069185815,0.));
#27168=CARTESIAN_POINT('Ctrl Pts',(-21.3033382073239,34.4150300340623,0.));
#27169=CARTESIAN_POINT('Ctrl Pts',(-21.3831361300104,34.4736054662052,0.));
#27170=CARTESIAN_POINT('Ctrl Pts',(-21.4634317666005,34.5317385658329,0.));
#27171=CARTESIAN_POINT('Ctrl Pts',(-21.5442132160757,34.5894355639082,0.));
#27172=CARTESIAN_POINT('Ctrl Pts',(-21.6254689009796,34.6467025072367,0.));
#27173=CARTESIAN_POINT('Ctrl Pts',(-21.7071892844497,34.7035440429025,0.));
#27174=CARTESIAN_POINT('Ctrl Pts',(-21.7893672401137,34.7599631530844,0.));
#27175=CARTESIAN_POINT('Ctrl Pts',(-21.8719971302817,34.8159618014436,0.));
#27176=CARTESIAN_POINT('Ctrl Pts',(-21.9550742217675,34.8715413418101,0.));
#27177=CARTESIAN_POINT('Ctrl Pts',(-22.0385940162683,34.9267029879922,0.));
#27178=CARTESIAN_POINT('Ctrl Pts',(-22.1225514798584,34.9814483545602,0.));
#27179=CARTESIAN_POINT('Ctrl Pts',(-22.2069408519232,35.0357795922459,0.));
#27180=CARTESIAN_POINT('Ctrl Pts',(-22.2917560356803,35.0896991159359,0.));
#27181=CARTESIAN_POINT('Ctrl Pts',(-22.3769908340843,35.1432094422642,0.));
#27182=CARTESIAN_POINT('Ctrl Pts',(-22.4626392230023,35.1963130003352,0.));
#27183=CARTESIAN_POINT('Ctrl Pts',(-22.5486956608909,35.2490119207975,0.));
#27184=CARTESIAN_POINT('Ctrl Pts',(-22.635155167154,35.3013079759252,0.));
#27185=CARTESIAN_POINT('Ctrl Pts',(-22.7220131336912,35.3532026952313,0.));
#27186=CARTESIAN_POINT('Ctrl Pts',(-22.8092652000706,35.4046974393492,0.));
#27187=CARTESIAN_POINT('Ctrl Pts',(-22.8969071125089,35.4557934871468,0.));
#27188=CARTESIAN_POINT('Ctrl Pts',(-22.9849345572033,35.5064921357308,0.));
#27189=CARTESIAN_POINT('Ctrl Pts',(-23.0733431097058,35.5567947408311,0.));
#27190=CARTESIAN_POINT('Ctrl Pts',(-23.1621283508111,35.6067026687722,0.));
#27191=CARTESIAN_POINT('Ctrl Pts',(-23.2512859425032,35.6562172725207,0.));
#27192=CARTESIAN_POINT('Ctrl Pts',(-23.3408117088761,35.7053398620512,0.));
#27193=CARTESIAN_POINT('Ctrl Pts',(-23.4307017328227,35.7540716771372,0.));
#27194=CARTESIAN_POINT('Ctrl Pts',(-23.5209523746427,35.8024138716897,0.));
#27195=CARTESIAN_POINT('Ctrl Pts',(-23.611560139948,35.8503675222885,0.));
#27196=CARTESIAN_POINT('Ctrl Pts',(-23.7025215735353,35.8979336336837,0.));
#27197=CARTESIAN_POINT('Ctrl Pts',(-23.7938331508737,35.9451131482488,0.));
#27198=CARTESIAN_POINT('Ctrl Pts',(-23.8854911428946,35.991906956547,0.));
#27199=CARTESIAN_POINT('Ctrl Pts',(-23.9774915680089,36.0383159101254,0.));
#27200=CARTESIAN_POINT('Ctrl Pts',(-24.0698304230588,36.0843408347974,0.));
#27201=CARTESIAN_POINT('Ctrl Pts',(-24.1625038657964,36.1299825471271,0.));
#27202=CARTESIAN_POINT('Ctrl Pts',(-24.2555084095332,36.1752418704833,0.));
#27203=CARTESIAN_POINT('Ctrl Pts',(-24.3488411214068,36.2201196586697,0.));
#27204=CARTESIAN_POINT('Ctrl Pts',(-24.4612315181512,36.2735162352736,0.));
#27205=CARTESIAN_POINT('Ctrl Pts',(-24.5552956307817,36.3175386315529,0.));
#27206=CARTESIAN_POINT('Ctrl Pts',(-24.630805301288,36.3524534604649,0.));
#27207=CARTESIAN_POINT('Ctrl Pts',(-24.6875827477484,36.37846926509,0.));
#27208=CARTESIAN_POINT('Ctrl Pts',(-24.725498909423,36.3957374383337,0.));
#27209=CARTESIAN_POINT('Ctrl Pts',(-19.1596907609891,32.3379313568208,15.));
#27210=CARTESIAN_POINT('Ctrl Pts',(-19.1693587749508,32.3542491343753,15.));
#27211=CARTESIAN_POINT('Ctrl Pts',(-19.1891139208368,32.3866012518553,15.));
#27212=CARTESIAN_POINT('Ctrl Pts',(-19.2200039764927,32.4342791270009,15.));
#27213=CARTESIAN_POINT('Ctrl Pts',(-19.2635813403783,32.4962340238036,15.));
#27214=CARTESIAN_POINT('Ctrl Pts',(-19.3213180490743,32.5714771007861,15.));
#27215=CARTESIAN_POINT('Ctrl Pts',(-19.381405831319,32.6451434870609,15.));
#27216=CARTESIAN_POINT('Ctrl Pts',(-19.4429429601189,32.7178463324062,15.));
#27217=CARTESIAN_POINT('Ctrl Pts',(-19.5052640847974,32.7900335943248,15.));
#27218=CARTESIAN_POINT('Ctrl Pts',(-19.5681157030437,32.8618672807884,15.));
#27219=CARTESIAN_POINT('Ctrl Pts',(-19.6315161742485,32.9333211533788,15.));
#27220=CARTESIAN_POINT('Ctrl Pts',(-19.6956473461873,33.004256563411,15.));
#27221=CARTESIAN_POINT('Ctrl Pts',(-19.7607398248651,33.0745026283418,15.));
#27222=CARTESIAN_POINT('Ctrl Pts',(-19.8269479776239,33.1439436707661,15.));
#27223=CARTESIAN_POINT('Ctrl Pts',(-19.8942704458546,33.2125746879472,15.));
#27224=CARTESIAN_POINT('Ctrl Pts',(-19.9626141625205,33.2804560993213,15.));
#27225=CARTESIAN_POINT('Ctrl Pts',(-20.0318342617212,33.3476854048385,15.));
#27226=CARTESIAN_POINT('Ctrl Pts',(-20.1017803986381,33.4143643679979,15.));
#27227=CARTESIAN_POINT('Ctrl Pts',(-20.1723475154533,33.480563024813,15.));
#27228=CARTESIAN_POINT('Ctrl Pts',(-20.243500298383,33.5463023319603,15.));
#27229=CARTESIAN_POINT('Ctrl Pts',(-20.3152448035298,33.6115742164079,15.));
#27230=CARTESIAN_POINT('Ctrl Pts',(-20.3876111773341,33.6763537716992,15.));
#27231=CARTESIAN_POINT('Ctrl Pts',(-20.4606334536183,33.7406135254083,15.));
#27232=CARTESIAN_POINT('Ctrl Pts',(-20.5343269914034,33.8043393734971,15.));
#27233=CARTESIAN_POINT('Ctrl Pts',(-20.6086800574386,33.8675365150454,15.));
#27234=CARTESIAN_POINT('Ctrl Pts',(-20.683665762903,33.9302209962425,15.));
#27235=CARTESIAN_POINT('Ctrl Pts',(-20.7592491770603,33.9924146647395,15.));
#27236=CARTESIAN_POINT('Ctrl Pts',(-20.8353957068415,34.0541392299678,15.));
#27237=CARTESIAN_POINT('Ctrl Pts',(-20.9120805673809,34.1154095510973,15.));
#27238=CARTESIAN_POINT('Ctrl Pts',(-20.9892914622612,34.176231731809,15.));
#27239=CARTESIAN_POINT('Ctrl Pts',(-21.0670234747355,34.2366067284279,15.));
#27240=CARTESIAN_POINT('Ctrl Pts',(-21.1452759244399,34.2965325673384,15.));
#27241=CARTESIAN_POINT('Ctrl Pts',(-21.2240487218079,34.3560069185815,15.));
#27242=CARTESIAN_POINT('Ctrl Pts',(-21.3033382073239,34.4150300340623,15.));
#27243=CARTESIAN_POINT('Ctrl Pts',(-21.3831361300104,34.4736054662052,15.));
#27244=CARTESIAN_POINT('Ctrl Pts',(-21.4634317666005,34.5317385658329,15.));
#27245=CARTESIAN_POINT('Ctrl Pts',(-21.5442132160757,34.5894355639082,15.));
#27246=CARTESIAN_POINT('Ctrl Pts',(-21.6254689009796,34.6467025072367,15.));
#27247=CARTESIAN_POINT('Ctrl Pts',(-21.7071892844497,34.7035440429025,15.));
#27248=CARTESIAN_POINT('Ctrl Pts',(-21.7893672401137,34.7599631530844,15.));
#27249=CARTESIAN_POINT('Ctrl Pts',(-21.8719971302817,34.8159618014436,15.));
#27250=CARTESIAN_POINT('Ctrl Pts',(-21.9550742217675,34.8715413418101,15.));
#27251=CARTESIAN_POINT('Ctrl Pts',(-22.0385940162683,34.9267029879922,15.));
#27252=CARTESIAN_POINT('Ctrl Pts',(-22.1225514798584,34.9814483545602,15.));
#27253=CARTESIAN_POINT('Ctrl Pts',(-22.2069408519232,35.0357795922459,15.));
#27254=CARTESIAN_POINT('Ctrl Pts',(-22.2917560356803,35.0896991159359,15.));
#27255=CARTESIAN_POINT('Ctrl Pts',(-22.3769908340843,35.1432094422642,15.));
#27256=CARTESIAN_POINT('Ctrl Pts',(-22.4626392230023,35.1963130003352,15.));
#27257=CARTESIAN_POINT('Ctrl Pts',(-22.5486956608909,35.2490119207975,15.));
#27258=CARTESIAN_POINT('Ctrl Pts',(-22.635155167154,35.3013079759252,15.));
#27259=CARTESIAN_POINT('Ctrl Pts',(-22.7220131336912,35.3532026952313,15.));
#27260=CARTESIAN_POINT('Ctrl Pts',(-22.8092652000706,35.4046974393492,15.));
#27261=CARTESIAN_POINT('Ctrl Pts',(-22.8969071125089,35.4557934871468,15.));
#27262=CARTESIAN_POINT('Ctrl Pts',(-22.9849345572033,35.5064921357308,15.));
#27263=CARTESIAN_POINT('Ctrl Pts',(-23.0733431097058,35.5567947408311,15.));
#27264=CARTESIAN_POINT('Ctrl Pts',(-23.1621283508111,35.6067026687722,15.));
#27265=CARTESIAN_POINT('Ctrl Pts',(-23.2512859425032,35.6562172725207,15.));
#27266=CARTESIAN_POINT('Ctrl Pts',(-23.3408117088761,35.7053398620512,15.));
#27267=CARTESIAN_POINT('Ctrl Pts',(-23.4307017328227,35.7540716771372,15.));
#27268=CARTESIAN_POINT('Ctrl Pts',(-23.5209523746427,35.8024138716897,15.));
#27269=CARTESIAN_POINT('Ctrl Pts',(-23.611560139948,35.8503675222885,15.));
#27270=CARTESIAN_POINT('Ctrl Pts',(-23.7025215735353,35.8979336336837,15.));
#27271=CARTESIAN_POINT('Ctrl Pts',(-23.7938331508737,35.9451131482488,15.));
#27272=CARTESIAN_POINT('Ctrl Pts',(-23.8854911428946,35.991906956547,15.));
#27273=CARTESIAN_POINT('Ctrl Pts',(-23.9774915680089,36.0383159101254,15.));
#27274=CARTESIAN_POINT('Ctrl Pts',(-24.0698304230588,36.0843408347974,15.));
#27275=CARTESIAN_POINT('Ctrl Pts',(-24.1625038657964,36.1299825471271,15.));
#27276=CARTESIAN_POINT('Ctrl Pts',(-24.2555084095332,36.1752418704833,15.));
#27277=CARTESIAN_POINT('Ctrl Pts',(-24.3488411214068,36.2201196586697,15.));
#27278=CARTESIAN_POINT('Ctrl Pts',(-24.4612315181512,36.2735162352736,15.));
#27279=CARTESIAN_POINT('Ctrl Pts',(-24.5552956307817,36.3175386315529,15.));
#27280=CARTESIAN_POINT('Ctrl Pts',(-24.630805301288,36.3524534604649,15.));
#27281=CARTESIAN_POINT('Ctrl Pts',(-24.6875827477484,36.37846926509,15.));
#27282=CARTESIAN_POINT('Ctrl Pts',(-24.725498909423,36.3957374383337,15.));
#27283=CARTESIAN_POINT('Ctrl Pts',(-14.911486495888,41.396226524684,0.));
#27284=CARTESIAN_POINT('Ctrl Pts',(-14.911486495888,41.396226524684,18.));
#27285=CARTESIAN_POINT('Ctrl Pts',(-14.9156446533966,41.3758141263348,0.));
#27286=CARTESIAN_POINT('Ctrl Pts',(-14.9156446533966,41.3758141263348,18.));
#27287=CARTESIAN_POINT('Ctrl Pts',(-14.9239113834707,41.3349931861715,0.));
#27288=CARTESIAN_POINT('Ctrl Pts',(-14.9239113834707,41.3349931861715,18.));
#27289=CARTESIAN_POINT('Ctrl Pts',(-14.936162723752,41.2737733455422,0.));
#27290=CARTESIAN_POINT('Ctrl Pts',(-14.936162723752,41.2737733455422,18.));
#27291=CARTESIAN_POINT('Ctrl Pts',(-14.9522002356298,41.1921700381957,0.));
#27292=CARTESIAN_POINT('Ctrl Pts',(-14.9522002356298,41.1921700381957,18.));
#27293=CARTESIAN_POINT('Ctrl Pts',(-14.9717503874227,41.0902046498729,0.));
#27294=CARTESIAN_POINT('Ctrl Pts',(-14.9717503874227,41.0902046498729,18.));
#27295=CARTESIAN_POINT('Ctrl Pts',(-14.9908026205824,40.9882784321884,0.));
#27296=CARTESIAN_POINT('Ctrl Pts',(-14.9908026205824,40.9882784321884,18.));
#27297=CARTESIAN_POINT('Ctrl Pts',(-15.0093553188655,40.8863921801,0.));
#27298=CARTESIAN_POINT('Ctrl Pts',(-15.0093553188655,40.8863921801,18.));
#27299=CARTESIAN_POINT('Ctrl Pts',(-15.0274064563211,40.7845471608654,0.));
#27300=CARTESIAN_POINT('Ctrl Pts',(-15.0274064563211,40.7845471608654,18.));
#27301=CARTESIAN_POINT('Ctrl Pts',(-15.0449536183143,40.6827452453667,0.));
#27302=CARTESIAN_POINT('Ctrl Pts',(-15.0449536183143,40.6827452453667,18.));
#27303=CARTESIAN_POINT('Ctrl Pts',(-15.0619940893017,40.58098877043,0.));
#27304=CARTESIAN_POINT('Ctrl Pts',(-15.0619940893017,40.58098877043,18.));
#27305=CARTESIAN_POINT('Ctrl Pts',(-15.0785249502524,40.4792803645352,0.));
#27306=CARTESIAN_POINT('Ctrl Pts',(-15.0785249502524,40.4792803645352,18.));
#27307=CARTESIAN_POINT('Ctrl Pts',(-15.0945431800723,40.3776227809037,0.));
#27308=CARTESIAN_POINT('Ctrl Pts',(-15.0945431800723,40.3776227809037,18.));
#27309=CARTESIAN_POINT('Ctrl Pts',(-15.1100457495259,40.2760187401821,0.));
#27310=CARTESIAN_POINT('Ctrl Pts',(-15.1100457495259,40.2760187401821,18.));
#27311=CARTESIAN_POINT('Ctrl Pts',(-15.1250297462408,40.1744707357902,0.));
#27312=CARTESIAN_POINT('Ctrl Pts',(-15.1250297462408,40.1744707357902,18.));
#27313=CARTESIAN_POINT('Ctrl Pts',(-15.1394923361537,40.0729810652204,0.));
#27314=CARTESIAN_POINT('Ctrl Pts',(-15.1394923361537,40.0729810652204,18.));
#27315=CARTESIAN_POINT('Ctrl Pts',(-15.1534306754871,39.9715519332134,0.));
#27316=CARTESIAN_POINT('Ctrl Pts',(-15.1534306754871,39.9715519332134,18.));
#27317=CARTESIAN_POINT('Ctrl Pts',(-15.1668418393198,39.8701855339908,0.));
#27318=CARTESIAN_POINT('Ctrl Pts',(-15.1668418393198,39.8701855339908,18.));
#27319=CARTESIAN_POINT('Ctrl Pts',(-15.1797227547561,39.7688841338802,0.));
#27320=CARTESIAN_POINT('Ctrl Pts',(-15.1797227547561,39.7688841338802,18.));
#27321=CARTESIAN_POINT('Ctrl Pts',(-15.1920701163803,39.6676501731673,0.));
#27322=CARTESIAN_POINT('Ctrl Pts',(-15.1920701163803,39.6676501731673,18.));
#27323=CARTESIAN_POINT('Ctrl Pts',(-15.2038804098649,39.5664862602472,0.));
#27324=CARTESIAN_POINT('Ctrl Pts',(-15.2038804098649,39.5664862602472,18.));
#27325=CARTESIAN_POINT('Ctrl Pts',(-15.2151499908149,39.4653951093947,0.));
#27326=CARTESIAN_POINT('Ctrl Pts',(-15.2151499908149,39.4653951093947,18.));
#27327=CARTESIAN_POINT('Ctrl Pts',(-15.2258751563069,39.3643794927167,0.));
#27328=CARTESIAN_POINT('Ctrl Pts',(-15.2258751563069,39.3643794927167,18.));
#27329=CARTESIAN_POINT('Ctrl Pts',(-15.2360522089072,39.2634421927888,0.));
#27330=CARTESIAN_POINT('Ctrl Pts',(-15.2360522089072,39.2634421927888,18.));
#27331=CARTESIAN_POINT('Ctrl Pts',(-15.2456775636447,39.1625859371304,0.));
#27332=CARTESIAN_POINT('Ctrl Pts',(-15.2456775636447,39.1625859371304,18.));
#27333=CARTESIAN_POINT('Ctrl Pts',(-15.2547476855825,39.061813415425,0.));
#27334=CARTESIAN_POINT('Ctrl Pts',(-15.2547476855825,39.061813415425,18.));
#27335=CARTESIAN_POINT('Ctrl Pts',(-15.2632589109473,38.9611273555758,0.));
#27336=CARTESIAN_POINT('Ctrl Pts',(-15.2632589109473,38.9611273555758,18.));
#27337=CARTESIAN_POINT('Ctrl Pts',(-15.2712072937639,38.860530586589,0.));
#27338=CARTESIAN_POINT('Ctrl Pts',(-15.2712072937639,38.860530586589,18.));
#27339=CARTESIAN_POINT('Ctrl Pts',(-15.2785884727112,38.7600260961351,0.));
#27340=CARTESIAN_POINT('Ctrl Pts',(-15.2785884727112,38.7600260961351,18.));
#27341=CARTESIAN_POINT('Ctrl Pts',(-15.2853974668211,38.659617115053,0.));
#27342=CARTESIAN_POINT('Ctrl Pts',(-15.2853974668211,38.659617115053,18.));
#27343=CARTESIAN_POINT('Ctrl Pts',(-15.2916287700102,38.5593070891769,0.));
#27344=CARTESIAN_POINT('Ctrl Pts',(-15.2916287700102,38.5593070891769,18.));
#27345=CARTESIAN_POINT('Ctrl Pts',(-15.2972767037469,38.4590995527814,0.));
#27346=CARTESIAN_POINT('Ctrl Pts',(-15.2972767037469,38.4590995527814,18.));
#27347=CARTESIAN_POINT('Ctrl Pts',(-15.3023357307483,38.3589980188324,0.));
#27348=CARTESIAN_POINT('Ctrl Pts',(-15.3023357307483,38.3589980188324,18.));
#27349=CARTESIAN_POINT('Ctrl Pts',(-15.3068007250314,38.2590058835965,0.));
#27350=CARTESIAN_POINT('Ctrl Pts',(-15.3068007250314,38.2590058835965,18.));
#27351=CARTESIAN_POINT('Ctrl Pts',(-15.310667421514,38.1591262705847,0.));
#27352=CARTESIAN_POINT('Ctrl Pts',(-15.310667421514,38.1591262705847,18.));
#27353=CARTESIAN_POINT('Ctrl Pts',(-15.3139321941687,38.0593621055415,0.));
#27354=CARTESIAN_POINT('Ctrl Pts',(-15.3139321941687,38.0593621055415,18.));
#27355=CARTESIAN_POINT('Ctrl Pts',(-15.3165911656268,37.959716421934,0.));
#27356=CARTESIAN_POINT('Ctrl Pts',(-15.3165911656268,37.959716421934,18.));
#27357=CARTESIAN_POINT('Ctrl Pts',(-15.3186394335023,37.8601926265378,0.));
#27358=CARTESIAN_POINT('Ctrl Pts',(-15.3186394335023,37.8601926265378,18.));
#27359=CARTESIAN_POINT('Ctrl Pts',(-15.320070396385,37.7607947318286,0.));
#27360=CARTESIAN_POINT('Ctrl Pts',(-15.320070396385,37.7607947318286,18.));
#27361=CARTESIAN_POINT('Ctrl Pts',(-15.320874689078,37.6615277218027,0.));
#27362=CARTESIAN_POINT('Ctrl Pts',(-15.320874689078,37.6615277218027,18.));
#27363=CARTESIAN_POINT('Ctrl Pts',(-15.3210406145546,37.562397408596,0.));
#27364=CARTESIAN_POINT('Ctrl Pts',(-15.3210406145546,37.562397408596,18.));
#27365=CARTESIAN_POINT('Ctrl Pts',(-15.3205561366169,37.4634097578665,0.));
#27366=CARTESIAN_POINT('Ctrl Pts',(-15.3205561366169,37.4634097578665,18.));
#27367=CARTESIAN_POINT('Ctrl Pts',(-15.3194106233801,37.3645702997848,0.));
#27368=CARTESIAN_POINT('Ctrl Pts',(-15.3194106233801,37.3645702997848,18.));
#27369=CARTESIAN_POINT('Ctrl Pts',(-15.3175963510697,37.2658836214694,0.));
#27370=CARTESIAN_POINT('Ctrl Pts',(-15.3175963510697,37.2658836214694,18.));
#27371=CARTESIAN_POINT('Ctrl Pts',(-15.3151109648809,37.1673525354642,0.));
#27372=CARTESIAN_POINT('Ctrl Pts',(-15.3151109648809,37.1673525354642,18.));
#27373=CARTESIAN_POINT('Ctrl Pts',(-15.3119562971444,37.0689784837457,0.));
#27374=CARTESIAN_POINT('Ctrl Pts',(-15.3119562971444,37.0689784837457,18.));
#27375=CARTESIAN_POINT('Ctrl Pts',(-15.3081335446406,36.970763176802,0.));
#27376=CARTESIAN_POINT('Ctrl Pts',(-15.3081335446406,36.970763176802,18.));
#27377=CARTESIAN_POINT('Ctrl Pts',(-15.3036390436952,36.8727100302512,0.));
#27378=CARTESIAN_POINT('Ctrl Pts',(-15.3036390436952,36.8727100302512,18.));
#27379=CARTESIAN_POINT('Ctrl Pts',(-15.2984606286737,36.7748254044502,0.));
#27380=CARTESIAN_POINT('Ctrl Pts',(-15.2984606286737,36.7748254044502,18.));
#27381=CARTESIAN_POINT('Ctrl Pts',(-15.2925717100767,36.6771206167756,0.));
#27382=CARTESIAN_POINT('Ctrl Pts',(-15.2925717100767,36.6771206167756,18.));
#27383=CARTESIAN_POINT('Ctrl Pts',(-15.2859343913094,36.5796108931244,0.));
#27384=CARTESIAN_POINT('Ctrl Pts',(-15.2859343913094,36.5796108931244,18.));
#27385=CARTESIAN_POINT('Ctrl Pts',(-15.2785104654792,36.4823116513289,0.));
#27386=CARTESIAN_POINT('Ctrl Pts',(-15.2785104654792,36.4823116513289,18.));
#27387=CARTESIAN_POINT('Ctrl Pts',(-15.2702711460937,36.3852352131887,0.));
#27388=CARTESIAN_POINT('Ctrl Pts',(-15.2702711460937,36.3852352131887,18.));
#27389=CARTESIAN_POINT('Ctrl Pts',(-15.2612053303773,36.2883880151607,0.));
#27390=CARTESIAN_POINT('Ctrl Pts',(-15.2612053303773,36.2883880151607,18.));
#27391=CARTESIAN_POINT('Ctrl Pts',(-15.2513334565427,36.1917659216814,0.));
#27392=CARTESIAN_POINT('Ctrl Pts',(-15.2513334565427,36.1917659216814,18.));
#27393=CARTESIAN_POINT('Ctrl Pts',(-15.240697754828,36.095357546697,0.));
#27394=CARTESIAN_POINT('Ctrl Pts',(-15.240697754828,36.095357546697,18.));
#27395=CARTESIAN_POINT('Ctrl Pts',(-15.2293360946131,35.9991531408727,0.));
#27396=CARTESIAN_POINT('Ctrl Pts',(-15.2293360946131,35.9991531408727,18.));
#27397=CARTESIAN_POINT('Ctrl Pts',(-15.2172585668056,35.9031525499277,0.));
#27398=CARTESIAN_POINT('Ctrl Pts',(-15.2172585668056,35.9031525499277,18.));
#27399=CARTESIAN_POINT('Ctrl Pts',(-15.2044274601769,35.8073720252878,0.));
#27400=CARTESIAN_POINT('Ctrl Pts',(-15.2044274601769,35.8073720252878,18.));
#27401=CARTESIAN_POINT('Ctrl Pts',(-15.1907243629659,35.7118553943773,0.));
#27402=CARTESIAN_POINT('Ctrl Pts',(-15.1907243629659,35.7118553943773,18.));
#27403=CARTESIAN_POINT('Ctrl Pts',(-15.1759785763051,35.6166644736253,0.));
#27404=CARTESIAN_POINT('Ctrl Pts',(-15.1759785763051,35.6166644736253,18.));
#27405=CARTESIAN_POINT('Ctrl Pts',(-15.1600260710384,35.5218591529745,0.));
#27406=CARTESIAN_POINT('Ctrl Pts',(-15.1600260710384,35.5218591529745,18.));
#27407=CARTESIAN_POINT('Ctrl Pts',(-15.1427632633831,35.4274792115856,0.));
#27408=CARTESIAN_POINT('Ctrl Pts',(-15.1427632633831,35.4274792115856,18.));
#27409=CARTESIAN_POINT('Ctrl Pts',(-15.1241934020681,35.3335286891314,0.));
#27410=CARTESIAN_POINT('Ctrl Pts',(-15.1241934020681,35.3335286891314,18.));
#27411=CARTESIAN_POINT('Ctrl Pts',(-15.104500806927,35.2399506932815,0.));
#27412=CARTESIAN_POINT('Ctrl Pts',(-15.104500806927,35.2399506932815,18.));
#27413=CARTESIAN_POINT('Ctrl Pts',(-15.08395927165,35.1466591020976,0.));
#27414=CARTESIAN_POINT('Ctrl Pts',(-15.08395927165,35.1466591020976,18.));
#27415=CARTESIAN_POINT('Ctrl Pts',(-15.0627878528202,35.0535882932913,0.));
#27416=CARTESIAN_POINT('Ctrl Pts',(-15.0627878528202,35.0535882932913,18.));
#27417=CARTESIAN_POINT('Ctrl Pts',(-15.041018569143,34.9607388363587,0.));
#27418=CARTESIAN_POINT('Ctrl Pts',(-15.041018569143,34.9607388363587,18.));
#27419=CARTESIAN_POINT('Ctrl Pts',(-15.0183713484962,34.8682205930809,0.));
#27420=CARTESIAN_POINT('Ctrl Pts',(-15.0183713484962,34.8682205930809,18.));
#27421=CARTESIAN_POINT('Ctrl Pts',(-14.9940927023322,34.7763085406486,0.));
#27422=CARTESIAN_POINT('Ctrl Pts',(-14.9940927023322,34.7763085406486,18.));
#27423=CARTESIAN_POINT('Ctrl Pts',(-14.9671565602316,34.6853717911268,0.));
#27424=CARTESIAN_POINT('Ctrl Pts',(-14.9671565602316,34.6853717911268,18.));
#27425=CARTESIAN_POINT('Ctrl Pts',(-14.9426481276593,34.6137007885254,0.));
#27426=CARTESIAN_POINT('Ctrl Pts',(-14.9426481276593,34.6137007885254,18.));
#27427=CARTESIAN_POINT('Ctrl Pts',(-14.9222326355678,34.5606858566713,0.));
#27428=CARTESIAN_POINT('Ctrl Pts',(-14.9222326355678,34.5606858566713,18.));
#27429=CARTESIAN_POINT('Ctrl Pts',(-14.9076710061311,34.525687510388,0.));
#27430=CARTESIAN_POINT('Ctrl Pts',(-14.9076710061311,34.525687510388,18.));
#27431=CARTESIAN_POINT('Ctrl Pts',(-14.9001523628048,34.5082745737944,0.));
#27432=CARTESIAN_POINT('Ctrl Pts',(-14.9001523628048,34.5082745737944,18.));
#27433=CARTESIAN_POINT('',(-14.9114864958881,41.3962265246839,0.));
#27434=CARTESIAN_POINT('Ctrl Pts',(-14.9001523628048,34.5082745737944,0.));
#27435=CARTESIAN_POINT('Ctrl Pts',(-14.9076710061311,34.525687510388,0.));
#27436=CARTESIAN_POINT('Ctrl Pts',(-14.9222326355678,34.5606858566713,0.));
#27437=CARTESIAN_POINT('Ctrl Pts',(-14.9426481276593,34.6137007885254,0.));
#27438=CARTESIAN_POINT('Ctrl Pts',(-14.9671565602316,34.6853717911268,0.));
#27439=CARTESIAN_POINT('Ctrl Pts',(-14.9940927023322,34.7763085406486,0.));
#27440=CARTESIAN_POINT('Ctrl Pts',(-15.0183713484962,34.8682205930809,0.));
#27441=CARTESIAN_POINT('Ctrl Pts',(-15.041018569143,34.9607388363587,0.));
#27442=CARTESIAN_POINT('Ctrl Pts',(-15.0627878528202,35.0535882932913,0.));
#27443=CARTESIAN_POINT('Ctrl Pts',(-15.08395927165,35.1466591020976,0.));
#27444=CARTESIAN_POINT('Ctrl Pts',(-15.104500806927,35.2399506932815,0.));
#27445=CARTESIAN_POINT('Ctrl Pts',(-15.1241934020681,35.3335286891314,0.));
#27446=CARTESIAN_POINT('Ctrl Pts',(-15.1427632633831,35.4274792115856,0.));
#27447=CARTESIAN_POINT('Ctrl Pts',(-15.1600260710384,35.5218591529745,0.));
#27448=CARTESIAN_POINT('Ctrl Pts',(-15.1759785763051,35.6166644736253,0.));
#27449=CARTESIAN_POINT('Ctrl Pts',(-15.1907243629659,35.7118553943773,0.));
#27450=CARTESIAN_POINT('Ctrl Pts',(-15.2044274601769,35.8073720252878,0.));
#27451=CARTESIAN_POINT('Ctrl Pts',(-15.2172585668056,35.9031525499277,0.));
#27452=CARTESIAN_POINT('Ctrl Pts',(-15.2293360946131,35.9991531408727,0.));
#27453=CARTESIAN_POINT('Ctrl Pts',(-15.240697754828,36.095357546697,0.));
#27454=CARTESIAN_POINT('Ctrl Pts',(-15.2513334565427,36.1917659216814,0.));
#27455=CARTESIAN_POINT('Ctrl Pts',(-15.2612053303773,36.2883880151607,0.));
#27456=CARTESIAN_POINT('Ctrl Pts',(-15.2702711460937,36.3852352131887,0.));
#27457=CARTESIAN_POINT('Ctrl Pts',(-15.2785104654792,36.4823116513289,0.));
#27458=CARTESIAN_POINT('Ctrl Pts',(-15.2859343913094,36.5796108931244,0.));
#27459=CARTESIAN_POINT('Ctrl Pts',(-15.2925717100767,36.6771206167756,0.));
#27460=CARTESIAN_POINT('Ctrl Pts',(-15.2984606286737,36.7748254044502,0.));
#27461=CARTESIAN_POINT('Ctrl Pts',(-15.3036390436952,36.8727100302512,0.));
#27462=CARTESIAN_POINT('Ctrl Pts',(-15.3081335446406,36.970763176802,0.));
#27463=CARTESIAN_POINT('Ctrl Pts',(-15.3119562971444,37.0689784837457,0.));
#27464=CARTESIAN_POINT('Ctrl Pts',(-15.3151109648809,37.1673525354642,0.));
#27465=CARTESIAN_POINT('Ctrl Pts',(-15.3175963510697,37.2658836214694,0.));
#27466=CARTESIAN_POINT('Ctrl Pts',(-15.3194106233801,37.3645702997848,0.));
#27467=CARTESIAN_POINT('Ctrl Pts',(-15.3205561366169,37.4634097578665,0.));
#27468=CARTESIAN_POINT('Ctrl Pts',(-15.3210406145546,37.562397408596,0.));
#27469=CARTESIAN_POINT('Ctrl Pts',(-15.320874689078,37.6615277218027,0.));
#27470=CARTESIAN_POINT('Ctrl Pts',(-15.320070396385,37.7607947318286,0.));
#27471=CARTESIAN_POINT('Ctrl Pts',(-15.3186394335023,37.8601926265378,0.));
#27472=CARTESIAN_POINT('Ctrl Pts',(-15.3165911656268,37.959716421934,0.));
#27473=CARTESIAN_POINT('Ctrl Pts',(-15.3139321941687,38.0593621055415,0.));
#27474=CARTESIAN_POINT('Ctrl Pts',(-15.310667421514,38.1591262705847,0.));
#27475=CARTESIAN_POINT('Ctrl Pts',(-15.3068007250314,38.2590058835965,0.));
#27476=CARTESIAN_POINT('Ctrl Pts',(-15.3023357307483,38.3589980188324,0.));
#27477=CARTESIAN_POINT('Ctrl Pts',(-15.2972767037469,38.4590995527814,0.));
#27478=CARTESIAN_POINT('Ctrl Pts',(-15.2916287700102,38.5593070891769,0.));
#27479=CARTESIAN_POINT('Ctrl Pts',(-15.2853974668211,38.659617115053,0.));
#27480=CARTESIAN_POINT('Ctrl Pts',(-15.2785884727112,38.7600260961351,0.));
#27481=CARTESIAN_POINT('Ctrl Pts',(-15.2712072937639,38.860530586589,0.));
#27482=CARTESIAN_POINT('Ctrl Pts',(-15.2632589109473,38.9611273555758,0.));
#27483=CARTESIAN_POINT('Ctrl Pts',(-15.2547476855825,39.061813415425,0.));
#27484=CARTESIAN_POINT('Ctrl Pts',(-15.2456775636447,39.1625859371304,0.));
#27485=CARTESIAN_POINT('Ctrl Pts',(-15.2360522089072,39.2634421927888,0.));
#27486=CARTESIAN_POINT('Ctrl Pts',(-15.2258751563069,39.3643794927167,0.));
#27487=CARTESIAN_POINT('Ctrl Pts',(-15.2151499908149,39.4653951093947,0.));
#27488=CARTESIAN_POINT('Ctrl Pts',(-15.2038804098649,39.5664862602472,0.));
#27489=CARTESIAN_POINT('Ctrl Pts',(-15.1920701163803,39.6676501731673,0.));
#27490=CARTESIAN_POINT('Ctrl Pts',(-15.1797227547561,39.7688841338802,0.));
#27491=CARTESIAN_POINT('Ctrl Pts',(-15.1668418393198,39.8701855339908,0.));
#27492=CARTESIAN_POINT('Ctrl Pts',(-15.1534306754871,39.9715519332134,0.));
#27493=CARTESIAN_POINT('Ctrl Pts',(-15.1394923361537,40.0729810652204,0.));
#27494=CARTESIAN_POINT('Ctrl Pts',(-15.1250297462408,40.1744707357902,0.));
#27495=CARTESIAN_POINT('Ctrl Pts',(-15.1100457495259,40.2760187401821,0.));
#27496=CARTESIAN_POINT('Ctrl Pts',(-15.0945431800723,40.3776227809037,0.));
#27497=CARTESIAN_POINT('Ctrl Pts',(-15.0785249502524,40.4792803645352,0.));
#27498=CARTESIAN_POINT('Ctrl Pts',(-15.0619940893017,40.58098877043,0.));
#27499=CARTESIAN_POINT('Ctrl Pts',(-15.0449536183143,40.6827452453667,0.));
#27500=CARTESIAN_POINT('Ctrl Pts',(-15.0274064563211,40.7845471608654,0.));
#27501=CARTESIAN_POINT('Ctrl Pts',(-15.0093553188655,40.8863921801,0.));
#27502=CARTESIAN_POINT('Ctrl Pts',(-14.9908026205824,40.9882784321884,0.));
#27503=CARTESIAN_POINT('Ctrl Pts',(-14.9679399407908,41.1105898934098,0.));
#27504=CARTESIAN_POINT('Ctrl Pts',(-14.9482653093396,41.2125650743922,0.));
#27505=CARTESIAN_POINT('Ctrl Pts',(-14.9321285285561,41.2941761025922,0.));
#27506=CARTESIAN_POINT('Ctrl Pts',(-14.919802810928,41.3554017279611,0.));
#27507=CARTESIAN_POINT('Ctrl Pts',(-14.911486495888,41.396226524684,0.));
#27508=CARTESIAN_POINT('',(-14.9114864958881,41.3962265246839,15.));
#27509=CARTESIAN_POINT('Ctrl Pts',(-14.911486495888,41.396226524684,15.));
#27510=CARTESIAN_POINT('Ctrl Pts',(-14.9156446533966,41.3758141263348,15.));
#27511=CARTESIAN_POINT('Ctrl Pts',(-14.9239113834707,41.3349931861715,15.));
#27512=CARTESIAN_POINT('Ctrl Pts',(-14.936162723752,41.2737733455422,15.));
#27513=CARTESIAN_POINT('Ctrl Pts',(-14.9522002356298,41.1921700381957,15.));
#27514=CARTESIAN_POINT('Ctrl Pts',(-14.9717503874227,41.0902046498729,15.));
#27515=CARTESIAN_POINT('Ctrl Pts',(-14.9908026205824,40.9882784321884,15.));
#27516=CARTESIAN_POINT('Ctrl Pts',(-15.0093553188655,40.8863921801,15.));
#27517=CARTESIAN_POINT('Ctrl Pts',(-15.0274064563211,40.7845471608654,15.));
#27518=CARTESIAN_POINT('Ctrl Pts',(-15.0449536183143,40.6827452453667,15.));
#27519=CARTESIAN_POINT('Ctrl Pts',(-15.0619940893017,40.58098877043,15.));
#27520=CARTESIAN_POINT('Ctrl Pts',(-15.0785249502524,40.4792803645352,15.));
#27521=CARTESIAN_POINT('Ctrl Pts',(-15.0945431800723,40.3776227809037,15.));
#27522=CARTESIAN_POINT('Ctrl Pts',(-15.1100457495259,40.2760187401821,15.));
#27523=CARTESIAN_POINT('Ctrl Pts',(-15.1250297462408,40.1744707357902,15.));
#27524=CARTESIAN_POINT('Ctrl Pts',(-15.1394923361537,40.0729810652204,15.));
#27525=CARTESIAN_POINT('Ctrl Pts',(-15.1534306754871,39.9715519332134,15.));
#27526=CARTESIAN_POINT('Ctrl Pts',(-15.1668418393198,39.8701855339908,15.));
#27527=CARTESIAN_POINT('Ctrl Pts',(-15.1797227547561,39.7688841338802,15.));
#27528=CARTESIAN_POINT('Ctrl Pts',(-15.1920701163803,39.6676501731673,15.));
#27529=CARTESIAN_POINT('Ctrl Pts',(-15.2038804098649,39.5664862602472,15.));
#27530=CARTESIAN_POINT('Ctrl Pts',(-15.2151499908149,39.4653951093947,15.));
#27531=CARTESIAN_POINT('Ctrl Pts',(-15.2258751563069,39.3643794927167,15.));
#27532=CARTESIAN_POINT('Ctrl Pts',(-15.2360522089072,39.2634421927888,15.));
#27533=CARTESIAN_POINT('Ctrl Pts',(-15.2456775636447,39.1625859371304,15.));
#27534=CARTESIAN_POINT('Ctrl Pts',(-15.2547476855825,39.061813415425,15.));
#27535=CARTESIAN_POINT('Ctrl Pts',(-15.2632589109473,38.9611273555758,15.));
#27536=CARTESIAN_POINT('Ctrl Pts',(-15.2712072937639,38.860530586589,15.));
#27537=CARTESIAN_POINT('Ctrl Pts',(-15.2785884727112,38.7600260961351,15.));
#27538=CARTESIAN_POINT('Ctrl Pts',(-15.2853974668211,38.659617115053,15.));
#27539=CARTESIAN_POINT('Ctrl Pts',(-15.2916287700102,38.5593070891769,15.));
#27540=CARTESIAN_POINT('Ctrl Pts',(-15.2972767037469,38.4590995527814,15.));
#27541=CARTESIAN_POINT('Ctrl Pts',(-15.3023357307483,38.3589980188324,15.));
#27542=CARTESIAN_POINT('Ctrl Pts',(-15.3068007250314,38.2590058835965,15.));
#27543=CARTESIAN_POINT('Ctrl Pts',(-15.310667421514,38.1591262705847,15.));
#27544=CARTESIAN_POINT('Ctrl Pts',(-15.3139321941687,38.0593621055415,15.));
#27545=CARTESIAN_POINT('Ctrl Pts',(-15.3165911656268,37.959716421934,15.));
#27546=CARTESIAN_POINT('Ctrl Pts',(-15.3186394335023,37.8601926265378,15.));
#27547=CARTESIAN_POINT('Ctrl Pts',(-15.320070396385,37.7607947318286,15.));
#27548=CARTESIAN_POINT('Ctrl Pts',(-15.320874689078,37.6615277218027,15.));
#27549=CARTESIAN_POINT('Ctrl Pts',(-15.3210406145546,37.562397408596,15.));
#27550=CARTESIAN_POINT('Ctrl Pts',(-15.3205561366169,37.4634097578665,15.));
#27551=CARTESIAN_POINT('Ctrl Pts',(-15.3194106233801,37.3645702997848,15.));
#27552=CARTESIAN_POINT('Ctrl Pts',(-15.3175963510697,37.2658836214694,15.));
#27553=CARTESIAN_POINT('Ctrl Pts',(-15.3151109648809,37.1673525354642,15.));
#27554=CARTESIAN_POINT('Ctrl Pts',(-15.3119562971444,37.0689784837457,15.));
#27555=CARTESIAN_POINT('Ctrl Pts',(-15.3081335446406,36.970763176802,15.));
#27556=CARTESIAN_POINT('Ctrl Pts',(-15.3036390436952,36.8727100302512,15.));
#27557=CARTESIAN_POINT('Ctrl Pts',(-15.2984606286737,36.7748254044502,15.));
#27558=CARTESIAN_POINT('Ctrl Pts',(-15.2925717100767,36.6771206167756,15.));
#27559=CARTESIAN_POINT('Ctrl Pts',(-15.2859343913094,36.5796108931244,15.));
#27560=CARTESIAN_POINT('Ctrl Pts',(-15.2785104654792,36.4823116513289,15.));
#27561=CARTESIAN_POINT('Ctrl Pts',(-15.2702711460937,36.3852352131887,15.));
#27562=CARTESIAN_POINT('Ctrl Pts',(-15.2612053303773,36.2883880151607,15.));
#27563=CARTESIAN_POINT('Ctrl Pts',(-15.2513334565427,36.1917659216814,15.));
#27564=CARTESIAN_POINT('Ctrl Pts',(-15.240697754828,36.095357546697,15.));
#27565=CARTESIAN_POINT('Ctrl Pts',(-15.2293360946131,35.9991531408727,15.));
#27566=CARTESIAN_POINT('Ctrl Pts',(-15.2172585668056,35.9031525499277,15.));
#27567=CARTESIAN_POINT('Ctrl Pts',(-15.2044274601769,35.8073720252878,15.));
#27568=CARTESIAN_POINT('Ctrl Pts',(-15.1907243629659,35.7118553943773,15.));
#27569=CARTESIAN_POINT('Ctrl Pts',(-15.1759785763051,35.6166644736253,15.));
#27570=CARTESIAN_POINT('Ctrl Pts',(-15.1600260710384,35.5218591529745,15.));
#27571=CARTESIAN_POINT('Ctrl Pts',(-15.1427632633831,35.4274792115856,15.));
#27572=CARTESIAN_POINT('Ctrl Pts',(-15.1241934020681,35.3335286891314,15.));
#27573=CARTESIAN_POINT('Ctrl Pts',(-15.104500806927,35.2399506932815,15.));
#27574=CARTESIAN_POINT('Ctrl Pts',(-15.08395927165,35.1466591020976,15.));
#27575=CARTESIAN_POINT('Ctrl Pts',(-15.0627878528202,35.0535882932913,15.));
#27576=CARTESIAN_POINT('Ctrl Pts',(-15.041018569143,34.9607388363587,15.));
#27577=CARTESIAN_POINT('Ctrl Pts',(-15.0183713484962,34.8682205930809,15.));
#27578=CARTESIAN_POINT('Ctrl Pts',(-14.9940927023322,34.7763085406486,15.));
#27579=CARTESIAN_POINT('Ctrl Pts',(-14.9671565602316,34.6853717911268,15.));
#27580=CARTESIAN_POINT('Ctrl Pts',(-14.9426481276593,34.6137007885254,15.));
#27581=CARTESIAN_POINT('Ctrl Pts',(-14.9222326355678,34.5606858566713,15.));
#27582=CARTESIAN_POINT('Ctrl Pts',(-14.9076710061311,34.525687510388,15.));
#27583=CARTESIAN_POINT('Ctrl Pts',(-14.9001523628048,34.5082745737944,15.));
#27584=CARTESIAN_POINT('',(-14.9114864958881,41.3962265246839,0.));
#27585=CARTESIAN_POINT('Origin',(-3.50213800024364E-12,1.07784724682657E-11,
0.));
#27586=CARTESIAN_POINT('',(-12.2684454652018,42.2550026135057,0.));
#27587=CARTESIAN_POINT('Origin',(-3.50213800024364E-12,1.07784724682657E-11,
0.));
#27588=CARTESIAN_POINT('',(-12.2684454652018,42.2550026135057,15.));
#27589=CARTESIAN_POINT('Origin',(-3.50213800024364E-12,1.07784724682657E-11,
15.));
#27590=CARTESIAN_POINT('',(-12.2684454652018,42.2550026135057,0.));
#27591=CARTESIAN_POINT('Ctrl Pts',(-8.22897839625061,36.6758703925241,0.));
#27592=CARTESIAN_POINT('Ctrl Pts',(-8.22897839625061,36.6758703925241,18.));
#27593=CARTESIAN_POINT('Ctrl Pts',(-8.23313075335376,36.6943771018148,0.));
#27594=CARTESIAN_POINT('Ctrl Pts',(-8.23313075335376,36.6943771018148,18.));
#27595=CARTESIAN_POINT('Ctrl Pts',(-8.24192165947367,36.7312504697652,0.));
#27596=CARTESIAN_POINT('Ctrl Pts',(-8.24192165947367,36.7312504697652,18.));
#27597=CARTESIAN_POINT('Ctrl Pts',(-8.2565665745182,36.7861403757604,0.));
#27598=CARTESIAN_POINT('Ctrl Pts',(-8.2565665745182,36.7861403757604,18.));
#27599=CARTESIAN_POINT('Ctrl Pts',(-8.27886599440784,36.8585291300917,0.));
#27600=CARTESIAN_POINT('Ctrl Pts',(-8.27886599440784,36.8585291300917,18.));
#27601=CARTESIAN_POINT('Ctrl Pts',(-8.31052547794591,36.9479311729484,0.));
#27602=CARTESIAN_POINT('Ctrl Pts',(-8.31052547794591,36.9479311729484,18.));
#27603=CARTESIAN_POINT('Ctrl Pts',(-8.34490818952639,37.0365602155148,0.));
#27604=CARTESIAN_POINT('Ctrl Pts',(-8.34490818952639,37.0365602155148,18.));
#27605=CARTESIAN_POINT('Ctrl Pts',(-8.38096706211447,37.1247207489179,0.));
#27606=CARTESIAN_POINT('Ctrl Pts',(-8.38096706211447,37.1247207489179,18.));
#27607=CARTESIAN_POINT('Ctrl Pts',(-8.4179308831326,37.2126332013933,0.));
#27608=CARTESIAN_POINT('Ctrl Pts',(-8.4179308831326,37.2126332013933,18.));
#27609=CARTESIAN_POINT('Ctrl Pts',(-8.45550849433959,37.3003733151561,0.));
#27610=CARTESIAN_POINT('Ctrl Pts',(-8.45550849433959,37.3003733151561,18.));
#27611=CARTESIAN_POINT('Ctrl Pts',(-8.49372546467075,37.3879218093514,0.));
#27612=CARTESIAN_POINT('Ctrl Pts',(-8.49372546467075,37.3879218093514,18.));
#27613=CARTESIAN_POINT('Ctrl Pts',(-8.53279758643784,37.4752030152968,0.));
#27614=CARTESIAN_POINT('Ctrl Pts',(-8.53279758643784,37.4752030152968,18.));
#27615=CARTESIAN_POINT('Ctrl Pts',(-8.57299698459465,37.5621256752108,0.));
#27616=CARTESIAN_POINT('Ctrl Pts',(-8.57299698459465,37.5621256752108,18.));
#27617=CARTESIAN_POINT('Ctrl Pts',(-8.61450621749155,37.6486274754754,0.));
#27618=CARTESIAN_POINT('Ctrl Pts',(-8.61450621749155,37.6486274754754,18.));
#27619=CARTESIAN_POINT('Ctrl Pts',(-8.65732553894524,37.7347032383719,0.));
#27620=CARTESIAN_POINT('Ctrl Pts',(-8.65732553894524,37.7347032383719,18.));
#27621=CARTESIAN_POINT('Ctrl Pts',(-8.70134776631143,37.8203816669031,0.));
#27622=CARTESIAN_POINT('Ctrl Pts',(-8.70134776631143,37.8203816669031,18.));
#27623=CARTESIAN_POINT('Ctrl Pts',(-8.74640499479002,37.9057107230066,0.));
#27624=CARTESIAN_POINT('Ctrl Pts',(-8.74640499479002,37.9057107230066,18.));
#27625=CARTESIAN_POINT('Ctrl Pts',(-8.79232279131092,37.9907407304174,0.));
#27626=CARTESIAN_POINT('Ctrl Pts',(-8.79232279131092,37.9907407304174,18.));
#27627=CARTESIAN_POINT('Ctrl Pts',(-8.83897959763348,38.0755058326913,0.));
#27628=CARTESIAN_POINT('Ctrl Pts',(-8.83897959763348,38.0755058326913,18.));
#27629=CARTESIAN_POINT('Ctrl Pts',(-8.88633535238434,38.1600150482528,0.));
#27630=CARTESIAN_POINT('Ctrl Pts',(-8.88633535238434,38.1600150482528,18.));
#27631=CARTESIAN_POINT('Ctrl Pts',(-8.93439830996339,38.2442625706309,0.));
#27632=CARTESIAN_POINT('Ctrl Pts',(-8.93439830996339,38.2442625706309,18.));
#27633=CARTESIAN_POINT('Ctrl Pts',(-8.98320483785759,38.3282340281403,0.));
#27634=CARTESIAN_POINT('Ctrl Pts',(-8.98320483785759,38.3282340281403,18.));
#27635=CARTESIAN_POINT('Ctrl Pts',(-9.0327957936019,38.4119138099805,0.));
#27636=CARTESIAN_POINT('Ctrl Pts',(-9.0327957936019,38.4119138099805,18.));
#27637=CARTESIAN_POINT('Ctrl Pts',(-9.08319014288085,38.4952932486131,0.));
#27638=CARTESIAN_POINT('Ctrl Pts',(-9.08319014288085,38.4952932486131,18.));
#27639=CARTESIAN_POINT('Ctrl Pts',(-9.13437512010585,38.5783736628826,0.));
#27640=CARTESIAN_POINT('Ctrl Pts',(-9.13437512010585,38.5783736628826,18.));
#27641=CARTESIAN_POINT('Ctrl Pts',(-9.18632019394329,38.6611620045193,0.));
#27642=CARTESIAN_POINT('Ctrl Pts',(-9.18632019394329,38.6611620045193,18.));
#27643=CARTESIAN_POINT('Ctrl Pts',(-9.23898539199331,38.7436682576832,0.));
#27644=CARTESIAN_POINT('Ctrl Pts',(-9.23898539199331,38.7436682576832,18.));
#27645=CARTESIAN_POINT('Ctrl Pts',(-9.29233110570902,38.8259023794241,0.));
#27646=CARTESIAN_POINT('Ctrl Pts',(-9.29233110570902,38.8259023794241,18.));
#27647=CARTESIAN_POINT('Ctrl Pts',(-9.34632917154636,38.9078708427078,0.));
#27648=CARTESIAN_POINT('Ctrl Pts',(-9.34632917154636,38.9078708427078,18.));
#27649=CARTESIAN_POINT('Ctrl Pts',(-9.40096600877643,38.9895756526779,0.));
#27650=CARTESIAN_POINT('Ctrl Pts',(-9.40096600877643,38.9895756526779,18.));
#27651=CARTESIAN_POINT('Ctrl Pts',(-9.45623664577431,39.0710161994951,0.));
#27652=CARTESIAN_POINT('Ctrl Pts',(-9.45623664577431,39.0710161994951,18.));
#27653=CARTESIAN_POINT('Ctrl Pts',(-9.5121410453562,39.1521903958955,0.));
#27654=CARTESIAN_POINT('Ctrl Pts',(-9.5121410453562,39.1521903958955,18.));
#27655=CARTESIAN_POINT('Ctrl Pts',(-9.56867984233622,39.2330959982788,0.));
#27656=CARTESIAN_POINT('Ctrl Pts',(-9.56867984233622,39.2330959982788,18.));
#27657=CARTESIAN_POINT('Ctrl Pts',(-9.62584947846543,39.3137321153686,0.));
#27658=CARTESIAN_POINT('Ctrl Pts',(-9.62584947846543,39.3137321153686,18.));
#27659=CARTESIAN_POINT('Ctrl Pts',(-9.68364100883826,39.3940995760289,0.));
#27660=CARTESIAN_POINT('Ctrl Pts',(-9.68364100883826,39.3940995760289,18.));
#27661=CARTESIAN_POINT('Ctrl Pts',(-9.74204258152663,39.4742001555227,0.));
#27662=CARTESIAN_POINT('Ctrl Pts',(-9.74204258152663,39.4742001555227,18.));
#27663=CARTESIAN_POINT('Ctrl Pts',(-9.80104095251613,39.5540361022309,0.));
#27664=CARTESIAN_POINT('Ctrl Pts',(-9.80104095251613,39.5540361022309,18.));
#27665=CARTESIAN_POINT('Ctrl Pts',(-9.86062324242559,39.6336095893767,0.));
#27666=CARTESIAN_POINT('Ctrl Pts',(-9.86062324242559,39.6336095893767,18.));
#27667=CARTESIAN_POINT('Ctrl Pts',(-9.92077894513191,39.712922089547,0.));
#27668=CARTESIAN_POINT('Ctrl Pts',(-9.92077894513191,39.712922089547,18.));
#27669=CARTESIAN_POINT('Ctrl Pts',(-9.98150036150822,39.7919742367922,0.));
#27670=CARTESIAN_POINT('Ctrl Pts',(-9.98150036150822,39.7919742367922,18.));
#27671=CARTESIAN_POINT('Ctrl Pts',(-10.0427815229883,39.8707661565233,0.));
#27672=CARTESIAN_POINT('Ctrl Pts',(-10.0427815229883,39.8707661565233,18.));
#27673=CARTESIAN_POINT('Ctrl Pts',(-10.1046175096878,39.9492976736738,0.));
#27674=CARTESIAN_POINT('Ctrl Pts',(-10.1046175096878,39.9492976736738,18.));
#27675=CARTESIAN_POINT('Ctrl Pts',(-10.1670036683795,40.0275685525923,0.));
#27676=CARTESIAN_POINT('Ctrl Pts',(-10.1670036683795,40.0275685525923,18.));
#27677=CARTESIAN_POINT('Ctrl Pts',(-10.2299347125857,40.1055787732578,0.));
#27678=CARTESIAN_POINT('Ctrl Pts',(-10.2299347125857,40.1055787732578,18.));
#27679=CARTESIAN_POINT('Ctrl Pts',(-10.2934044990237,40.1833286010098,0.));
#27680=CARTESIAN_POINT('Ctrl Pts',(-10.2934044990237,40.1833286010098,18.));
#27681=CARTESIAN_POINT('Ctrl Pts',(-10.3574064830678,40.2608184485326,0.));
#27682=CARTESIAN_POINT('Ctrl Pts',(-10.3574064830678,40.2608184485326,18.));
#27683=CARTESIAN_POINT('Ctrl Pts',(-10.421933993295,40.3380487942952,0.));
#27684=CARTESIAN_POINT('Ctrl Pts',(-10.421933993295,40.3380487942952,18.));
#27685=CARTESIAN_POINT('Ctrl Pts',(-10.48698054978,40.4150200869536,0.));
#27686=CARTESIAN_POINT('Ctrl Pts',(-10.48698054978,40.4150200869536,18.));
#27687=CARTESIAN_POINT('Ctrl Pts',(-10.5525402237951,40.4917326404439,0.));
#27688=CARTESIAN_POINT('Ctrl Pts',(-10.5525402237951,40.4917326404439,18.));
#27689=CARTESIAN_POINT('Ctrl Pts',(-10.618607730849,40.5681866012103,0.));
#27690=CARTESIAN_POINT('Ctrl Pts',(-10.618607730849,40.5681866012103,18.));
#27691=CARTESIAN_POINT('Ctrl Pts',(-10.6851782157325,40.6443819999244,0.));
#27692=CARTESIAN_POINT('Ctrl Pts',(-10.6851782157325,40.6443819999244,18.));
#27693=CARTESIAN_POINT('Ctrl Pts',(-10.7522471109694,40.7203187831783,0.));
#27694=CARTESIAN_POINT('Ctrl Pts',(-10.7522471109694,40.7203187831783,18.));
#27695=CARTESIAN_POINT('Ctrl Pts',(-10.8198099757795,40.795996852756,0.));
#27696=CARTESIAN_POINT('Ctrl Pts',(-10.8198099757795,40.795996852756,18.));
#27697=CARTESIAN_POINT('Ctrl Pts',(-10.8878623066646,40.8714161092412,0.));
#27698=CARTESIAN_POINT('Ctrl Pts',(-10.8878623066646,40.8714161092412,18.));
#27699=CARTESIAN_POINT('Ctrl Pts',(-10.956399476781,40.9465764747798,0.));
#27700=CARTESIAN_POINT('Ctrl Pts',(-10.956399476781,40.9465764747798,18.));
#27701=CARTESIAN_POINT('Ctrl Pts',(-11.0254168609972,41.0214778832142,0.));
#27702=CARTESIAN_POINT('Ctrl Pts',(-11.0254168609972,41.0214778832142,18.));
#27703=CARTESIAN_POINT('Ctrl Pts',(-11.0949099155251,41.0961202807715,0.));
#27704=CARTESIAN_POINT('Ctrl Pts',(-11.0949099155251,41.0961202807715,18.));
#27705=CARTESIAN_POINT('Ctrl Pts',(-11.1648742640378,41.1705036228854,0.));
#27706=CARTESIAN_POINT('Ctrl Pts',(-11.1648742640378,41.1705036228854,18.));
#27707=CARTESIAN_POINT('Ctrl Pts',(-11.2353057980338,41.2446278781981,0.));
#27708=CARTESIAN_POINT('Ctrl Pts',(-11.2353057980338,41.2446278781981,18.));
#27709=CARTESIAN_POINT('Ctrl Pts',(-11.3062006993745,41.3184930194148,0.));
#27710=CARTESIAN_POINT('Ctrl Pts',(-11.3062006993745,41.3184930194148,18.));
#27711=CARTESIAN_POINT('Ctrl Pts',(-11.3775553120176,41.3920989905986,0.));
#27712=CARTESIAN_POINT('Ctrl Pts',(-11.3775553120176,41.3920989905986,18.));
#27713=CARTESIAN_POINT('Ctrl Pts',(-11.4493660393849,41.4654456796071,0.));
#27714=CARTESIAN_POINT('Ctrl Pts',(-11.4493660393849,41.4654456796071,18.));
#27715=CARTESIAN_POINT('Ctrl Pts',(-11.5216292382388,41.5385328935506,0.));
#27716=CARTESIAN_POINT('Ctrl Pts',(-11.5216292382388,41.5385328935506,18.));
#27717=CARTESIAN_POINT('Ctrl Pts',(-11.5943410868252,41.6113603270596,0.));
#27718=CARTESIAN_POINT('Ctrl Pts',(-11.5943410868252,41.6113603270596,18.));
#27719=CARTESIAN_POINT('Ctrl Pts',(-11.6674975352851,41.6839275596248,0.));
#27720=CARTESIAN_POINT('Ctrl Pts',(-11.6674975352851,41.6839275596248,18.));
#27721=CARTESIAN_POINT('Ctrl Pts',(-11.7410945211992,41.7562341395977,0.));
#27722=CARTESIAN_POINT('Ctrl Pts',(-11.7410945211992,41.7562341395977,18.));
#27723=CARTESIAN_POINT('Ctrl Pts',(-11.81512813804,41.8282796562569,0.));
#27724=CARTESIAN_POINT('Ctrl Pts',(-11.81512813804,41.8282796562569,18.));
#27725=CARTESIAN_POINT('Ctrl Pts',(-11.8895948153349,41.9000638152266,0.));
#27726=CARTESIAN_POINT('Ctrl Pts',(-11.8895948153349,41.9000638152266,18.));
#27727=CARTESIAN_POINT('Ctrl Pts',(-11.9644914999263,41.9715865222182,0.));
#27728=CARTESIAN_POINT('Ctrl Pts',(-11.9644914999263,41.9715865222182,18.));
#27729=CARTESIAN_POINT('Ctrl Pts',(-12.0398158079102,42.0428479428228,0.));
#27730=CARTESIAN_POINT('Ctrl Pts',(-12.0398158079102,42.0428479428228,18.));
#27731=CARTESIAN_POINT('Ctrl Pts',(-12.1155659644537,42.1138483839101,0.));
#27732=CARTESIAN_POINT('Ctrl Pts',(-12.1155659644537,42.1138483839101,18.));
#27733=CARTESIAN_POINT('Ctrl Pts',(-12.1765058047069,42.1704402333854,0.));
#27734=CARTESIAN_POINT('Ctrl Pts',(-12.1765058047069,42.1704402333854,18.));
#27735=CARTESIAN_POINT('Ctrl Pts',(-12.2224014666679,42.2127669677092,0.));
#27736=CARTESIAN_POINT('Ctrl Pts',(-12.2224014666679,42.2127669677092,18.));
#27737=CARTESIAN_POINT('Ctrl Pts',(-12.2530833383985,42.2409327400055,0.));
#27738=CARTESIAN_POINT('Ctrl Pts',(-12.2530833383985,42.2409327400055,18.));
#27739=CARTESIAN_POINT('Ctrl Pts',(-12.2684454652018,42.2550026135057,0.));
#27740=CARTESIAN_POINT('Ctrl Pts',(-12.2684454652018,42.2550026135057,18.));
#27741=CARTESIAN_POINT('Ctrl Pts',(-8.22897839625061,36.6758703925241,0.));
#27742=CARTESIAN_POINT('Ctrl Pts',(-8.23313075335376,36.6943771018148,0.));
#27743=CARTESIAN_POINT('Ctrl Pts',(-8.24192165947367,36.7312504697652,0.));
#27744=CARTESIAN_POINT('Ctrl Pts',(-8.2565665745182,36.7861403757604,0.));
#27745=CARTESIAN_POINT('Ctrl Pts',(-8.27886599440784,36.8585291300917,0.));
#27746=CARTESIAN_POINT('Ctrl Pts',(-8.31052547794591,36.9479311729484,0.));
#27747=CARTESIAN_POINT('Ctrl Pts',(-8.34490818952639,37.0365602155148,0.));
#27748=CARTESIAN_POINT('Ctrl Pts',(-8.38096706211447,37.1247207489179,0.));
#27749=CARTESIAN_POINT('Ctrl Pts',(-8.4179308831326,37.2126332013933,0.));
#27750=CARTESIAN_POINT('Ctrl Pts',(-8.45550849433959,37.3003733151561,0.));
#27751=CARTESIAN_POINT('Ctrl Pts',(-8.49372546467075,37.3879218093514,0.));
#27752=CARTESIAN_POINT('Ctrl Pts',(-8.53279758643784,37.4752030152968,0.));
#27753=CARTESIAN_POINT('Ctrl Pts',(-8.57299698459465,37.5621256752108,0.));
#27754=CARTESIAN_POINT('Ctrl Pts',(-8.61450621749155,37.6486274754754,0.));
#27755=CARTESIAN_POINT('Ctrl Pts',(-8.65732553894524,37.7347032383719,0.));
#27756=CARTESIAN_POINT('Ctrl Pts',(-8.70134776631143,37.8203816669031,0.));
#27757=CARTESIAN_POINT('Ctrl Pts',(-8.74640499479002,37.9057107230066,0.));
#27758=CARTESIAN_POINT('Ctrl Pts',(-8.79232279131092,37.9907407304174,0.));
#27759=CARTESIAN_POINT('Ctrl Pts',(-8.83897959763348,38.0755058326913,0.));
#27760=CARTESIAN_POINT('Ctrl Pts',(-8.88633535238434,38.1600150482528,0.));
#27761=CARTESIAN_POINT('Ctrl Pts',(-8.93439830996339,38.2442625706309,0.));
#27762=CARTESIAN_POINT('Ctrl Pts',(-8.98320483785759,38.3282340281403,0.));
#27763=CARTESIAN_POINT('Ctrl Pts',(-9.0327957936019,38.4119138099805,0.));
#27764=CARTESIAN_POINT('Ctrl Pts',(-9.08319014288085,38.4952932486131,0.));
#27765=CARTESIAN_POINT('Ctrl Pts',(-9.13437512010585,38.5783736628826,0.));
#27766=CARTESIAN_POINT('Ctrl Pts',(-9.18632019394329,38.6611620045193,0.));
#27767=CARTESIAN_POINT('Ctrl Pts',(-9.23898539199331,38.7436682576832,0.));
#27768=CARTESIAN_POINT('Ctrl Pts',(-9.29233110570902,38.8259023794241,0.));
#27769=CARTESIAN_POINT('Ctrl Pts',(-9.34632917154636,38.9078708427078,0.));
#27770=CARTESIAN_POINT('Ctrl Pts',(-9.40096600877643,38.9895756526779,0.));
#27771=CARTESIAN_POINT('Ctrl Pts',(-9.45623664577431,39.0710161994951,0.));
#27772=CARTESIAN_POINT('Ctrl Pts',(-9.5121410453562,39.1521903958955,0.));
#27773=CARTESIAN_POINT('Ctrl Pts',(-9.56867984233622,39.2330959982788,0.));
#27774=CARTESIAN_POINT('Ctrl Pts',(-9.62584947846543,39.3137321153686,0.));
#27775=CARTESIAN_POINT('Ctrl Pts',(-9.68364100883826,39.3940995760289,0.));
#27776=CARTESIAN_POINT('Ctrl Pts',(-9.74204258152663,39.4742001555227,0.));
#27777=CARTESIAN_POINT('Ctrl Pts',(-9.80104095251613,39.5540361022309,0.));
#27778=CARTESIAN_POINT('Ctrl Pts',(-9.86062324242559,39.6336095893767,0.));
#27779=CARTESIAN_POINT('Ctrl Pts',(-9.92077894513191,39.712922089547,0.));
#27780=CARTESIAN_POINT('Ctrl Pts',(-9.98150036150822,39.7919742367922,0.));
#27781=CARTESIAN_POINT('Ctrl Pts',(-10.0427815229883,39.8707661565233,0.));
#27782=CARTESIAN_POINT('Ctrl Pts',(-10.1046175096878,39.9492976736738,0.));
#27783=CARTESIAN_POINT('Ctrl Pts',(-10.1670036683795,40.0275685525923,0.));
#27784=CARTESIAN_POINT('Ctrl Pts',(-10.2299347125857,40.1055787732578,0.));
#27785=CARTESIAN_POINT('Ctrl Pts',(-10.2934044990237,40.1833286010098,0.));
#27786=CARTESIAN_POINT('Ctrl Pts',(-10.3574064830678,40.2608184485326,0.));
#27787=CARTESIAN_POINT('Ctrl Pts',(-10.421933993295,40.3380487942952,0.));
#27788=CARTESIAN_POINT('Ctrl Pts',(-10.48698054978,40.4150200869536,0.));
#27789=CARTESIAN_POINT('Ctrl Pts',(-10.5525402237951,40.4917326404439,0.));
#27790=CARTESIAN_POINT('Ctrl Pts',(-10.618607730849,40.5681866012103,0.));
#27791=CARTESIAN_POINT('Ctrl Pts',(-10.6851782157325,40.6443819999244,0.));
#27792=CARTESIAN_POINT('Ctrl Pts',(-10.7522471109694,40.7203187831783,0.));
#27793=CARTESIAN_POINT('Ctrl Pts',(-10.8198099757795,40.795996852756,0.));
#27794=CARTESIAN_POINT('Ctrl Pts',(-10.8878623066646,40.8714161092412,0.));
#27795=CARTESIAN_POINT('Ctrl Pts',(-10.956399476781,40.9465764747798,0.));
#27796=CARTESIAN_POINT('Ctrl Pts',(-11.0254168609972,41.0214778832142,0.));
#27797=CARTESIAN_POINT('Ctrl Pts',(-11.0949099155251,41.0961202807715,0.));
#27798=CARTESIAN_POINT('Ctrl Pts',(-11.1648742640378,41.1705036228854,0.));
#27799=CARTESIAN_POINT('Ctrl Pts',(-11.2353057980338,41.2446278781981,0.));
#27800=CARTESIAN_POINT('Ctrl Pts',(-11.3062006993745,41.3184930194148,0.));
#27801=CARTESIAN_POINT('Ctrl Pts',(-11.3775553120176,41.3920989905986,0.));
#27802=CARTESIAN_POINT('Ctrl Pts',(-11.4493660393849,41.4654456796071,0.));
#27803=CARTESIAN_POINT('Ctrl Pts',(-11.5216292382388,41.5385328935506,0.));
#27804=CARTESIAN_POINT('Ctrl Pts',(-11.5943410868252,41.6113603270596,0.));
#27805=CARTESIAN_POINT('Ctrl Pts',(-11.6674975352851,41.6839275596248,0.));
#27806=CARTESIAN_POINT('Ctrl Pts',(-11.7410945211992,41.7562341395977,0.));
#27807=CARTESIAN_POINT('Ctrl Pts',(-11.81512813804,41.8282796562569,0.));
#27808=CARTESIAN_POINT('Ctrl Pts',(-11.8895948153349,41.9000638152266,0.));
#27809=CARTESIAN_POINT('Ctrl Pts',(-11.9644914999263,41.9715865222182,0.));
#27810=CARTESIAN_POINT('Ctrl Pts',(-12.054880669507,42.0571002269437,0.));
#27811=CARTESIAN_POINT('Ctrl Pts',(-12.1307372881904,42.1280354231517,0.));
#27812=CARTESIAN_POINT('Ctrl Pts',(-12.1917619768791,42.18457517013,0.));
#27813=CARTESIAN_POINT('Ctrl Pts',(-12.2377212115623,42.2268628664988,0.));
#27814=CARTESIAN_POINT('Ctrl Pts',(-12.2684454652018,42.2550026135057,0.));
#27815=CARTESIAN_POINT('Ctrl Pts',(-8.22897839625061,36.6758703925241,15.));
#27816=CARTESIAN_POINT('Ctrl Pts',(-8.23313075335376,36.6943771018148,15.));
#27817=CARTESIAN_POINT('Ctrl Pts',(-8.24192165947367,36.7312504697652,15.));
#27818=CARTESIAN_POINT('Ctrl Pts',(-8.2565665745182,36.7861403757604,15.));
#27819=CARTESIAN_POINT('Ctrl Pts',(-8.27886599440784,36.8585291300917,15.));
#27820=CARTESIAN_POINT('Ctrl Pts',(-8.31052547794591,36.9479311729484,15.));
#27821=CARTESIAN_POINT('Ctrl Pts',(-8.34490818952639,37.0365602155148,15.));
#27822=CARTESIAN_POINT('Ctrl Pts',(-8.38096706211447,37.1247207489179,15.));
#27823=CARTESIAN_POINT('Ctrl Pts',(-8.4179308831326,37.2126332013933,15.));
#27824=CARTESIAN_POINT('Ctrl Pts',(-8.45550849433959,37.3003733151561,15.));
#27825=CARTESIAN_POINT('Ctrl Pts',(-8.49372546467075,37.3879218093514,15.));
#27826=CARTESIAN_POINT('Ctrl Pts',(-8.53279758643784,37.4752030152968,15.));
#27827=CARTESIAN_POINT('Ctrl Pts',(-8.57299698459465,37.5621256752108,15.));
#27828=CARTESIAN_POINT('Ctrl Pts',(-8.61450621749155,37.6486274754754,15.));
#27829=CARTESIAN_POINT('Ctrl Pts',(-8.65732553894524,37.7347032383719,15.));
#27830=CARTESIAN_POINT('Ctrl Pts',(-8.70134776631143,37.8203816669031,15.));
#27831=CARTESIAN_POINT('Ctrl Pts',(-8.74640499479002,37.9057107230066,15.));
#27832=CARTESIAN_POINT('Ctrl Pts',(-8.79232279131092,37.9907407304174,15.));
#27833=CARTESIAN_POINT('Ctrl Pts',(-8.83897959763348,38.0755058326913,15.));
#27834=CARTESIAN_POINT('Ctrl Pts',(-8.88633535238434,38.1600150482528,15.));
#27835=CARTESIAN_POINT('Ctrl Pts',(-8.93439830996339,38.2442625706309,15.));
#27836=CARTESIAN_POINT('Ctrl Pts',(-8.98320483785759,38.3282340281403,15.));
#27837=CARTESIAN_POINT('Ctrl Pts',(-9.0327957936019,38.4119138099805,15.));
#27838=CARTESIAN_POINT('Ctrl Pts',(-9.08319014288085,38.4952932486131,15.));
#27839=CARTESIAN_POINT('Ctrl Pts',(-9.13437512010585,38.5783736628826,15.));
#27840=CARTESIAN_POINT('Ctrl Pts',(-9.18632019394329,38.6611620045193,15.));
#27841=CARTESIAN_POINT('Ctrl Pts',(-9.23898539199331,38.7436682576832,15.));
#27842=CARTESIAN_POINT('Ctrl Pts',(-9.29233110570902,38.8259023794241,15.));
#27843=CARTESIAN_POINT('Ctrl Pts',(-9.34632917154636,38.9078708427078,15.));
#27844=CARTESIAN_POINT('Ctrl Pts',(-9.40096600877643,38.9895756526779,15.));
#27845=CARTESIAN_POINT('Ctrl Pts',(-9.45623664577431,39.0710161994951,15.));
#27846=CARTESIAN_POINT('Ctrl Pts',(-9.5121410453562,39.1521903958955,15.));
#27847=CARTESIAN_POINT('Ctrl Pts',(-9.56867984233622,39.2330959982788,15.));
#27848=CARTESIAN_POINT('Ctrl Pts',(-9.62584947846543,39.3137321153686,15.));
#27849=CARTESIAN_POINT('Ctrl Pts',(-9.68364100883826,39.3940995760289,15.));
#27850=CARTESIAN_POINT('Ctrl Pts',(-9.74204258152663,39.4742001555227,15.));
#27851=CARTESIAN_POINT('Ctrl Pts',(-9.80104095251613,39.5540361022309,15.));
#27852=CARTESIAN_POINT('Ctrl Pts',(-9.86062324242559,39.6336095893767,15.));
#27853=CARTESIAN_POINT('Ctrl Pts',(-9.92077894513191,39.712922089547,15.));
#27854=CARTESIAN_POINT('Ctrl Pts',(-9.98150036150822,39.7919742367922,15.));
#27855=CARTESIAN_POINT('Ctrl Pts',(-10.0427815229883,39.8707661565233,15.));
#27856=CARTESIAN_POINT('Ctrl Pts',(-10.1046175096878,39.9492976736738,15.));
#27857=CARTESIAN_POINT('Ctrl Pts',(-10.1670036683795,40.0275685525923,15.));
#27858=CARTESIAN_POINT('Ctrl Pts',(-10.2299347125857,40.1055787732578,15.));
#27859=CARTESIAN_POINT('Ctrl Pts',(-10.2934044990237,40.1833286010098,15.));
#27860=CARTESIAN_POINT('Ctrl Pts',(-10.3574064830678,40.2608184485326,15.));
#27861=CARTESIAN_POINT('Ctrl Pts',(-10.421933993295,40.3380487942952,15.));
#27862=CARTESIAN_POINT('Ctrl Pts',(-10.48698054978,40.4150200869536,15.));
#27863=CARTESIAN_POINT('Ctrl Pts',(-10.5525402237951,40.4917326404439,15.));
#27864=CARTESIAN_POINT('Ctrl Pts',(-10.618607730849,40.5681866012103,15.));
#27865=CARTESIAN_POINT('Ctrl Pts',(-10.6851782157325,40.6443819999244,15.));
#27866=CARTESIAN_POINT('Ctrl Pts',(-10.7522471109694,40.7203187831783,15.));
#27867=CARTESIAN_POINT('Ctrl Pts',(-10.8198099757795,40.795996852756,15.));
#27868=CARTESIAN_POINT('Ctrl Pts',(-10.8878623066646,40.8714161092412,15.));
#27869=CARTESIAN_POINT('Ctrl Pts',(-10.956399476781,40.9465764747798,15.));
#27870=CARTESIAN_POINT('Ctrl Pts',(-11.0254168609972,41.0214778832142,15.));
#27871=CARTESIAN_POINT('Ctrl Pts',(-11.0949099155251,41.0961202807715,15.));
#27872=CARTESIAN_POINT('Ctrl Pts',(-11.1648742640378,41.1705036228854,15.));
#27873=CARTESIAN_POINT('Ctrl Pts',(-11.2353057980338,41.2446278781981,15.));
#27874=CARTESIAN_POINT('Ctrl Pts',(-11.3062006993745,41.3184930194148,15.));
#27875=CARTESIAN_POINT('Ctrl Pts',(-11.3775553120176,41.3920989905986,15.));
#27876=CARTESIAN_POINT('Ctrl Pts',(-11.4493660393849,41.4654456796071,15.));
#27877=CARTESIAN_POINT('Ctrl Pts',(-11.5216292382388,41.5385328935506,15.));
#27878=CARTESIAN_POINT('Ctrl Pts',(-11.5943410868252,41.6113603270596,15.));
#27879=CARTESIAN_POINT('Ctrl Pts',(-11.6674975352851,41.6839275596248,15.));
#27880=CARTESIAN_POINT('Ctrl Pts',(-11.7410945211992,41.7562341395977,15.));
#27881=CARTESIAN_POINT('Ctrl Pts',(-11.81512813804,41.8282796562569,15.));
#27882=CARTESIAN_POINT('Ctrl Pts',(-11.8895948153349,41.9000638152266,15.));
#27883=CARTESIAN_POINT('Ctrl Pts',(-11.9644914999263,41.9715865222182,15.));
#27884=CARTESIAN_POINT('Ctrl Pts',(-12.054880669507,42.0571002269437,15.));
#27885=CARTESIAN_POINT('Ctrl Pts',(-12.1307372881904,42.1280354231517,15.));
#27886=CARTESIAN_POINT('Ctrl Pts',(-12.1917619768791,42.18457517013,15.));
#27887=CARTESIAN_POINT('Ctrl Pts',(-12.2377212115623,42.2268628664988,15.));
#27888=CARTESIAN_POINT('Ctrl Pts',(-12.2684454652018,42.2550026135057,15.));
#27889=CARTESIAN_POINT('Ctrl Pts',(-1.38952890043916,43.9780537249529,0.));
#27890=CARTESIAN_POINT('Ctrl Pts',(-1.38952890043916,43.9780537249529,18.));
#27891=CARTESIAN_POINT('Ctrl Pts',(-1.39979132121931,43.9599253218252,0.));
#27892=CARTESIAN_POINT('Ctrl Pts',(-1.39979132121931,43.9599253218252,18.));
#27893=CARTESIAN_POINT('Ctrl Pts',(-1.42026781296156,43.9236568607623,0.));
#27894=CARTESIAN_POINT('Ctrl Pts',(-1.42026781296156,43.9236568607623,18.));
#27895=CARTESIAN_POINT('Ctrl Pts',(-1.45083750111682,43.8692192047561,0.));
#27896=CARTESIAN_POINT('Ctrl Pts',(-1.45083750111682,43.8692192047561,18.));
#27897=CARTESIAN_POINT('Ctrl Pts',(-1.49130689006066,43.7965657112708,0.));
#27898=CARTESIAN_POINT('Ctrl Pts',(-1.49130689006066,43.7965657112708,18.));
#27899=CARTESIAN_POINT('Ctrl Pts',(-1.54140922714765,43.7056321934163,0.));
#27900=CARTESIAN_POINT('Ctrl Pts',(-1.54140922714765,43.7056321934163,18.));
#27901=CARTESIAN_POINT('Ctrl Pts',(-1.59102591108103,43.6145820637333,0.));
#27902=CARTESIAN_POINT('Ctrl Pts',(-1.59102591108103,43.6145820637333,18.));
#27903=CARTESIAN_POINT('Ctrl Pts',(-1.64015515906648,43.5234155788248,0.));
#27904=CARTESIAN_POINT('Ctrl Pts',(-1.64015515906648,43.5234155788248,18.));
#27905=CARTESIAN_POINT('Ctrl Pts',(-1.68879465270608,43.4321333178711,0.));
#27906=CARTESIAN_POINT('Ctrl Pts',(-1.68879465270608,43.4321333178711,18.));
#27907=CARTESIAN_POINT('Ctrl Pts',(-1.73694151741124,43.3407363140236,0.));
#27908=CARTESIAN_POINT('Ctrl Pts',(-1.73694151741124,43.3407363140236,18.));
#27909=CARTESIAN_POINT('Ctrl Pts',(-1.78459244842769,43.2492259505872,0.));
#27910=CARTESIAN_POINT('Ctrl Pts',(-1.78459244842769,43.2492259505872,18.));
#27911=CARTESIAN_POINT('Ctrl Pts',(-1.83174385734711,43.1576038253643,0.));
#27912=CARTESIAN_POINT('Ctrl Pts',(-1.83174385734711,43.1576038253643,18.));
#27913=CARTESIAN_POINT('Ctrl Pts',(-1.87839202014609,43.065871623255,0.));
#27914=CARTESIAN_POINT('Ctrl Pts',(-1.87839202014609,43.065871623255,18.));
#27915=CARTESIAN_POINT('Ctrl Pts',(-1.92453321512436,42.9740309956624,0.));
#27916=CARTESIAN_POINT('Ctrl Pts',(-1.92453321512436,42.9740309956624,18.));
#27917=CARTESIAN_POINT('Ctrl Pts',(-1.97016390194216,42.8820834139973,0.));
#27918=CARTESIAN_POINT('Ctrl Pts',(-1.97016390194216,42.8820834139973,18.));
#27919=CARTESIAN_POINT('Ctrl Pts',(-2.01528067528089,42.7900301875309,0.));
#27920=CARTESIAN_POINT('Ctrl Pts',(-2.01528067528089,42.7900301875309,18.));
#27921=CARTESIAN_POINT('Ctrl Pts',(-2.05988014924519,42.6978725343209,0.));
#27922=CARTESIAN_POINT('Ctrl Pts',(-2.05988014924519,42.6978725343209,18.));
#27923=CARTESIAN_POINT('Ctrl Pts',(-2.10395886401771,42.6056116373456,0.));
#27924=CARTESIAN_POINT('Ctrl Pts',(-2.10395886401771,42.6056116373456,18.));
#27925=CARTESIAN_POINT('Ctrl Pts',(-2.14751319676745,42.5132487024335,0.));
#27926=CARTESIAN_POINT('Ctrl Pts',(-2.14751319676745,42.5132487024335,18.));
#27927=CARTESIAN_POINT('Ctrl Pts',(-2.19053924976737,42.4207850290047,0.));
#27928=CARTESIAN_POINT('Ctrl Pts',(-2.19053924976737,42.4207850290047,18.));
#27929=CARTESIAN_POINT('Ctrl Pts',(-2.233032874655,42.3282220118033,0.));
#27930=CARTESIAN_POINT('Ctrl Pts',(-2.233032874655,42.3282220118033,18.));
#27931=CARTESIAN_POINT('Ctrl Pts',(-2.27498976664774,42.2355611060784,0.));
#27932=CARTESIAN_POINT('Ctrl Pts',(-2.27498976664774,42.2355611060784,18.));
#27933=CARTESIAN_POINT('Ctrl Pts',(-2.31640554742808,42.1428038039937,0.));
#27934=CARTESIAN_POINT('Ctrl Pts',(-2.31640554742808,42.1428038039937,18.));
#27935=CARTESIAN_POINT('Ctrl Pts',(-2.35727584066429,42.0499516093661,0.));
#27936=CARTESIAN_POINT('Ctrl Pts',(-2.35727584066429,42.0499516093661,18.));
#27937=CARTESIAN_POINT('Ctrl Pts',(-2.39759639399648,41.9570060084039,0.));
#27938=CARTESIAN_POINT('Ctrl Pts',(-2.39759639399648,41.9570060084039,18.));
#27939=CARTESIAN_POINT('Ctrl Pts',(-2.437363014342,41.8639684667923,0.));
#27940=CARTESIAN_POINT('Ctrl Pts',(-2.437363014342,41.8639684667923,18.));
#27941=CARTESIAN_POINT('Ctrl Pts',(-2.47657137427693,41.7708404467533,0.));
#27942=CARTESIAN_POINT('Ctrl Pts',(-2.47657137427693,41.7708404467533,18.));
#27943=CARTESIAN_POINT('Ctrl Pts',(-2.51521684674477,41.6776234194583,0.));
#27944=CARTESIAN_POINT('Ctrl Pts',(-2.51521684674477,41.6776234194583,18.));
#27945=CARTESIAN_POINT('Ctrl Pts',(-2.55329436064184,41.5843188786284,0.));
#27946=CARTESIAN_POINT('Ctrl Pts',(-2.55329436064184,41.5843188786284,18.));
#27947=CARTESIAN_POINT('Ctrl Pts',(-2.59079818040171,41.4909283577703,0.));
#27948=CARTESIAN_POINT('Ctrl Pts',(-2.59079818040171,41.4909283577703,18.));
#27949=CARTESIAN_POINT('Ctrl Pts',(-2.62772200460656,41.3974534325936,0.));
#27950=CARTESIAN_POINT('Ctrl Pts',(-2.62772200460656,41.3974534325936,18.));
#27951=CARTESIAN_POINT('Ctrl Pts',(-2.66405934050118,41.3038957096306,0.));
#27952=CARTESIAN_POINT('Ctrl Pts',(-2.66405934050118,41.3038957096306,18.));
#27953=CARTESIAN_POINT('Ctrl Pts',(-2.69980383625015,41.2102568187956,0.));
#27954=CARTESIAN_POINT('Ctrl Pts',(-2.69980383625015,41.2102568187956,18.));
#27955=CARTESIAN_POINT('Ctrl Pts',(-2.73494956725005,41.1165384061145,0.));
#27956=CARTESIAN_POINT('Ctrl Pts',(-2.73494956725005,41.1165384061145,18.));
#27957=CARTESIAN_POINT('Ctrl Pts',(-2.76949151194863,41.0227421242398,0.));
#27958=CARTESIAN_POINT('Ctrl Pts',(-2.76949151194863,41.0227421242398,18.));
#27959=CARTESIAN_POINT('Ctrl Pts',(-2.80342531768405,40.9288696352159,0.));
#27960=CARTESIAN_POINT('Ctrl Pts',(-2.80342531768405,40.9288696352159,18.));
#27961=CARTESIAN_POINT('Ctrl Pts',(-2.83674635946679,40.8349226258683,0.));
#27962=CARTESIAN_POINT('Ctrl Pts',(-2.83674635946679,40.8349226258683,18.));
#27963=CARTESIAN_POINT('Ctrl Pts',(-2.86944892209898,40.7409028213129,0.));
#27964=CARTESIAN_POINT('Ctrl Pts',(-2.86944892209898,40.7409028213129,18.));
#27965=CARTESIAN_POINT('Ctrl Pts',(-2.90152548734343,40.6468119976928,0.));
#27966=CARTESIAN_POINT('Ctrl Pts',(-2.90152548734343,40.6468119976928,18.));
#27967=CARTESIAN_POINT('Ctrl Pts',(-2.93296560822893,40.5526520010651,0.));
#27968=CARTESIAN_POINT('Ctrl Pts',(-2.93296560822893,40.5526520010651,18.));
#27969=CARTESIAN_POINT('Ctrl Pts',(-2.96375636417322,40.4584247445196,0.));
#27970=CARTESIAN_POINT('Ctrl Pts',(-2.96375636417322,40.4584247445196,18.));
#27971=CARTESIAN_POINT('Ctrl Pts',(-2.99388446458219,40.3641321823444,0.));
#27972=CARTESIAN_POINT('Ctrl Pts',(-2.99388446458219,40.3641321823444,18.));
#27973=CARTESIAN_POINT('Ctrl Pts',(-3.02333808901595,40.2697762886113,0.));
#27974=CARTESIAN_POINT('Ctrl Pts',(-3.02333808901595,40.2697762886113,18.));
#27975=CARTESIAN_POINT('Ctrl Pts',(-3.0521084742307,40.1753590391515,0.));
#27976=CARTESIAN_POINT('Ctrl Pts',(-3.0521084742307,40.1753590391515,18.));
#27977=CARTESIAN_POINT('Ctrl Pts',(-3.08019251155015,40.0808823811787,0.));
#27978=CARTESIAN_POINT('Ctrl Pts',(-3.08019251155015,40.0808823811787,18.));
#27979=CARTESIAN_POINT('Ctrl Pts',(-3.10759149802908,39.9863482523153,0.));
#27980=CARTESIAN_POINT('Ctrl Pts',(-3.10759149802908,39.9863482523153,18.));
#27981=CARTESIAN_POINT('Ctrl Pts',(-3.13430604330356,39.8917586491576,0.));
#27982=CARTESIAN_POINT('Ctrl Pts',(-3.13430604330356,39.8917586491576,18.));
#27983=CARTESIAN_POINT('Ctrl Pts',(-3.16033160752804,39.7971156880138,0.));
#27984=CARTESIAN_POINT('Ctrl Pts',(-3.16033160752804,39.7971156880138,18.));
#27985=CARTESIAN_POINT('Ctrl Pts',(-3.18565465503835,39.7024216585552,0.));
#27986=CARTESIAN_POINT('Ctrl Pts',(-3.18565465503835,39.7024216585552,18.));
#27987=CARTESIAN_POINT('Ctrl Pts',(-3.21024640045595,39.607679107639,0.));
#27988=CARTESIAN_POINT('Ctrl Pts',(-3.21024640045595,39.607679107639,18.));
#27989=CARTESIAN_POINT('Ctrl Pts',(-3.23406609691661,39.5128908052622,0.));
#27990=CARTESIAN_POINT('Ctrl Pts',(-3.23406609691661,39.5128908052622,18.));
#27991=CARTESIAN_POINT('Ctrl Pts',(-3.25707264313388,39.4180596080755,0.));
#27992=CARTESIAN_POINT('Ctrl Pts',(-3.25707264313388,39.4180596080755,18.));
#27993=CARTESIAN_POINT('Ctrl Pts',(-3.27923485388117,39.3231883392913,0.));
#27994=CARTESIAN_POINT('Ctrl Pts',(-3.27923485388117,39.3231883392913,18.));
#27995=CARTESIAN_POINT('Ctrl Pts',(-3.30054018081687,39.2282796893977,0.));
#27996=CARTESIAN_POINT('Ctrl Pts',(-3.30054018081687,39.2282796893977,18.));
#27997=CARTESIAN_POINT('Ctrl Pts',(-3.32100933979557,39.1333360409949,0.));
#27998=CARTESIAN_POINT('Ctrl Pts',(-3.32100933979557,39.1333360409949,18.));
#27999=CARTESIAN_POINT('Ctrl Pts',(-3.34068601264472,39.0383596151636,0.));
#28000=CARTESIAN_POINT('Ctrl Pts',(-3.34068601264472,39.0383596151636,18.));
#28001=CARTESIAN_POINT('Ctrl Pts',(-3.35960922799481,38.9433528420174,0.));
#28002=CARTESIAN_POINT('Ctrl Pts',(-3.35960922799481,38.9433528420174,18.));
#28003=CARTESIAN_POINT('Ctrl Pts',(-3.37778863054482,38.8483186930884,0.));
#28004=CARTESIAN_POINT('Ctrl Pts',(-3.37778863054482,38.8483186930884,18.));
#28005=CARTESIAN_POINT('Ctrl Pts',(-3.39518333281818,38.7532609709905,0.));
#28006=CARTESIAN_POINT('Ctrl Pts',(-3.39518333281818,38.7532609709905,18.));
#28007=CARTESIAN_POINT('Ctrl Pts',(-3.41166717511901,38.6581847668347,0.));
#28008=CARTESIAN_POINT('Ctrl Pts',(-3.41166717511901,38.6581847668347,18.));
#28009=CARTESIAN_POINT('Ctrl Pts',(-3.42705871084997,38.5630961226878,0.));
#28010=CARTESIAN_POINT('Ctrl Pts',(-3.42705871084997,38.5630961226878,18.));
#28011=CARTESIAN_POINT('Ctrl Pts',(-3.44118343200303,38.4680013094732,0.));
#28012=CARTESIAN_POINT('Ctrl Pts',(-3.44118343200303,38.4680013094732,18.));
#28013=CARTESIAN_POINT('Ctrl Pts',(-3.45393053211023,38.3729061502716,0.));
#28014=CARTESIAN_POINT('Ctrl Pts',(-3.45393053211023,38.3729061502716,18.));
#28015=CARTESIAN_POINT('Ctrl Pts',(-3.46530185256872,38.2778154909527,0.));
#28016=CARTESIAN_POINT('Ctrl Pts',(-3.46530185256872,38.2778154909527,18.));
#28017=CARTESIAN_POINT('Ctrl Pts',(-3.47549027265411,38.1827321816559,0.));
#28018=CARTESIAN_POINT('Ctrl Pts',(-3.47549027265411,38.1827321816559,18.));
#28019=CARTESIAN_POINT('Ctrl Pts',(-3.48478279878233,38.0876589224537,0.));
#28020=CARTESIAN_POINT('Ctrl Pts',(-3.48478279878233,38.0876589224537,18.));
#28021=CARTESIAN_POINT('Ctrl Pts',(-3.49340804454645,37.9926009950482,0.));
#28022=CARTESIAN_POINT('Ctrl Pts',(-3.49340804454645,37.9926009950482,18.));
#28023=CARTESIAN_POINT('Ctrl Pts',(-3.50139628556083,37.8975688353863,0.));
#28024=CARTESIAN_POINT('Ctrl Pts',(-3.50139628556083,37.8975688353863,18.));
#28025=CARTESIAN_POINT('Ctrl Pts',(-3.50844720825128,37.8025803811856,0.));
#28026=CARTESIAN_POINT('Ctrl Pts',(-3.50844720825128,37.8025803811856,18.));
#28027=CARTESIAN_POINT('Ctrl Pts',(-3.51375922979957,37.7076643105286,0.));
#28028=CARTESIAN_POINT('Ctrl Pts',(-3.51375922979957,37.7076643105286,18.));
#28029=CARTESIAN_POINT('Ctrl Pts',(-3.51624243734645,37.6128545966533,0.));
#28030=CARTESIAN_POINT('Ctrl Pts',(-3.51624243734645,37.6128545966533,18.));
#28031=CARTESIAN_POINT('Ctrl Pts',(-3.51508109065209,37.5371179004295,0.));
#28032=CARTESIAN_POINT('Ctrl Pts',(-3.51508109065209,37.5371179004295,18.));
#28033=CARTESIAN_POINT('Ctrl Pts',(-3.51204731876361,37.4803889700239,0.));
#28034=CARTESIAN_POINT('Ctrl Pts',(-3.51204731876361,37.4803889700239,18.));
#28035=CARTESIAN_POINT('Ctrl Pts',(-3.50901346997657,37.4426037737699,0.));
#28036=CARTESIAN_POINT('Ctrl Pts',(-3.50901346997657,37.4426037737699,18.));
#28037=CARTESIAN_POINT('Ctrl Pts',(-3.50724370857673,37.4237196983922,0.));
#28038=CARTESIAN_POINT('Ctrl Pts',(-3.50724370857673,37.4237196983922,18.));
#28039=CARTESIAN_POINT('',(-1.38952890043929,43.9780537249529,0.));
#28040=CARTESIAN_POINT('Ctrl Pts',(-3.50724370857673,37.4237196983922,0.));
#28041=CARTESIAN_POINT('Ctrl Pts',(-3.50901346997657,37.4426037737699,0.));
#28042=CARTESIAN_POINT('Ctrl Pts',(-3.51204731876361,37.4803889700239,0.));
#28043=CARTESIAN_POINT('Ctrl Pts',(-3.51508109065209,37.5371179004295,0.));
#28044=CARTESIAN_POINT('Ctrl Pts',(-3.51624243734645,37.6128545966533,0.));
#28045=CARTESIAN_POINT('Ctrl Pts',(-3.51375922979957,37.7076643105286,0.));
#28046=CARTESIAN_POINT('Ctrl Pts',(-3.50844720825128,37.8025803811856,0.));
#28047=CARTESIAN_POINT('Ctrl Pts',(-3.50139628556083,37.8975688353863,0.));
#28048=CARTESIAN_POINT('Ctrl Pts',(-3.49340804454645,37.9926009950482,0.));
#28049=CARTESIAN_POINT('Ctrl Pts',(-3.48478279878233,38.0876589224537,0.));
#28050=CARTESIAN_POINT('Ctrl Pts',(-3.47549027265411,38.1827321816559,0.));
#28051=CARTESIAN_POINT('Ctrl Pts',(-3.46530185256872,38.2778154909527,0.));
#28052=CARTESIAN_POINT('Ctrl Pts',(-3.45393053211023,38.3729061502716,0.));
#28053=CARTESIAN_POINT('Ctrl Pts',(-3.44118343200303,38.4680013094732,0.));
#28054=CARTESIAN_POINT('Ctrl Pts',(-3.42705871084997,38.5630961226878,0.));
#28055=CARTESIAN_POINT('Ctrl Pts',(-3.41166717511901,38.6581847668347,0.));
#28056=CARTESIAN_POINT('Ctrl Pts',(-3.39518333281818,38.7532609709905,0.));
#28057=CARTESIAN_POINT('Ctrl Pts',(-3.37778863054482,38.8483186930884,0.));
#28058=CARTESIAN_POINT('Ctrl Pts',(-3.35960922799481,38.9433528420174,0.));
#28059=CARTESIAN_POINT('Ctrl Pts',(-3.34068601264472,39.0383596151636,0.));
#28060=CARTESIAN_POINT('Ctrl Pts',(-3.32100933979557,39.1333360409949,0.));
#28061=CARTESIAN_POINT('Ctrl Pts',(-3.30054018081687,39.2282796893977,0.));
#28062=CARTESIAN_POINT('Ctrl Pts',(-3.27923485388117,39.3231883392913,0.));
#28063=CARTESIAN_POINT('Ctrl Pts',(-3.25707264313388,39.4180596080755,0.));
#28064=CARTESIAN_POINT('Ctrl Pts',(-3.23406609691661,39.5128908052622,0.));
#28065=CARTESIAN_POINT('Ctrl Pts',(-3.21024640045595,39.607679107639,0.));
#28066=CARTESIAN_POINT('Ctrl Pts',(-3.18565465503835,39.7024216585552,0.));
#28067=CARTESIAN_POINT('Ctrl Pts',(-3.16033160752804,39.7971156880138,0.));
#28068=CARTESIAN_POINT('Ctrl Pts',(-3.13430604330356,39.8917586491576,0.));
#28069=CARTESIAN_POINT('Ctrl Pts',(-3.10759149802908,39.9863482523153,0.));
#28070=CARTESIAN_POINT('Ctrl Pts',(-3.08019251155015,40.0808823811787,0.));
#28071=CARTESIAN_POINT('Ctrl Pts',(-3.0521084742307,40.1753590391515,0.));
#28072=CARTESIAN_POINT('Ctrl Pts',(-3.02333808901595,40.2697762886113,0.));
#28073=CARTESIAN_POINT('Ctrl Pts',(-2.99388446458219,40.3641321823444,0.));
#28074=CARTESIAN_POINT('Ctrl Pts',(-2.96375636417322,40.4584247445196,0.));
#28075=CARTESIAN_POINT('Ctrl Pts',(-2.93296560822893,40.5526520010651,0.));
#28076=CARTESIAN_POINT('Ctrl Pts',(-2.90152548734343,40.6468119976928,0.));
#28077=CARTESIAN_POINT('Ctrl Pts',(-2.86944892209898,40.7409028213129,0.));
#28078=CARTESIAN_POINT('Ctrl Pts',(-2.83674635946679,40.8349226258683,0.));
#28079=CARTESIAN_POINT('Ctrl Pts',(-2.80342531768405,40.9288696352159,0.));
#28080=CARTESIAN_POINT('Ctrl Pts',(-2.76949151194863,41.0227421242398,0.));
#28081=CARTESIAN_POINT('Ctrl Pts',(-2.73494956725005,41.1165384061145,0.));
#28082=CARTESIAN_POINT('Ctrl Pts',(-2.69980383625015,41.2102568187956,0.));
#28083=CARTESIAN_POINT('Ctrl Pts',(-2.66405934050118,41.3038957096306,0.));
#28084=CARTESIAN_POINT('Ctrl Pts',(-2.62772200460656,41.3974534325936,0.));
#28085=CARTESIAN_POINT('Ctrl Pts',(-2.59079818040171,41.4909283577703,0.));
#28086=CARTESIAN_POINT('Ctrl Pts',(-2.55329436064184,41.5843188786284,0.));
#28087=CARTESIAN_POINT('Ctrl Pts',(-2.51521684674477,41.6776234194583,0.));
#28088=CARTESIAN_POINT('Ctrl Pts',(-2.47657137427693,41.7708404467533,0.));
#28089=CARTESIAN_POINT('Ctrl Pts',(-2.437363014342,41.8639684667923,0.));
#28090=CARTESIAN_POINT('Ctrl Pts',(-2.39759639399648,41.9570060084039,0.));
#28091=CARTESIAN_POINT('Ctrl Pts',(-2.35727584066429,42.0499516093661,0.));
#28092=CARTESIAN_POINT('Ctrl Pts',(-2.31640554742808,42.1428038039937,0.));
#28093=CARTESIAN_POINT('Ctrl Pts',(-2.27498976664774,42.2355611060784,0.));
#28094=CARTESIAN_POINT('Ctrl Pts',(-2.233032874655,42.3282220118033,0.));
#28095=CARTESIAN_POINT('Ctrl Pts',(-2.19053924976737,42.4207850290047,0.));
#28096=CARTESIAN_POINT('Ctrl Pts',(-2.14751319676745,42.5132487024335,0.));
#28097=CARTESIAN_POINT('Ctrl Pts',(-2.10395886401771,42.6056116373456,0.));
#28098=CARTESIAN_POINT('Ctrl Pts',(-2.05988014924519,42.6978725343209,0.));
#28099=CARTESIAN_POINT('Ctrl Pts',(-2.01528067528089,42.7900301875309,0.));
#28100=CARTESIAN_POINT('Ctrl Pts',(-1.97016390194216,42.8820834139973,0.));
#28101=CARTESIAN_POINT('Ctrl Pts',(-1.92453321512436,42.9740309956624,0.));
#28102=CARTESIAN_POINT('Ctrl Pts',(-1.87839202014609,43.065871623255,0.));
#28103=CARTESIAN_POINT('Ctrl Pts',(-1.83174385734711,43.1576038253643,0.));
#28104=CARTESIAN_POINT('Ctrl Pts',(-1.78459244842769,43.2492259505872,0.));
#28105=CARTESIAN_POINT('Ctrl Pts',(-1.73694151741124,43.3407363140236,0.));
#28106=CARTESIAN_POINT('Ctrl Pts',(-1.68879465270608,43.4321333178711,0.));
#28107=CARTESIAN_POINT('Ctrl Pts',(-1.64015515906648,43.5234155788248,0.));
#28108=CARTESIAN_POINT('Ctrl Pts',(-1.59102591108103,43.6145820637333,0.));
#28109=CARTESIAN_POINT('Ctrl Pts',(-1.53148589036097,43.7238422193529,0.));
#28110=CARTESIAN_POINT('Ctrl Pts',(-1.48126213998558,43.8147465842503,0.));
#28111=CARTESIAN_POINT('Ctrl Pts',(-1.44069595482723,43.8873767449247,0.));
#28112=CARTESIAN_POINT('Ctrl Pts',(-1.41005374202872,43.9417969186811,0.));
#28113=CARTESIAN_POINT('Ctrl Pts',(-1.38952890043916,43.9780537249529,0.));
#28114=CARTESIAN_POINT('',(-1.38952890043929,43.9780537249529,15.));
#28115=CARTESIAN_POINT('Ctrl Pts',(-1.38952890043916,43.9780537249529,15.));
#28116=CARTESIAN_POINT('Ctrl Pts',(-1.39979132121931,43.9599253218252,15.));
#28117=CARTESIAN_POINT('Ctrl Pts',(-1.42026781296156,43.9236568607623,15.));
#28118=CARTESIAN_POINT('Ctrl Pts',(-1.45083750111682,43.8692192047561,15.));
#28119=CARTESIAN_POINT('Ctrl Pts',(-1.49130689006066,43.7965657112708,15.));
#28120=CARTESIAN_POINT('Ctrl Pts',(-1.54140922714765,43.7056321934163,15.));
#28121=CARTESIAN_POINT('Ctrl Pts',(-1.59102591108103,43.6145820637333,15.));
#28122=CARTESIAN_POINT('Ctrl Pts',(-1.64015515906648,43.5234155788248,15.));
#28123=CARTESIAN_POINT('Ctrl Pts',(-1.68879465270608,43.4321333178711,15.));
#28124=CARTESIAN_POINT('Ctrl Pts',(-1.73694151741124,43.3407363140236,15.));
#28125=CARTESIAN_POINT('Ctrl Pts',(-1.78459244842769,43.2492259505872,15.));
#28126=CARTESIAN_POINT('Ctrl Pts',(-1.83174385734711,43.1576038253643,15.));
#28127=CARTESIAN_POINT('Ctrl Pts',(-1.87839202014609,43.065871623255,15.));
#28128=CARTESIAN_POINT('Ctrl Pts',(-1.92453321512436,42.9740309956624,15.));
#28129=CARTESIAN_POINT('Ctrl Pts',(-1.97016390194216,42.8820834139973,15.));
#28130=CARTESIAN_POINT('Ctrl Pts',(-2.01528067528089,42.7900301875309,15.));
#28131=CARTESIAN_POINT('Ctrl Pts',(-2.05988014924519,42.6978725343209,15.));
#28132=CARTESIAN_POINT('Ctrl Pts',(-2.10395886401771,42.6056116373456,15.));
#28133=CARTESIAN_POINT('Ctrl Pts',(-2.14751319676745,42.5132487024335,15.));
#28134=CARTESIAN_POINT('Ctrl Pts',(-2.19053924976737,42.4207850290047,15.));
#28135=CARTESIAN_POINT('Ctrl Pts',(-2.233032874655,42.3282220118033,15.));
#28136=CARTESIAN_POINT('Ctrl Pts',(-2.27498976664774,42.2355611060784,15.));
#28137=CARTESIAN_POINT('Ctrl Pts',(-2.31640554742808,42.1428038039937,15.));
#28138=CARTESIAN_POINT('Ctrl Pts',(-2.35727584066429,42.0499516093661,15.));
#28139=CARTESIAN_POINT('Ctrl Pts',(-2.39759639399648,41.9570060084039,15.));
#28140=CARTESIAN_POINT('Ctrl Pts',(-2.437363014342,41.8639684667923,15.));
#28141=CARTESIAN_POINT('Ctrl Pts',(-2.47657137427693,41.7708404467533,15.));
#28142=CARTESIAN_POINT('Ctrl Pts',(-2.51521684674477,41.6776234194583,15.));
#28143=CARTESIAN_POINT('Ctrl Pts',(-2.55329436064184,41.5843188786284,15.));
#28144=CARTESIAN_POINT('Ctrl Pts',(-2.59079818040171,41.4909283577703,15.));
#28145=CARTESIAN_POINT('Ctrl Pts',(-2.62772200460656,41.3974534325936,15.));
#28146=CARTESIAN_POINT('Ctrl Pts',(-2.66405934050118,41.3038957096306,15.));
#28147=CARTESIAN_POINT('Ctrl Pts',(-2.69980383625015,41.2102568187956,15.));
#28148=CARTESIAN_POINT('Ctrl Pts',(-2.73494956725005,41.1165384061145,15.));
#28149=CARTESIAN_POINT('Ctrl Pts',(-2.76949151194863,41.0227421242398,15.));
#28150=CARTESIAN_POINT('Ctrl Pts',(-2.80342531768405,40.9288696352159,15.));
#28151=CARTESIAN_POINT('Ctrl Pts',(-2.83674635946679,40.8349226258683,15.));
#28152=CARTESIAN_POINT('Ctrl Pts',(-2.86944892209898,40.7409028213129,15.));
#28153=CARTESIAN_POINT('Ctrl Pts',(-2.90152548734343,40.6468119976928,15.));
#28154=CARTESIAN_POINT('Ctrl Pts',(-2.93296560822893,40.5526520010651,15.));
#28155=CARTESIAN_POINT('Ctrl Pts',(-2.96375636417322,40.4584247445196,15.));
#28156=CARTESIAN_POINT('Ctrl Pts',(-2.99388446458219,40.3641321823444,15.));
#28157=CARTESIAN_POINT('Ctrl Pts',(-3.02333808901595,40.2697762886113,15.));
#28158=CARTESIAN_POINT('Ctrl Pts',(-3.0521084742307,40.1753590391515,15.));
#28159=CARTESIAN_POINT('Ctrl Pts',(-3.08019251155015,40.0808823811787,15.));
#28160=CARTESIAN_POINT('Ctrl Pts',(-3.10759149802908,39.9863482523153,15.));
#28161=CARTESIAN_POINT('Ctrl Pts',(-3.13430604330356,39.8917586491576,15.));
#28162=CARTESIAN_POINT('Ctrl Pts',(-3.16033160752804,39.7971156880138,15.));
#28163=CARTESIAN_POINT('Ctrl Pts',(-3.18565465503835,39.7024216585552,15.));
#28164=CARTESIAN_POINT('Ctrl Pts',(-3.21024640045595,39.607679107639,15.));
#28165=CARTESIAN_POINT('Ctrl Pts',(-3.23406609691661,39.5128908052622,15.));
#28166=CARTESIAN_POINT('Ctrl Pts',(-3.25707264313388,39.4180596080755,15.));
#28167=CARTESIAN_POINT('Ctrl Pts',(-3.27923485388117,39.3231883392913,15.));
#28168=CARTESIAN_POINT('Ctrl Pts',(-3.30054018081687,39.2282796893977,15.));
#28169=CARTESIAN_POINT('Ctrl Pts',(-3.32100933979557,39.1333360409949,15.));
#28170=CARTESIAN_POINT('Ctrl Pts',(-3.34068601264472,39.0383596151636,15.));
#28171=CARTESIAN_POINT('Ctrl Pts',(-3.35960922799481,38.9433528420174,15.));
#28172=CARTESIAN_POINT('Ctrl Pts',(-3.37778863054482,38.8483186930884,15.));
#28173=CARTESIAN_POINT('Ctrl Pts',(-3.39518333281818,38.7532609709905,15.));
#28174=CARTESIAN_POINT('Ctrl Pts',(-3.41166717511901,38.6581847668347,15.));
#28175=CARTESIAN_POINT('Ctrl Pts',(-3.42705871084997,38.5630961226878,15.));
#28176=CARTESIAN_POINT('Ctrl Pts',(-3.44118343200303,38.4680013094732,15.));
#28177=CARTESIAN_POINT('Ctrl Pts',(-3.45393053211023,38.3729061502716,15.));
#28178=CARTESIAN_POINT('Ctrl Pts',(-3.46530185256872,38.2778154909527,15.));
#28179=CARTESIAN_POINT('Ctrl Pts',(-3.47549027265411,38.1827321816559,15.));
#28180=CARTESIAN_POINT('Ctrl Pts',(-3.48478279878233,38.0876589224537,15.));
#28181=CARTESIAN_POINT('Ctrl Pts',(-3.49340804454645,37.9926009950482,15.));
#28182=CARTESIAN_POINT('Ctrl Pts',(-3.50139628556083,37.8975688353863,15.));
#28183=CARTESIAN_POINT('Ctrl Pts',(-3.50844720825128,37.8025803811856,15.));
#28184=CARTESIAN_POINT('Ctrl Pts',(-3.51375922979957,37.7076643105286,15.));
#28185=CARTESIAN_POINT('Ctrl Pts',(-3.51624243734645,37.6128545966533,15.));
#28186=CARTESIAN_POINT('Ctrl Pts',(-3.51508109065209,37.5371179004295,15.));
#28187=CARTESIAN_POINT('Ctrl Pts',(-3.51204731876361,37.4803889700239,15.));
#28188=CARTESIAN_POINT('Ctrl Pts',(-3.50901346997657,37.4426037737699,15.));
#28189=CARTESIAN_POINT('Ctrl Pts',(-3.50724370857673,37.4237196983922,15.));
#28190=CARTESIAN_POINT('',(-1.38952890043929,43.9780537249529,0.));
#28191=CARTESIAN_POINT('Origin',(0.,1.13331566353736E-11,0.));
#28192=CARTESIAN_POINT('',(1.38952890043917,43.9780537249529,0.));
#28193=CARTESIAN_POINT('Origin',(0.,1.13331566353736E-11,0.));
#28194=CARTESIAN_POINT('',(1.38952890043917,43.9780537249529,15.));
#28195=CARTESIAN_POINT('Origin',(0.,1.13331566353736E-11,15.));
#28196=CARTESIAN_POINT('',(1.38952890043917,43.9780537249529,0.));
#28197=CARTESIAN_POINT('Ctrl Pts',(3.50724370857673,37.4237196983923,0.));
#28198=CARTESIAN_POINT('Ctrl Pts',(3.50724370857673,37.4237196983923,18.));
#28199=CARTESIAN_POINT('Ctrl Pts',(3.50901346997657,37.4426037737699,0.));
#28200=CARTESIAN_POINT('Ctrl Pts',(3.50901346997657,37.4426037737699,18.));
#28201=CARTESIAN_POINT('Ctrl Pts',(3.51204731876361,37.4803889700239,0.));
#28202=CARTESIAN_POINT('Ctrl Pts',(3.51204731876361,37.4803889700239,18.));
#28203=CARTESIAN_POINT('Ctrl Pts',(3.5150810906521,37.5371179004295,0.));
#28204=CARTESIAN_POINT('Ctrl Pts',(3.5150810906521,37.5371179004295,18.));
#28205=CARTESIAN_POINT('Ctrl Pts',(3.51624243734645,37.6128545966533,0.));
#28206=CARTESIAN_POINT('Ctrl Pts',(3.51624243734645,37.6128545966533,18.));
#28207=CARTESIAN_POINT('Ctrl Pts',(3.51375922979958,37.7076643105286,0.));
#28208=CARTESIAN_POINT('Ctrl Pts',(3.51375922979958,37.7076643105286,18.));
#28209=CARTESIAN_POINT('Ctrl Pts',(3.50844720825128,37.8025803811856,0.));
#28210=CARTESIAN_POINT('Ctrl Pts',(3.50844720825128,37.8025803811856,18.));
#28211=CARTESIAN_POINT('Ctrl Pts',(3.50139628556084,37.8975688353863,0.));
#28212=CARTESIAN_POINT('Ctrl Pts',(3.50139628556084,37.8975688353863,18.));
#28213=CARTESIAN_POINT('Ctrl Pts',(3.49340804454646,37.9926009950482,0.));
#28214=CARTESIAN_POINT('Ctrl Pts',(3.49340804454646,37.9926009950482,18.));
#28215=CARTESIAN_POINT('Ctrl Pts',(3.48478279878234,38.0876589224537,0.));
#28216=CARTESIAN_POINT('Ctrl Pts',(3.48478279878234,38.0876589224537,18.));
#28217=CARTESIAN_POINT('Ctrl Pts',(3.47549027265412,38.1827321816559,0.));
#28218=CARTESIAN_POINT('Ctrl Pts',(3.47549027265412,38.1827321816559,18.));
#28219=CARTESIAN_POINT('Ctrl Pts',(3.46530185256873,38.2778154909527,0.));
#28220=CARTESIAN_POINT('Ctrl Pts',(3.46530185256873,38.2778154909527,18.));
#28221=CARTESIAN_POINT('Ctrl Pts',(3.45393053211023,38.3729061502716,0.));
#28222=CARTESIAN_POINT('Ctrl Pts',(3.45393053211023,38.3729061502716,18.));
#28223=CARTESIAN_POINT('Ctrl Pts',(3.44118343200303,38.4680013094732,0.));
#28224=CARTESIAN_POINT('Ctrl Pts',(3.44118343200303,38.4680013094732,18.));
#28225=CARTESIAN_POINT('Ctrl Pts',(3.42705871084997,38.5630961226878,0.));
#28226=CARTESIAN_POINT('Ctrl Pts',(3.42705871084997,38.5630961226878,18.));
#28227=CARTESIAN_POINT('Ctrl Pts',(3.41166717511901,38.6581847668347,0.));
#28228=CARTESIAN_POINT('Ctrl Pts',(3.41166717511901,38.6581847668347,18.));
#28229=CARTESIAN_POINT('Ctrl Pts',(3.39518333281818,38.7532609709905,0.));
#28230=CARTESIAN_POINT('Ctrl Pts',(3.39518333281818,38.7532609709905,18.));
#28231=CARTESIAN_POINT('Ctrl Pts',(3.37778863054482,38.8483186930884,0.));
#28232=CARTESIAN_POINT('Ctrl Pts',(3.37778863054482,38.8483186930884,18.));
#28233=CARTESIAN_POINT('Ctrl Pts',(3.35960922799481,38.9433528420174,0.));
#28234=CARTESIAN_POINT('Ctrl Pts',(3.35960922799481,38.9433528420174,18.));
#28235=CARTESIAN_POINT('Ctrl Pts',(3.34068601264472,39.0383596151636,0.));
#28236=CARTESIAN_POINT('Ctrl Pts',(3.34068601264472,39.0383596151636,18.));
#28237=CARTESIAN_POINT('Ctrl Pts',(3.32100933979558,39.1333360409949,0.));
#28238=CARTESIAN_POINT('Ctrl Pts',(3.32100933979558,39.1333360409949,18.));
#28239=CARTESIAN_POINT('Ctrl Pts',(3.30054018081688,39.2282796893977,0.));
#28240=CARTESIAN_POINT('Ctrl Pts',(3.30054018081688,39.2282796893977,18.));
#28241=CARTESIAN_POINT('Ctrl Pts',(3.27923485388118,39.3231883392913,0.));
#28242=CARTESIAN_POINT('Ctrl Pts',(3.27923485388118,39.3231883392913,18.));
#28243=CARTESIAN_POINT('Ctrl Pts',(3.25707264313388,39.4180596080755,0.));
#28244=CARTESIAN_POINT('Ctrl Pts',(3.25707264313388,39.4180596080755,18.));
#28245=CARTESIAN_POINT('Ctrl Pts',(3.23406609691661,39.5128908052622,0.));
#28246=CARTESIAN_POINT('Ctrl Pts',(3.23406609691661,39.5128908052622,18.));
#28247=CARTESIAN_POINT('Ctrl Pts',(3.21024640045595,39.607679107639,0.));
#28248=CARTESIAN_POINT('Ctrl Pts',(3.21024640045595,39.607679107639,18.));
#28249=CARTESIAN_POINT('Ctrl Pts',(3.18565465503836,39.7024216585552,0.));
#28250=CARTESIAN_POINT('Ctrl Pts',(3.18565465503836,39.7024216585552,18.));
#28251=CARTESIAN_POINT('Ctrl Pts',(3.16033160752804,39.7971156880138,0.));
#28252=CARTESIAN_POINT('Ctrl Pts',(3.16033160752804,39.7971156880138,18.));
#28253=CARTESIAN_POINT('Ctrl Pts',(3.13430604330356,39.8917586491576,0.));
#28254=CARTESIAN_POINT('Ctrl Pts',(3.13430604330356,39.8917586491576,18.));
#28255=CARTESIAN_POINT('Ctrl Pts',(3.10759149802908,39.9863482523153,0.));
#28256=CARTESIAN_POINT('Ctrl Pts',(3.10759149802908,39.9863482523153,18.));
#28257=CARTESIAN_POINT('Ctrl Pts',(3.08019251155016,40.0808823811787,0.));
#28258=CARTESIAN_POINT('Ctrl Pts',(3.08019251155016,40.0808823811787,18.));
#28259=CARTESIAN_POINT('Ctrl Pts',(3.05210847423071,40.1753590391515,0.));
#28260=CARTESIAN_POINT('Ctrl Pts',(3.05210847423071,40.1753590391515,18.));
#28261=CARTESIAN_POINT('Ctrl Pts',(3.02333808901595,40.2697762886113,0.));
#28262=CARTESIAN_POINT('Ctrl Pts',(3.02333808901595,40.2697762886113,18.));
#28263=CARTESIAN_POINT('Ctrl Pts',(2.9938844645822,40.3641321823444,0.));
#28264=CARTESIAN_POINT('Ctrl Pts',(2.9938844645822,40.3641321823444,18.));
#28265=CARTESIAN_POINT('Ctrl Pts',(2.96375636417323,40.4584247445196,0.));
#28266=CARTESIAN_POINT('Ctrl Pts',(2.96375636417323,40.4584247445196,18.));
#28267=CARTESIAN_POINT('Ctrl Pts',(2.93296560822894,40.5526520010651,0.));
#28268=CARTESIAN_POINT('Ctrl Pts',(2.93296560822894,40.5526520010651,18.));
#28269=CARTESIAN_POINT('Ctrl Pts',(2.90152548734343,40.6468119976928,0.));
#28270=CARTESIAN_POINT('Ctrl Pts',(2.90152548734343,40.6468119976928,18.));
#28271=CARTESIAN_POINT('Ctrl Pts',(2.86944892209898,40.7409028213129,0.));
#28272=CARTESIAN_POINT('Ctrl Pts',(2.86944892209898,40.7409028213129,18.));
#28273=CARTESIAN_POINT('Ctrl Pts',(2.8367463594668,40.8349226258683,0.));
#28274=CARTESIAN_POINT('Ctrl Pts',(2.8367463594668,40.8349226258683,18.));
#28275=CARTESIAN_POINT('Ctrl Pts',(2.80342531768405,40.9288696352159,0.));
#28276=CARTESIAN_POINT('Ctrl Pts',(2.80342531768405,40.9288696352159,18.));
#28277=CARTESIAN_POINT('Ctrl Pts',(2.76949151194864,41.0227421242398,0.));
#28278=CARTESIAN_POINT('Ctrl Pts',(2.76949151194864,41.0227421242398,18.));
#28279=CARTESIAN_POINT('Ctrl Pts',(2.73494956725006,41.1165384061145,0.));
#28280=CARTESIAN_POINT('Ctrl Pts',(2.73494956725006,41.1165384061145,18.));
#28281=CARTESIAN_POINT('Ctrl Pts',(2.69980383625016,41.2102568187956,0.));
#28282=CARTESIAN_POINT('Ctrl Pts',(2.69980383625016,41.2102568187956,18.));
#28283=CARTESIAN_POINT('Ctrl Pts',(2.66405934050118,41.3038957096306,0.));
#28284=CARTESIAN_POINT('Ctrl Pts',(2.66405934050118,41.3038957096306,18.));
#28285=CARTESIAN_POINT('Ctrl Pts',(2.62772200460657,41.3974534325937,0.));
#28286=CARTESIAN_POINT('Ctrl Pts',(2.62772200460657,41.3974534325937,18.));
#28287=CARTESIAN_POINT('Ctrl Pts',(2.59079818040172,41.4909283577703,0.));
#28288=CARTESIAN_POINT('Ctrl Pts',(2.59079818040172,41.4909283577703,18.));
#28289=CARTESIAN_POINT('Ctrl Pts',(2.55329436064184,41.5843188786284,0.));
#28290=CARTESIAN_POINT('Ctrl Pts',(2.55329436064184,41.5843188786284,18.));
#28291=CARTESIAN_POINT('Ctrl Pts',(2.51521684674477,41.6776234194583,0.));
#28292=CARTESIAN_POINT('Ctrl Pts',(2.51521684674477,41.6776234194583,18.));
#28293=CARTESIAN_POINT('Ctrl Pts',(2.47657137427693,41.7708404467533,0.));
#28294=CARTESIAN_POINT('Ctrl Pts',(2.47657137427693,41.7708404467533,18.));
#28295=CARTESIAN_POINT('Ctrl Pts',(2.43736301434201,41.8639684667923,0.));
#28296=CARTESIAN_POINT('Ctrl Pts',(2.43736301434201,41.8639684667923,18.));
#28297=CARTESIAN_POINT('Ctrl Pts',(2.39759639399648,41.9570060084039,0.));
#28298=CARTESIAN_POINT('Ctrl Pts',(2.39759639399648,41.9570060084039,18.));
#28299=CARTESIAN_POINT('Ctrl Pts',(2.35727584066429,42.0499516093661,0.));
#28300=CARTESIAN_POINT('Ctrl Pts',(2.35727584066429,42.0499516093661,18.));
#28301=CARTESIAN_POINT('Ctrl Pts',(2.3164055474281,42.1428038039937,0.));
#28302=CARTESIAN_POINT('Ctrl Pts',(2.3164055474281,42.1428038039937,18.));
#28303=CARTESIAN_POINT('Ctrl Pts',(2.27498976664775,42.2355611060784,0.));
#28304=CARTESIAN_POINT('Ctrl Pts',(2.27498976664775,42.2355611060784,18.));
#28305=CARTESIAN_POINT('Ctrl Pts',(2.233032874655,42.3282220118033,0.));
#28306=CARTESIAN_POINT('Ctrl Pts',(2.233032874655,42.3282220118033,18.));
#28307=CARTESIAN_POINT('Ctrl Pts',(2.19053924976738,42.4207850290047,0.));
#28308=CARTESIAN_POINT('Ctrl Pts',(2.19053924976738,42.4207850290047,18.));
#28309=CARTESIAN_POINT('Ctrl Pts',(2.14751319676746,42.5132487024335,0.));
#28310=CARTESIAN_POINT('Ctrl Pts',(2.14751319676746,42.5132487024335,18.));
#28311=CARTESIAN_POINT('Ctrl Pts',(2.10395886401771,42.6056116373456,0.));
#28312=CARTESIAN_POINT('Ctrl Pts',(2.10395886401771,42.6056116373456,18.));
#28313=CARTESIAN_POINT('Ctrl Pts',(2.05988014924519,42.6978725343209,0.));
#28314=CARTESIAN_POINT('Ctrl Pts',(2.05988014924519,42.6978725343209,18.));
#28315=CARTESIAN_POINT('Ctrl Pts',(2.01528067528089,42.7900301875309,0.));
#28316=CARTESIAN_POINT('Ctrl Pts',(2.01528067528089,42.7900301875309,18.));
#28317=CARTESIAN_POINT('Ctrl Pts',(1.97016390194216,42.8820834139973,0.));
#28318=CARTESIAN_POINT('Ctrl Pts',(1.97016390194216,42.8820834139973,18.));
#28319=CARTESIAN_POINT('Ctrl Pts',(1.92453321512436,42.9740309956624,0.));
#28320=CARTESIAN_POINT('Ctrl Pts',(1.92453321512436,42.9740309956624,18.));
#28321=CARTESIAN_POINT('Ctrl Pts',(1.87839202014609,43.065871623255,0.));
#28322=CARTESIAN_POINT('Ctrl Pts',(1.87839202014609,43.065871623255,18.));
#28323=CARTESIAN_POINT('Ctrl Pts',(1.83174385734712,43.1576038253643,0.));
#28324=CARTESIAN_POINT('Ctrl Pts',(1.83174385734712,43.1576038253643,18.));
#28325=CARTESIAN_POINT('Ctrl Pts',(1.7845924484277,43.2492259505872,0.));
#28326=CARTESIAN_POINT('Ctrl Pts',(1.7845924484277,43.2492259505872,18.));
#28327=CARTESIAN_POINT('Ctrl Pts',(1.73694151741124,43.3407363140236,0.));
#28328=CARTESIAN_POINT('Ctrl Pts',(1.73694151741124,43.3407363140236,18.));
#28329=CARTESIAN_POINT('Ctrl Pts',(1.68879465270608,43.4321333178711,0.));
#28330=CARTESIAN_POINT('Ctrl Pts',(1.68879465270608,43.4321333178711,18.));
#28331=CARTESIAN_POINT('Ctrl Pts',(1.64015515906649,43.5234155788248,0.));
#28332=CARTESIAN_POINT('Ctrl Pts',(1.64015515906649,43.5234155788248,18.));
#28333=CARTESIAN_POINT('Ctrl Pts',(1.59102591108104,43.6145820637333,0.));
#28334=CARTESIAN_POINT('Ctrl Pts',(1.59102591108104,43.6145820637333,18.));
#28335=CARTESIAN_POINT('Ctrl Pts',(1.54140922714765,43.7056321934163,0.));
#28336=CARTESIAN_POINT('Ctrl Pts',(1.54140922714765,43.7056321934163,18.));
#28337=CARTESIAN_POINT('Ctrl Pts',(1.49130689006067,43.7965657112708,0.));
#28338=CARTESIAN_POINT('Ctrl Pts',(1.49130689006067,43.7965657112708,18.));
#28339=CARTESIAN_POINT('Ctrl Pts',(1.45083750111682,43.8692192047561,0.));
#28340=CARTESIAN_POINT('Ctrl Pts',(1.45083750111682,43.8692192047561,18.));
#28341=CARTESIAN_POINT('Ctrl Pts',(1.42026781296157,43.9236568607623,0.));
#28342=CARTESIAN_POINT('Ctrl Pts',(1.42026781296157,43.9236568607623,18.));
#28343=CARTESIAN_POINT('Ctrl Pts',(1.39979132121931,43.9599253218251,0.));
#28344=CARTESIAN_POINT('Ctrl Pts',(1.39979132121931,43.9599253218251,18.));
#28345=CARTESIAN_POINT('Ctrl Pts',(1.38952890043916,43.9780537249529,0.));
#28346=CARTESIAN_POINT('Ctrl Pts',(1.38952890043916,43.9780537249529,18.));
#28347=CARTESIAN_POINT('Ctrl Pts',(3.50724370857673,37.4237196983923,0.));
#28348=CARTESIAN_POINT('Ctrl Pts',(3.50901346997657,37.4426037737699,0.));
#28349=CARTESIAN_POINT('Ctrl Pts',(3.51204731876361,37.4803889700239,0.));
#28350=CARTESIAN_POINT('Ctrl Pts',(3.5150810906521,37.5371179004295,0.));
#28351=CARTESIAN_POINT('Ctrl Pts',(3.51624243734645,37.6128545966533,0.));
#28352=CARTESIAN_POINT('Ctrl Pts',(3.51375922979958,37.7076643105286,0.));
#28353=CARTESIAN_POINT('Ctrl Pts',(3.50844720825128,37.8025803811856,0.));
#28354=CARTESIAN_POINT('Ctrl Pts',(3.50139628556084,37.8975688353863,0.));
#28355=CARTESIAN_POINT('Ctrl Pts',(3.49340804454646,37.9926009950482,0.));
#28356=CARTESIAN_POINT('Ctrl Pts',(3.48478279878234,38.0876589224537,0.));
#28357=CARTESIAN_POINT('Ctrl Pts',(3.47549027265412,38.1827321816559,0.));
#28358=CARTESIAN_POINT('Ctrl Pts',(3.46530185256873,38.2778154909527,0.));
#28359=CARTESIAN_POINT('Ctrl Pts',(3.45393053211023,38.3729061502716,0.));
#28360=CARTESIAN_POINT('Ctrl Pts',(3.44118343200303,38.4680013094732,0.));
#28361=CARTESIAN_POINT('Ctrl Pts',(3.42705871084997,38.5630961226878,0.));
#28362=CARTESIAN_POINT('Ctrl Pts',(3.41166717511901,38.6581847668347,0.));
#28363=CARTESIAN_POINT('Ctrl Pts',(3.39518333281818,38.7532609709905,0.));
#28364=CARTESIAN_POINT('Ctrl Pts',(3.37778863054482,38.8483186930884,0.));
#28365=CARTESIAN_POINT('Ctrl Pts',(3.35960922799481,38.9433528420174,0.));
#28366=CARTESIAN_POINT('Ctrl Pts',(3.34068601264472,39.0383596151636,0.));
#28367=CARTESIAN_POINT('Ctrl Pts',(3.32100933979558,39.1333360409949,0.));
#28368=CARTESIAN_POINT('Ctrl Pts',(3.30054018081688,39.2282796893977,0.));
#28369=CARTESIAN_POINT('Ctrl Pts',(3.27923485388118,39.3231883392913,0.));
#28370=CARTESIAN_POINT('Ctrl Pts',(3.25707264313388,39.4180596080755,0.));
#28371=CARTESIAN_POINT('Ctrl Pts',(3.23406609691661,39.5128908052622,0.));
#28372=CARTESIAN_POINT('Ctrl Pts',(3.21024640045595,39.607679107639,0.));
#28373=CARTESIAN_POINT('Ctrl Pts',(3.18565465503836,39.7024216585552,0.));
#28374=CARTESIAN_POINT('Ctrl Pts',(3.16033160752804,39.7971156880138,0.));
#28375=CARTESIAN_POINT('Ctrl Pts',(3.13430604330356,39.8917586491576,0.));
#28376=CARTESIAN_POINT('Ctrl Pts',(3.10759149802908,39.9863482523153,0.));
#28377=CARTESIAN_POINT('Ctrl Pts',(3.08019251155016,40.0808823811787,0.));
#28378=CARTESIAN_POINT('Ctrl Pts',(3.05210847423071,40.1753590391515,0.));
#28379=CARTESIAN_POINT('Ctrl Pts',(3.02333808901595,40.2697762886113,0.));
#28380=CARTESIAN_POINT('Ctrl Pts',(2.9938844645822,40.3641321823444,0.));
#28381=CARTESIAN_POINT('Ctrl Pts',(2.96375636417323,40.4584247445196,0.));
#28382=CARTESIAN_POINT('Ctrl Pts',(2.93296560822894,40.5526520010651,0.));
#28383=CARTESIAN_POINT('Ctrl Pts',(2.90152548734343,40.6468119976928,0.));
#28384=CARTESIAN_POINT('Ctrl Pts',(2.86944892209898,40.7409028213129,0.));
#28385=CARTESIAN_POINT('Ctrl Pts',(2.8367463594668,40.8349226258683,0.));
#28386=CARTESIAN_POINT('Ctrl Pts',(2.80342531768405,40.9288696352159,0.));
#28387=CARTESIAN_POINT('Ctrl Pts',(2.76949151194864,41.0227421242398,0.));
#28388=CARTESIAN_POINT('Ctrl Pts',(2.73494956725006,41.1165384061145,0.));
#28389=CARTESIAN_POINT('Ctrl Pts',(2.69980383625016,41.2102568187956,0.));
#28390=CARTESIAN_POINT('Ctrl Pts',(2.66405934050118,41.3038957096306,0.));
#28391=CARTESIAN_POINT('Ctrl Pts',(2.62772200460657,41.3974534325937,0.));
#28392=CARTESIAN_POINT('Ctrl Pts',(2.59079818040172,41.4909283577703,0.));
#28393=CARTESIAN_POINT('Ctrl Pts',(2.55329436064184,41.5843188786284,0.));
#28394=CARTESIAN_POINT('Ctrl Pts',(2.51521684674477,41.6776234194583,0.));
#28395=CARTESIAN_POINT('Ctrl Pts',(2.47657137427693,41.7708404467533,0.));
#28396=CARTESIAN_POINT('Ctrl Pts',(2.43736301434201,41.8639684667923,0.));
#28397=CARTESIAN_POINT('Ctrl Pts',(2.39759639399648,41.9570060084039,0.));
#28398=CARTESIAN_POINT('Ctrl Pts',(2.35727584066429,42.0499516093661,0.));
#28399=CARTESIAN_POINT('Ctrl Pts',(2.3164055474281,42.1428038039937,0.));
#28400=CARTESIAN_POINT('Ctrl Pts',(2.27498976664775,42.2355611060784,0.));
#28401=CARTESIAN_POINT('Ctrl Pts',(2.233032874655,42.3282220118033,0.));
#28402=CARTESIAN_POINT('Ctrl Pts',(2.19053924976738,42.4207850290047,0.));
#28403=CARTESIAN_POINT('Ctrl Pts',(2.14751319676746,42.5132487024335,0.));
#28404=CARTESIAN_POINT('Ctrl Pts',(2.10395886401771,42.6056116373456,0.));
#28405=CARTESIAN_POINT('Ctrl Pts',(2.05988014924519,42.6978725343209,0.));
#28406=CARTESIAN_POINT('Ctrl Pts',(2.01528067528089,42.7900301875309,0.));
#28407=CARTESIAN_POINT('Ctrl Pts',(1.97016390194216,42.8820834139973,0.));
#28408=CARTESIAN_POINT('Ctrl Pts',(1.92453321512436,42.9740309956624,0.));
#28409=CARTESIAN_POINT('Ctrl Pts',(1.87839202014609,43.065871623255,0.));
#28410=CARTESIAN_POINT('Ctrl Pts',(1.83174385734712,43.1576038253643,0.));
#28411=CARTESIAN_POINT('Ctrl Pts',(1.7845924484277,43.2492259505872,0.));
#28412=CARTESIAN_POINT('Ctrl Pts',(1.73694151741124,43.3407363140236,0.));
#28413=CARTESIAN_POINT('Ctrl Pts',(1.68879465270608,43.4321333178711,0.));
#28414=CARTESIAN_POINT('Ctrl Pts',(1.64015515906649,43.5234155788248,0.));
#28415=CARTESIAN_POINT('Ctrl Pts',(1.59102591108104,43.6145820637333,0.));
#28416=CARTESIAN_POINT('Ctrl Pts',(1.53148589036097,43.7238422193529,0.));
#28417=CARTESIAN_POINT('Ctrl Pts',(1.48126213998559,43.8147465842503,0.));
#28418=CARTESIAN_POINT('Ctrl Pts',(1.44069595482723,43.8873767449247,0.));
#28419=CARTESIAN_POINT('Ctrl Pts',(1.41005374202874,43.9417969186811,0.));
#28420=CARTESIAN_POINT('Ctrl Pts',(1.38952890043916,43.9780537249529,0.));
#28421=CARTESIAN_POINT('Ctrl Pts',(3.50724370857673,37.4237196983923,15.));
#28422=CARTESIAN_POINT('Ctrl Pts',(3.50901346997657,37.4426037737699,15.));
#28423=CARTESIAN_POINT('Ctrl Pts',(3.51204731876361,37.4803889700239,15.));
#28424=CARTESIAN_POINT('Ctrl Pts',(3.5150810906521,37.5371179004295,15.));
#28425=CARTESIAN_POINT('Ctrl Pts',(3.51624243734645,37.6128545966533,15.));
#28426=CARTESIAN_POINT('Ctrl Pts',(3.51375922979958,37.7076643105286,15.));
#28427=CARTESIAN_POINT('Ctrl Pts',(3.50844720825128,37.8025803811856,15.));
#28428=CARTESIAN_POINT('Ctrl Pts',(3.50139628556084,37.8975688353863,15.));
#28429=CARTESIAN_POINT('Ctrl Pts',(3.49340804454646,37.9926009950482,15.));
#28430=CARTESIAN_POINT('Ctrl Pts',(3.48478279878234,38.0876589224537,15.));
#28431=CARTESIAN_POINT('Ctrl Pts',(3.47549027265412,38.1827321816559,15.));
#28432=CARTESIAN_POINT('Ctrl Pts',(3.46530185256873,38.2778154909527,15.));
#28433=CARTESIAN_POINT('Ctrl Pts',(3.45393053211023,38.3729061502716,15.));
#28434=CARTESIAN_POINT('Ctrl Pts',(3.44118343200303,38.4680013094732,15.));
#28435=CARTESIAN_POINT('Ctrl Pts',(3.42705871084997,38.5630961226878,15.));
#28436=CARTESIAN_POINT('Ctrl Pts',(3.41166717511901,38.6581847668347,15.));
#28437=CARTESIAN_POINT('Ctrl Pts',(3.39518333281818,38.7532609709905,15.));
#28438=CARTESIAN_POINT('Ctrl Pts',(3.37778863054482,38.8483186930884,15.));
#28439=CARTESIAN_POINT('Ctrl Pts',(3.35960922799481,38.9433528420174,15.));
#28440=CARTESIAN_POINT('Ctrl Pts',(3.34068601264472,39.0383596151636,15.));
#28441=CARTESIAN_POINT('Ctrl Pts',(3.32100933979558,39.1333360409949,15.));
#28442=CARTESIAN_POINT('Ctrl Pts',(3.30054018081688,39.2282796893977,15.));
#28443=CARTESIAN_POINT('Ctrl Pts',(3.27923485388118,39.3231883392913,15.));
#28444=CARTESIAN_POINT('Ctrl Pts',(3.25707264313388,39.4180596080755,15.));
#28445=CARTESIAN_POINT('Ctrl Pts',(3.23406609691661,39.5128908052622,15.));
#28446=CARTESIAN_POINT('Ctrl Pts',(3.21024640045595,39.607679107639,15.));
#28447=CARTESIAN_POINT('Ctrl Pts',(3.18565465503836,39.7024216585552,15.));
#28448=CARTESIAN_POINT('Ctrl Pts',(3.16033160752804,39.7971156880138,15.));
#28449=CARTESIAN_POINT('Ctrl Pts',(3.13430604330356,39.8917586491576,15.));
#28450=CARTESIAN_POINT('Ctrl Pts',(3.10759149802908,39.9863482523153,15.));
#28451=CARTESIAN_POINT('Ctrl Pts',(3.08019251155016,40.0808823811787,15.));
#28452=CARTESIAN_POINT('Ctrl Pts',(3.05210847423071,40.1753590391515,15.));
#28453=CARTESIAN_POINT('Ctrl Pts',(3.02333808901595,40.2697762886113,15.));
#28454=CARTESIAN_POINT('Ctrl Pts',(2.9938844645822,40.3641321823444,15.));
#28455=CARTESIAN_POINT('Ctrl Pts',(2.96375636417323,40.4584247445196,15.));
#28456=CARTESIAN_POINT('Ctrl Pts',(2.93296560822894,40.5526520010651,15.));
#28457=CARTESIAN_POINT('Ctrl Pts',(2.90152548734343,40.6468119976928,15.));
#28458=CARTESIAN_POINT('Ctrl Pts',(2.86944892209898,40.7409028213129,15.));
#28459=CARTESIAN_POINT('Ctrl Pts',(2.8367463594668,40.8349226258683,15.));
#28460=CARTESIAN_POINT('Ctrl Pts',(2.80342531768405,40.9288696352159,15.));
#28461=CARTESIAN_POINT('Ctrl Pts',(2.76949151194864,41.0227421242398,15.));
#28462=CARTESIAN_POINT('Ctrl Pts',(2.73494956725006,41.1165384061145,15.));
#28463=CARTESIAN_POINT('Ctrl Pts',(2.69980383625016,41.2102568187956,15.));
#28464=CARTESIAN_POINT('Ctrl Pts',(2.66405934050118,41.3038957096306,15.));
#28465=CARTESIAN_POINT('Ctrl Pts',(2.62772200460657,41.3974534325937,15.));
#28466=CARTESIAN_POINT('Ctrl Pts',(2.59079818040172,41.4909283577703,15.));
#28467=CARTESIAN_POINT('Ctrl Pts',(2.55329436064184,41.5843188786284,15.));
#28468=CARTESIAN_POINT('Ctrl Pts',(2.51521684674477,41.6776234194583,15.));
#28469=CARTESIAN_POINT('Ctrl Pts',(2.47657137427693,41.7708404467533,15.));
#28470=CARTESIAN_POINT('Ctrl Pts',(2.43736301434201,41.8639684667923,15.));
#28471=CARTESIAN_POINT('Ctrl Pts',(2.39759639399648,41.9570060084039,15.));
#28472=CARTESIAN_POINT('Ctrl Pts',(2.35727584066429,42.0499516093661,15.));
#28473=CARTESIAN_POINT('Ctrl Pts',(2.3164055474281,42.1428038039937,15.));
#28474=CARTESIAN_POINT('Ctrl Pts',(2.27498976664775,42.2355611060784,15.));
#28475=CARTESIAN_POINT('Ctrl Pts',(2.233032874655,42.3282220118033,15.));
#28476=CARTESIAN_POINT('Ctrl Pts',(2.19053924976738,42.4207850290047,15.));
#28477=CARTESIAN_POINT('Ctrl Pts',(2.14751319676746,42.5132487024335,15.));
#28478=CARTESIAN_POINT('Ctrl Pts',(2.10395886401771,42.6056116373456,15.));
#28479=CARTESIAN_POINT('Ctrl Pts',(2.05988014924519,42.6978725343209,15.));
#28480=CARTESIAN_POINT('Ctrl Pts',(2.01528067528089,42.7900301875309,15.));
#28481=CARTESIAN_POINT('Ctrl Pts',(1.97016390194216,42.8820834139973,15.));
#28482=CARTESIAN_POINT('Ctrl Pts',(1.92453321512436,42.9740309956624,15.));
#28483=CARTESIAN_POINT('Ctrl Pts',(1.87839202014609,43.065871623255,15.));
#28484=CARTESIAN_POINT('Ctrl Pts',(1.83174385734712,43.1576038253643,15.));
#28485=CARTESIAN_POINT('Ctrl Pts',(1.7845924484277,43.2492259505872,15.));
#28486=CARTESIAN_POINT('Ctrl Pts',(1.73694151741124,43.3407363140236,15.));
#28487=CARTESIAN_POINT('Ctrl Pts',(1.68879465270608,43.4321333178711,15.));
#28488=CARTESIAN_POINT('Ctrl Pts',(1.64015515906649,43.5234155788248,15.));
#28489=CARTESIAN_POINT('Ctrl Pts',(1.59102591108104,43.6145820637333,15.));
#28490=CARTESIAN_POINT('Ctrl Pts',(1.53148589036097,43.7238422193529,15.));
#28491=CARTESIAN_POINT('Ctrl Pts',(1.48126213998559,43.8147465842503,15.));
#28492=CARTESIAN_POINT('Ctrl Pts',(1.44069595482723,43.8873767449247,15.));
#28493=CARTESIAN_POINT('Ctrl Pts',(1.41005374202874,43.9417969186811,15.));
#28494=CARTESIAN_POINT('Ctrl Pts',(1.38952890043916,43.9780537249529,15.));
#28495=CARTESIAN_POINT('Ctrl Pts',(12.2684454652018,42.2550026135057,0.));
#28496=CARTESIAN_POINT('Ctrl Pts',(12.2684454652018,42.2550026135057,18.));
#28497=CARTESIAN_POINT('Ctrl Pts',(12.2530833383985,42.2409327400055,0.));
#28498=CARTESIAN_POINT('Ctrl Pts',(12.2530833383985,42.2409327400055,18.));
#28499=CARTESIAN_POINT('Ctrl Pts',(12.222401466668,42.2127669677092,0.));
#28500=CARTESIAN_POINT('Ctrl Pts',(12.222401466668,42.2127669677092,18.));
#28501=CARTESIAN_POINT('Ctrl Pts',(12.1765058047069,42.1704402333854,0.));
#28502=CARTESIAN_POINT('Ctrl Pts',(12.1765058047069,42.1704402333854,18.));
#28503=CARTESIAN_POINT('Ctrl Pts',(12.1155659644537,42.1138483839101,0.));
#28504=CARTESIAN_POINT('Ctrl Pts',(12.1155659644537,42.1138483839101,18.));
#28505=CARTESIAN_POINT('Ctrl Pts',(12.0398158079102,42.0428479428228,0.));
#28506=CARTESIAN_POINT('Ctrl Pts',(12.0398158079102,42.0428479428228,18.));
#28507=CARTESIAN_POINT('Ctrl Pts',(11.9644914999263,41.9715865222182,0.));
#28508=CARTESIAN_POINT('Ctrl Pts',(11.9644914999263,41.9715865222182,18.));
#28509=CARTESIAN_POINT('Ctrl Pts',(11.8895948153349,41.9000638152266,0.));
#28510=CARTESIAN_POINT('Ctrl Pts',(11.8895948153349,41.9000638152266,18.));
#28511=CARTESIAN_POINT('Ctrl Pts',(11.81512813804,41.8282796562569,0.));
#28512=CARTESIAN_POINT('Ctrl Pts',(11.81512813804,41.8282796562569,18.));
#28513=CARTESIAN_POINT('Ctrl Pts',(11.7410945211992,41.7562341395977,0.));
#28514=CARTESIAN_POINT('Ctrl Pts',(11.7410945211992,41.7562341395977,18.));
#28515=CARTESIAN_POINT('Ctrl Pts',(11.6674975352852,41.6839275596248,0.));
#28516=CARTESIAN_POINT('Ctrl Pts',(11.6674975352852,41.6839275596248,18.));
#28517=CARTESIAN_POINT('Ctrl Pts',(11.5943410868252,41.6113603270596,0.));
#28518=CARTESIAN_POINT('Ctrl Pts',(11.5943410868252,41.6113603270596,18.));
#28519=CARTESIAN_POINT('Ctrl Pts',(11.5216292382388,41.5385328935506,0.));
#28520=CARTESIAN_POINT('Ctrl Pts',(11.5216292382388,41.5385328935506,18.));
#28521=CARTESIAN_POINT('Ctrl Pts',(11.4493660393849,41.4654456796071,0.));
#28522=CARTESIAN_POINT('Ctrl Pts',(11.4493660393849,41.4654456796071,18.));
#28523=CARTESIAN_POINT('Ctrl Pts',(11.3775553120176,41.3920989905986,0.));
#28524=CARTESIAN_POINT('Ctrl Pts',(11.3775553120176,41.3920989905986,18.));
#28525=CARTESIAN_POINT('Ctrl Pts',(11.3062006993745,41.3184930194148,0.));
#28526=CARTESIAN_POINT('Ctrl Pts',(11.3062006993745,41.3184930194148,18.));
#28527=CARTESIAN_POINT('Ctrl Pts',(11.2353057980338,41.2446278781981,0.));
#28528=CARTESIAN_POINT('Ctrl Pts',(11.2353057980338,41.2446278781981,18.));
#28529=CARTESIAN_POINT('Ctrl Pts',(11.1648742640378,41.1705036228854,0.));
#28530=CARTESIAN_POINT('Ctrl Pts',(11.1648742640378,41.1705036228854,18.));
#28531=CARTESIAN_POINT('Ctrl Pts',(11.0949099155251,41.0961202807715,0.));
#28532=CARTESIAN_POINT('Ctrl Pts',(11.0949099155251,41.0961202807715,18.));
#28533=CARTESIAN_POINT('Ctrl Pts',(11.0254168609972,41.0214778832142,0.));
#28534=CARTESIAN_POINT('Ctrl Pts',(11.0254168609972,41.0214778832142,18.));
#28535=CARTESIAN_POINT('Ctrl Pts',(10.956399476781,40.9465764747798,0.));
#28536=CARTESIAN_POINT('Ctrl Pts',(10.956399476781,40.9465764747798,18.));
#28537=CARTESIAN_POINT('Ctrl Pts',(10.8878623066646,40.8714161092412,0.));
#28538=CARTESIAN_POINT('Ctrl Pts',(10.8878623066646,40.8714161092412,18.));
#28539=CARTESIAN_POINT('Ctrl Pts',(10.8198099757795,40.7959968527561,0.));
#28540=CARTESIAN_POINT('Ctrl Pts',(10.8198099757795,40.7959968527561,18.));
#28541=CARTESIAN_POINT('Ctrl Pts',(10.7522471109694,40.7203187831783,0.));
#28542=CARTESIAN_POINT('Ctrl Pts',(10.7522471109694,40.7203187831783,18.));
#28543=CARTESIAN_POINT('Ctrl Pts',(10.6851782157325,40.6443819999244,0.));
#28544=CARTESIAN_POINT('Ctrl Pts',(10.6851782157325,40.6443819999244,18.));
#28545=CARTESIAN_POINT('Ctrl Pts',(10.618607730849,40.5681866012103,0.));
#28546=CARTESIAN_POINT('Ctrl Pts',(10.618607730849,40.5681866012103,18.));
#28547=CARTESIAN_POINT('Ctrl Pts',(10.5525402237951,40.4917326404439,0.));
#28548=CARTESIAN_POINT('Ctrl Pts',(10.5525402237951,40.4917326404439,18.));
#28549=CARTESIAN_POINT('Ctrl Pts',(10.48698054978,40.4150200869536,0.));
#28550=CARTESIAN_POINT('Ctrl Pts',(10.48698054978,40.4150200869536,18.));
#28551=CARTESIAN_POINT('Ctrl Pts',(10.4219339932951,40.3380487942952,0.));
#28552=CARTESIAN_POINT('Ctrl Pts',(10.4219339932951,40.3380487942952,18.));
#28553=CARTESIAN_POINT('Ctrl Pts',(10.3574064830678,40.2608184485326,0.));
#28554=CARTESIAN_POINT('Ctrl Pts',(10.3574064830678,40.2608184485326,18.));
#28555=CARTESIAN_POINT('Ctrl Pts',(10.2934044990237,40.1833286010098,0.));
#28556=CARTESIAN_POINT('Ctrl Pts',(10.2934044990237,40.1833286010098,18.));
#28557=CARTESIAN_POINT('Ctrl Pts',(10.2299347125857,40.1055787732578,0.));
#28558=CARTESIAN_POINT('Ctrl Pts',(10.2299347125857,40.1055787732578,18.));
#28559=CARTESIAN_POINT('Ctrl Pts',(10.1670036683795,40.0275685525923,0.));
#28560=CARTESIAN_POINT('Ctrl Pts',(10.1670036683795,40.0275685525923,18.));
#28561=CARTESIAN_POINT('Ctrl Pts',(10.1046175096878,39.9492976736738,0.));
#28562=CARTESIAN_POINT('Ctrl Pts',(10.1046175096878,39.9492976736738,18.));
#28563=CARTESIAN_POINT('Ctrl Pts',(10.0427815229883,39.8707661565233,0.));
#28564=CARTESIAN_POINT('Ctrl Pts',(10.0427815229883,39.8707661565233,18.));
#28565=CARTESIAN_POINT('Ctrl Pts',(9.98150036150824,39.7919742367922,0.));
#28566=CARTESIAN_POINT('Ctrl Pts',(9.98150036150824,39.7919742367922,18.));
#28567=CARTESIAN_POINT('Ctrl Pts',(9.92077894513192,39.712922089547,0.));
#28568=CARTESIAN_POINT('Ctrl Pts',(9.92077894513192,39.712922089547,18.));
#28569=CARTESIAN_POINT('Ctrl Pts',(9.8606232424256,39.6336095893767,0.));
#28570=CARTESIAN_POINT('Ctrl Pts',(9.8606232424256,39.6336095893767,18.));
#28571=CARTESIAN_POINT('Ctrl Pts',(9.80104095251614,39.5540361022309,0.));
#28572=CARTESIAN_POINT('Ctrl Pts',(9.80104095251614,39.5540361022309,18.));
#28573=CARTESIAN_POINT('Ctrl Pts',(9.74204258152664,39.4742001555227,0.));
#28574=CARTESIAN_POINT('Ctrl Pts',(9.74204258152664,39.4742001555227,18.));
#28575=CARTESIAN_POINT('Ctrl Pts',(9.68364100883828,39.3940995760289,0.));
#28576=CARTESIAN_POINT('Ctrl Pts',(9.68364100883828,39.3940995760289,18.));
#28577=CARTESIAN_POINT('Ctrl Pts',(9.62584947846544,39.3137321153686,0.));
#28578=CARTESIAN_POINT('Ctrl Pts',(9.62584947846544,39.3137321153686,18.));
#28579=CARTESIAN_POINT('Ctrl Pts',(9.56867984233624,39.2330959982788,0.));
#28580=CARTESIAN_POINT('Ctrl Pts',(9.56867984233624,39.2330959982788,18.));
#28581=CARTESIAN_POINT('Ctrl Pts',(9.51214104535621,39.1521903958956,0.));
#28582=CARTESIAN_POINT('Ctrl Pts',(9.51214104535621,39.1521903958956,18.));
#28583=CARTESIAN_POINT('Ctrl Pts',(9.45623664577432,39.0710161994951,0.));
#28584=CARTESIAN_POINT('Ctrl Pts',(9.45623664577432,39.0710161994951,18.));
#28585=CARTESIAN_POINT('Ctrl Pts',(9.40096600877644,38.9895756526779,0.));
#28586=CARTESIAN_POINT('Ctrl Pts',(9.40096600877644,38.9895756526779,18.));
#28587=CARTESIAN_POINT('Ctrl Pts',(9.34632917154637,38.9078708427078,0.));
#28588=CARTESIAN_POINT('Ctrl Pts',(9.34632917154637,38.9078708427078,18.));
#28589=CARTESIAN_POINT('Ctrl Pts',(9.29233110570903,38.8259023794241,0.));
#28590=CARTESIAN_POINT('Ctrl Pts',(9.29233110570903,38.8259023794241,18.));
#28591=CARTESIAN_POINT('Ctrl Pts',(9.23898539199332,38.7436682576832,0.));
#28592=CARTESIAN_POINT('Ctrl Pts',(9.23898539199332,38.7436682576832,18.));
#28593=CARTESIAN_POINT('Ctrl Pts',(9.1863201939433,38.6611620045193,0.));
#28594=CARTESIAN_POINT('Ctrl Pts',(9.1863201939433,38.6611620045193,18.));
#28595=CARTESIAN_POINT('Ctrl Pts',(9.13437512010586,38.5783736628826,0.));
#28596=CARTESIAN_POINT('Ctrl Pts',(9.13437512010586,38.5783736628826,18.));
#28597=CARTESIAN_POINT('Ctrl Pts',(9.08319014288086,38.4952932486131,0.));
#28598=CARTESIAN_POINT('Ctrl Pts',(9.08319014288086,38.4952932486131,18.));
#28599=CARTESIAN_POINT('Ctrl Pts',(9.03279579360191,38.4119138099805,0.));
#28600=CARTESIAN_POINT('Ctrl Pts',(9.03279579360191,38.4119138099805,18.));
#28601=CARTESIAN_POINT('Ctrl Pts',(8.9832048378576,38.3282340281403,0.));
#28602=CARTESIAN_POINT('Ctrl Pts',(8.9832048378576,38.3282340281403,18.));
#28603=CARTESIAN_POINT('Ctrl Pts',(8.93439830996339,38.2442625706309,0.));
#28604=CARTESIAN_POINT('Ctrl Pts',(8.93439830996339,38.2442625706309,18.));
#28605=CARTESIAN_POINT('Ctrl Pts',(8.88633535238435,38.1600150482528,0.));
#28606=CARTESIAN_POINT('Ctrl Pts',(8.88633535238435,38.1600150482528,18.));
#28607=CARTESIAN_POINT('Ctrl Pts',(8.8389795976335,38.0755058326913,0.));
#28608=CARTESIAN_POINT('Ctrl Pts',(8.8389795976335,38.0755058326913,18.));
#28609=CARTESIAN_POINT('Ctrl Pts',(8.79232279131092,37.9907407304174,0.));
#28610=CARTESIAN_POINT('Ctrl Pts',(8.79232279131092,37.9907407304174,18.));
#28611=CARTESIAN_POINT('Ctrl Pts',(8.74640499479003,37.9057107230066,0.));
#28612=CARTESIAN_POINT('Ctrl Pts',(8.74640499479003,37.9057107230066,18.));
#28613=CARTESIAN_POINT('Ctrl Pts',(8.70134776631144,37.8203816669032,0.));
#28614=CARTESIAN_POINT('Ctrl Pts',(8.70134776631144,37.8203816669032,18.));
#28615=CARTESIAN_POINT('Ctrl Pts',(8.65732553894525,37.7347032383719,0.));
#28616=CARTESIAN_POINT('Ctrl Pts',(8.65732553894525,37.7347032383719,18.));
#28617=CARTESIAN_POINT('Ctrl Pts',(8.61450621749155,37.6486274754754,0.));
#28618=CARTESIAN_POINT('Ctrl Pts',(8.61450621749155,37.6486274754754,18.));
#28619=CARTESIAN_POINT('Ctrl Pts',(8.57299698459466,37.5621256752108,0.));
#28620=CARTESIAN_POINT('Ctrl Pts',(8.57299698459466,37.5621256752108,18.));
#28621=CARTESIAN_POINT('Ctrl Pts',(8.53279758643785,37.4752030152968,0.));
#28622=CARTESIAN_POINT('Ctrl Pts',(8.53279758643785,37.4752030152968,18.));
#28623=CARTESIAN_POINT('Ctrl Pts',(8.49372546467076,37.3879218093514,0.));
#28624=CARTESIAN_POINT('Ctrl Pts',(8.49372546467076,37.3879218093514,18.));
#28625=CARTESIAN_POINT('Ctrl Pts',(8.4555084943396,37.3003733151561,0.));
#28626=CARTESIAN_POINT('Ctrl Pts',(8.4555084943396,37.3003733151561,18.));
#28627=CARTESIAN_POINT('Ctrl Pts',(8.41793088313261,37.2126332013933,0.));
#28628=CARTESIAN_POINT('Ctrl Pts',(8.41793088313261,37.2126332013933,18.));
#28629=CARTESIAN_POINT('Ctrl Pts',(8.38096706211448,37.1247207489179,0.));
#28630=CARTESIAN_POINT('Ctrl Pts',(8.38096706211448,37.1247207489179,18.));
#28631=CARTESIAN_POINT('Ctrl Pts',(8.3449081895264,37.0365602155149,0.));
#28632=CARTESIAN_POINT('Ctrl Pts',(8.3449081895264,37.0365602155149,18.));
#28633=CARTESIAN_POINT('Ctrl Pts',(8.31052547794592,36.9479311729484,0.));
#28634=CARTESIAN_POINT('Ctrl Pts',(8.31052547794592,36.9479311729484,18.));
#28635=CARTESIAN_POINT('Ctrl Pts',(8.27886599440786,36.8585291300917,0.));
#28636=CARTESIAN_POINT('Ctrl Pts',(8.27886599440786,36.8585291300917,18.));
#28637=CARTESIAN_POINT('Ctrl Pts',(8.25656657451821,36.7861403757605,0.));
#28638=CARTESIAN_POINT('Ctrl Pts',(8.25656657451821,36.7861403757605,18.));
#28639=CARTESIAN_POINT('Ctrl Pts',(8.24192165947368,36.7312504697652,0.));
#28640=CARTESIAN_POINT('Ctrl Pts',(8.24192165947368,36.7312504697652,18.));
#28641=CARTESIAN_POINT('Ctrl Pts',(8.23313075335377,36.6943771018148,0.));
#28642=CARTESIAN_POINT('Ctrl Pts',(8.23313075335377,36.6943771018148,18.));
#28643=CARTESIAN_POINT('Ctrl Pts',(8.22897839625062,36.6758703925241,0.));
#28644=CARTESIAN_POINT('Ctrl Pts',(8.22897839625062,36.6758703925241,18.));
#28645=CARTESIAN_POINT('',(12.2684454652017,42.2550026135057,0.));
#28646=CARTESIAN_POINT('Ctrl Pts',(8.22897839625062,36.6758703925241,0.));
#28647=CARTESIAN_POINT('Ctrl Pts',(8.23313075335377,36.6943771018148,0.));
#28648=CARTESIAN_POINT('Ctrl Pts',(8.24192165947368,36.7312504697652,0.));
#28649=CARTESIAN_POINT('Ctrl Pts',(8.25656657451821,36.7861403757605,0.));
#28650=CARTESIAN_POINT('Ctrl Pts',(8.27886599440786,36.8585291300917,0.));
#28651=CARTESIAN_POINT('Ctrl Pts',(8.31052547794592,36.9479311729484,0.));
#28652=CARTESIAN_POINT('Ctrl Pts',(8.3449081895264,37.0365602155149,0.));
#28653=CARTESIAN_POINT('Ctrl Pts',(8.38096706211448,37.1247207489179,0.));
#28654=CARTESIAN_POINT('Ctrl Pts',(8.41793088313261,37.2126332013933,0.));
#28655=CARTESIAN_POINT('Ctrl Pts',(8.4555084943396,37.3003733151561,0.));
#28656=CARTESIAN_POINT('Ctrl Pts',(8.49372546467076,37.3879218093514,0.));
#28657=CARTESIAN_POINT('Ctrl Pts',(8.53279758643785,37.4752030152968,0.));
#28658=CARTESIAN_POINT('Ctrl Pts',(8.57299698459466,37.5621256752108,0.));
#28659=CARTESIAN_POINT('Ctrl Pts',(8.61450621749155,37.6486274754754,0.));
#28660=CARTESIAN_POINT('Ctrl Pts',(8.65732553894525,37.7347032383719,0.));
#28661=CARTESIAN_POINT('Ctrl Pts',(8.70134776631144,37.8203816669032,0.));
#28662=CARTESIAN_POINT('Ctrl Pts',(8.74640499479003,37.9057107230066,0.));
#28663=CARTESIAN_POINT('Ctrl Pts',(8.79232279131092,37.9907407304174,0.));
#28664=CARTESIAN_POINT('Ctrl Pts',(8.8389795976335,38.0755058326913,0.));
#28665=CARTESIAN_POINT('Ctrl Pts',(8.88633535238435,38.1600150482528,0.));
#28666=CARTESIAN_POINT('Ctrl Pts',(8.93439830996339,38.2442625706309,0.));
#28667=CARTESIAN_POINT('Ctrl Pts',(8.9832048378576,38.3282340281403,0.));
#28668=CARTESIAN_POINT('Ctrl Pts',(9.03279579360191,38.4119138099805,0.));
#28669=CARTESIAN_POINT('Ctrl Pts',(9.08319014288086,38.4952932486131,0.));
#28670=CARTESIAN_POINT('Ctrl Pts',(9.13437512010586,38.5783736628826,0.));
#28671=CARTESIAN_POINT('Ctrl Pts',(9.1863201939433,38.6611620045193,0.));
#28672=CARTESIAN_POINT('Ctrl Pts',(9.23898539199332,38.7436682576832,0.));
#28673=CARTESIAN_POINT('Ctrl Pts',(9.29233110570903,38.8259023794241,0.));
#28674=CARTESIAN_POINT('Ctrl Pts',(9.34632917154637,38.9078708427078,0.));
#28675=CARTESIAN_POINT('Ctrl Pts',(9.40096600877644,38.9895756526779,0.));
#28676=CARTESIAN_POINT('Ctrl Pts',(9.45623664577432,39.0710161994951,0.));
#28677=CARTESIAN_POINT('Ctrl Pts',(9.51214104535621,39.1521903958956,0.));
#28678=CARTESIAN_POINT('Ctrl Pts',(9.56867984233624,39.2330959982788,0.));
#28679=CARTESIAN_POINT('Ctrl Pts',(9.62584947846544,39.3137321153686,0.));
#28680=CARTESIAN_POINT('Ctrl Pts',(9.68364100883828,39.3940995760289,0.));
#28681=CARTESIAN_POINT('Ctrl Pts',(9.74204258152664,39.4742001555227,0.));
#28682=CARTESIAN_POINT('Ctrl Pts',(9.80104095251614,39.5540361022309,0.));
#28683=CARTESIAN_POINT('Ctrl Pts',(9.8606232424256,39.6336095893767,0.));
#28684=CARTESIAN_POINT('Ctrl Pts',(9.92077894513192,39.712922089547,0.));
#28685=CARTESIAN_POINT('Ctrl Pts',(9.98150036150824,39.7919742367922,0.));
#28686=CARTESIAN_POINT('Ctrl Pts',(10.0427815229883,39.8707661565233,0.));
#28687=CARTESIAN_POINT('Ctrl Pts',(10.1046175096878,39.9492976736738,0.));
#28688=CARTESIAN_POINT('Ctrl Pts',(10.1670036683795,40.0275685525923,0.));
#28689=CARTESIAN_POINT('Ctrl Pts',(10.2299347125857,40.1055787732578,0.));
#28690=CARTESIAN_POINT('Ctrl Pts',(10.2934044990237,40.1833286010098,0.));
#28691=CARTESIAN_POINT('Ctrl Pts',(10.3574064830678,40.2608184485326,0.));
#28692=CARTESIAN_POINT('Ctrl Pts',(10.4219339932951,40.3380487942952,0.));
#28693=CARTESIAN_POINT('Ctrl Pts',(10.48698054978,40.4150200869536,0.));
#28694=CARTESIAN_POINT('Ctrl Pts',(10.5525402237951,40.4917326404439,0.));
#28695=CARTESIAN_POINT('Ctrl Pts',(10.618607730849,40.5681866012103,0.));
#28696=CARTESIAN_POINT('Ctrl Pts',(10.6851782157325,40.6443819999244,0.));
#28697=CARTESIAN_POINT('Ctrl Pts',(10.7522471109694,40.7203187831783,0.));
#28698=CARTESIAN_POINT('Ctrl Pts',(10.8198099757795,40.7959968527561,0.));
#28699=CARTESIAN_POINT('Ctrl Pts',(10.8878623066646,40.8714161092412,0.));
#28700=CARTESIAN_POINT('Ctrl Pts',(10.956399476781,40.9465764747798,0.));
#28701=CARTESIAN_POINT('Ctrl Pts',(11.0254168609972,41.0214778832142,0.));
#28702=CARTESIAN_POINT('Ctrl Pts',(11.0949099155251,41.0961202807715,0.));
#28703=CARTESIAN_POINT('Ctrl Pts',(11.1648742640378,41.1705036228854,0.));
#28704=CARTESIAN_POINT('Ctrl Pts',(11.2353057980338,41.2446278781981,0.));
#28705=CARTESIAN_POINT('Ctrl Pts',(11.3062006993745,41.3184930194148,0.));
#28706=CARTESIAN_POINT('Ctrl Pts',(11.3775553120176,41.3920989905986,0.));
#28707=CARTESIAN_POINT('Ctrl Pts',(11.4493660393849,41.4654456796071,0.));
#28708=CARTESIAN_POINT('Ctrl Pts',(11.5216292382388,41.5385328935506,0.));
#28709=CARTESIAN_POINT('Ctrl Pts',(11.5943410868252,41.6113603270596,0.));
#28710=CARTESIAN_POINT('Ctrl Pts',(11.6674975352852,41.6839275596248,0.));
#28711=CARTESIAN_POINT('Ctrl Pts',(11.7410945211992,41.7562341395977,0.));
#28712=CARTESIAN_POINT('Ctrl Pts',(11.81512813804,41.8282796562569,0.));
#28713=CARTESIAN_POINT('Ctrl Pts',(11.8895948153349,41.9000638152266,0.));
#28714=CARTESIAN_POINT('Ctrl Pts',(11.9644914999263,41.9715865222182,0.));
#28715=CARTESIAN_POINT('Ctrl Pts',(12.054880669507,42.0571002269437,0.));
#28716=CARTESIAN_POINT('Ctrl Pts',(12.1307372881904,42.1280354231517,0.));
#28717=CARTESIAN_POINT('Ctrl Pts',(12.1917619768791,42.18457517013,0.));
#28718=CARTESIAN_POINT('Ctrl Pts',(12.2377212115625,42.2268628664988,0.));
#28719=CARTESIAN_POINT('Ctrl Pts',(12.2684454652018,42.2550026135057,0.));
#28720=CARTESIAN_POINT('',(12.2684454652017,42.2550026135057,15.));
#28721=CARTESIAN_POINT('Ctrl Pts',(12.2684454652018,42.2550026135057,15.));
#28722=CARTESIAN_POINT('Ctrl Pts',(12.2530833383985,42.2409327400055,15.));
#28723=CARTESIAN_POINT('Ctrl Pts',(12.222401466668,42.2127669677092,15.));
#28724=CARTESIAN_POINT('Ctrl Pts',(12.1765058047069,42.1704402333854,15.));
#28725=CARTESIAN_POINT('Ctrl Pts',(12.1155659644537,42.1138483839101,15.));
#28726=CARTESIAN_POINT('Ctrl Pts',(12.0398158079102,42.0428479428228,15.));
#28727=CARTESIAN_POINT('Ctrl Pts',(11.9644914999263,41.9715865222182,15.));
#28728=CARTESIAN_POINT('Ctrl Pts',(11.8895948153349,41.9000638152266,15.));
#28729=CARTESIAN_POINT('Ctrl Pts',(11.81512813804,41.8282796562569,15.));
#28730=CARTESIAN_POINT('Ctrl Pts',(11.7410945211992,41.7562341395977,15.));
#28731=CARTESIAN_POINT('Ctrl Pts',(11.6674975352852,41.6839275596248,15.));
#28732=CARTESIAN_POINT('Ctrl Pts',(11.5943410868252,41.6113603270596,15.));
#28733=CARTESIAN_POINT('Ctrl Pts',(11.5216292382388,41.5385328935506,15.));
#28734=CARTESIAN_POINT('Ctrl Pts',(11.4493660393849,41.4654456796071,15.));
#28735=CARTESIAN_POINT('Ctrl Pts',(11.3775553120176,41.3920989905986,15.));
#28736=CARTESIAN_POINT('Ctrl Pts',(11.3062006993745,41.3184930194148,15.));
#28737=CARTESIAN_POINT('Ctrl Pts',(11.2353057980338,41.2446278781981,15.));
#28738=CARTESIAN_POINT('Ctrl Pts',(11.1648742640378,41.1705036228854,15.));
#28739=CARTESIAN_POINT('Ctrl Pts',(11.0949099155251,41.0961202807715,15.));
#28740=CARTESIAN_POINT('Ctrl Pts',(11.0254168609972,41.0214778832142,15.));
#28741=CARTESIAN_POINT('Ctrl Pts',(10.956399476781,40.9465764747798,15.));
#28742=CARTESIAN_POINT('Ctrl Pts',(10.8878623066646,40.8714161092412,15.));
#28743=CARTESIAN_POINT('Ctrl Pts',(10.8198099757795,40.7959968527561,15.));
#28744=CARTESIAN_POINT('Ctrl Pts',(10.7522471109694,40.7203187831783,15.));
#28745=CARTESIAN_POINT('Ctrl Pts',(10.6851782157325,40.6443819999244,15.));
#28746=CARTESIAN_POINT('Ctrl Pts',(10.618607730849,40.5681866012103,15.));
#28747=CARTESIAN_POINT('Ctrl Pts',(10.5525402237951,40.4917326404439,15.));
#28748=CARTESIAN_POINT('Ctrl Pts',(10.48698054978,40.4150200869536,15.));
#28749=CARTESIAN_POINT('Ctrl Pts',(10.4219339932951,40.3380487942952,15.));
#28750=CARTESIAN_POINT('Ctrl Pts',(10.3574064830678,40.2608184485326,15.));
#28751=CARTESIAN_POINT('Ctrl Pts',(10.2934044990237,40.1833286010098,15.));
#28752=CARTESIAN_POINT('Ctrl Pts',(10.2299347125857,40.1055787732578,15.));
#28753=CARTESIAN_POINT('Ctrl Pts',(10.1670036683795,40.0275685525923,15.));
#28754=CARTESIAN_POINT('Ctrl Pts',(10.1046175096878,39.9492976736738,15.));
#28755=CARTESIAN_POINT('Ctrl Pts',(10.0427815229883,39.8707661565233,15.));
#28756=CARTESIAN_POINT('Ctrl Pts',(9.98150036150824,39.7919742367922,15.));
#28757=CARTESIAN_POINT('Ctrl Pts',(9.92077894513192,39.712922089547,15.));
#28758=CARTESIAN_POINT('Ctrl Pts',(9.8606232424256,39.6336095893767,15.));
#28759=CARTESIAN_POINT('Ctrl Pts',(9.80104095251614,39.5540361022309,15.));
#28760=CARTESIAN_POINT('Ctrl Pts',(9.74204258152664,39.4742001555227,15.));
#28761=CARTESIAN_POINT('Ctrl Pts',(9.68364100883828,39.3940995760289,15.));
#28762=CARTESIAN_POINT('Ctrl Pts',(9.62584947846544,39.3137321153686,15.));
#28763=CARTESIAN_POINT('Ctrl Pts',(9.56867984233624,39.2330959982788,15.));
#28764=CARTESIAN_POINT('Ctrl Pts',(9.51214104535621,39.1521903958956,15.));
#28765=CARTESIAN_POINT('Ctrl Pts',(9.45623664577432,39.0710161994951,15.));
#28766=CARTESIAN_POINT('Ctrl Pts',(9.40096600877644,38.9895756526779,15.));
#28767=CARTESIAN_POINT('Ctrl Pts',(9.34632917154637,38.9078708427078,15.));
#28768=CARTESIAN_POINT('Ctrl Pts',(9.29233110570903,38.8259023794241,15.));
#28769=CARTESIAN_POINT('Ctrl Pts',(9.23898539199332,38.7436682576832,15.));
#28770=CARTESIAN_POINT('Ctrl Pts',(9.1863201939433,38.6611620045193,15.));
#28771=CARTESIAN_POINT('Ctrl Pts',(9.13437512010586,38.5783736628826,15.));
#28772=CARTESIAN_POINT('Ctrl Pts',(9.08319014288086,38.4952932486131,15.));
#28773=CARTESIAN_POINT('Ctrl Pts',(9.03279579360191,38.4119138099805,15.));
#28774=CARTESIAN_POINT('Ctrl Pts',(8.9832048378576,38.3282340281403,15.));
#28775=CARTESIAN_POINT('Ctrl Pts',(8.93439830996339,38.2442625706309,15.));
#28776=CARTESIAN_POINT('Ctrl Pts',(8.88633535238435,38.1600150482528,15.));
#28777=CARTESIAN_POINT('Ctrl Pts',(8.8389795976335,38.0755058326913,15.));
#28778=CARTESIAN_POINT('Ctrl Pts',(8.79232279131092,37.9907407304174,15.));
#28779=CARTESIAN_POINT('Ctrl Pts',(8.74640499479003,37.9057107230066,15.));
#28780=CARTESIAN_POINT('Ctrl Pts',(8.70134776631144,37.8203816669032,15.));
#28781=CARTESIAN_POINT('Ctrl Pts',(8.65732553894525,37.7347032383719,15.));
#28782=CARTESIAN_POINT('Ctrl Pts',(8.61450621749155,37.6486274754754,15.));
#28783=CARTESIAN_POINT('Ctrl Pts',(8.57299698459466,37.5621256752108,15.));
#28784=CARTESIAN_POINT('Ctrl Pts',(8.53279758643785,37.4752030152968,15.));
#28785=CARTESIAN_POINT('Ctrl Pts',(8.49372546467076,37.3879218093514,15.));
#28786=CARTESIAN_POINT('Ctrl Pts',(8.4555084943396,37.3003733151561,15.));
#28787=CARTESIAN_POINT('Ctrl Pts',(8.41793088313261,37.2126332013933,15.));
#28788=CARTESIAN_POINT('Ctrl Pts',(8.38096706211448,37.1247207489179,15.));
#28789=CARTESIAN_POINT('Ctrl Pts',(8.3449081895264,37.0365602155149,15.));
#28790=CARTESIAN_POINT('Ctrl Pts',(8.31052547794592,36.9479311729484,15.));
#28791=CARTESIAN_POINT('Ctrl Pts',(8.27886599440786,36.8585291300917,15.));
#28792=CARTESIAN_POINT('Ctrl Pts',(8.25656657451821,36.7861403757605,15.));
#28793=CARTESIAN_POINT('Ctrl Pts',(8.24192165947368,36.7312504697652,15.));
#28794=CARTESIAN_POINT('Ctrl Pts',(8.23313075335377,36.6943771018148,15.));
#28795=CARTESIAN_POINT('Ctrl Pts',(8.22897839625062,36.6758703925241,15.));
#28796=CARTESIAN_POINT('',(12.2684454652017,42.2550026135057,0.));
#28797=CARTESIAN_POINT('Origin',(3.50213800024364E-12,1.07784724682657E-11,
0.));
#28798=CARTESIAN_POINT('',(14.911486495888,41.396226524684,0.));
#28799=CARTESIAN_POINT('Origin',(3.50213800024364E-12,1.07784724682657E-11,
0.));
#28800=CARTESIAN_POINT('',(14.911486495888,41.396226524684,15.));
#28801=CARTESIAN_POINT('Origin',(3.50213800024364E-12,1.07784724682657E-11,
15.));
#28802=CARTESIAN_POINT('',(14.911486495888,41.396226524684,0.));
#28803=CARTESIAN_POINT('Ctrl Pts',(14.9001523628048,34.5082745737944,0.));
#28804=CARTESIAN_POINT('Ctrl Pts',(14.9001523628048,34.5082745737944,18.));
#28805=CARTESIAN_POINT('Ctrl Pts',(14.9076710061311,34.525687510388,0.));
#28806=CARTESIAN_POINT('Ctrl Pts',(14.9076710061311,34.525687510388,18.));
#28807=CARTESIAN_POINT('Ctrl Pts',(14.9222326355678,34.5606858566713,0.));
#28808=CARTESIAN_POINT('Ctrl Pts',(14.9222326355678,34.5606858566713,18.));
#28809=CARTESIAN_POINT('Ctrl Pts',(14.9426481276593,34.6137007885254,0.));
#28810=CARTESIAN_POINT('Ctrl Pts',(14.9426481276593,34.6137007885254,18.));
#28811=CARTESIAN_POINT('Ctrl Pts',(14.9671565602316,34.6853717911269,0.));
#28812=CARTESIAN_POINT('Ctrl Pts',(14.9671565602316,34.6853717911269,18.));
#28813=CARTESIAN_POINT('Ctrl Pts',(14.9940927023322,34.7763085406486,0.));
#28814=CARTESIAN_POINT('Ctrl Pts',(14.9940927023322,34.7763085406486,18.));
#28815=CARTESIAN_POINT('Ctrl Pts',(15.0183713484962,34.8682205930809,0.));
#28816=CARTESIAN_POINT('Ctrl Pts',(15.0183713484962,34.8682205930809,18.));
#28817=CARTESIAN_POINT('Ctrl Pts',(15.041018569143,34.9607388363587,0.));
#28818=CARTESIAN_POINT('Ctrl Pts',(15.041018569143,34.9607388363587,18.));
#28819=CARTESIAN_POINT('Ctrl Pts',(15.0627878528202,35.0535882932913,0.));
#28820=CARTESIAN_POINT('Ctrl Pts',(15.0627878528202,35.0535882932913,18.));
#28821=CARTESIAN_POINT('Ctrl Pts',(15.08395927165,35.1466591020976,0.));
#28822=CARTESIAN_POINT('Ctrl Pts',(15.08395927165,35.1466591020976,18.));
#28823=CARTESIAN_POINT('Ctrl Pts',(15.104500806927,35.2399506932815,0.));
#28824=CARTESIAN_POINT('Ctrl Pts',(15.104500806927,35.2399506932815,18.));
#28825=CARTESIAN_POINT('Ctrl Pts',(15.1241934020682,35.3335286891314,0.));
#28826=CARTESIAN_POINT('Ctrl Pts',(15.1241934020682,35.3335286891314,18.));
#28827=CARTESIAN_POINT('Ctrl Pts',(15.1427632633831,35.4274792115857,0.));
#28828=CARTESIAN_POINT('Ctrl Pts',(15.1427632633831,35.4274792115857,18.));
#28829=CARTESIAN_POINT('Ctrl Pts',(15.1600260710384,35.5218591529746,0.));
#28830=CARTESIAN_POINT('Ctrl Pts',(15.1600260710384,35.5218591529746,18.));
#28831=CARTESIAN_POINT('Ctrl Pts',(15.1759785763051,35.6166644736253,0.));
#28832=CARTESIAN_POINT('Ctrl Pts',(15.1759785763051,35.6166644736253,18.));
#28833=CARTESIAN_POINT('Ctrl Pts',(15.1907243629659,35.7118553943773,0.));
#28834=CARTESIAN_POINT('Ctrl Pts',(15.1907243629659,35.7118553943773,18.));
#28835=CARTESIAN_POINT('Ctrl Pts',(15.2044274601769,35.8073720252878,0.));
#28836=CARTESIAN_POINT('Ctrl Pts',(15.2044274601769,35.8073720252878,18.));
#28837=CARTESIAN_POINT('Ctrl Pts',(15.2172585668056,35.9031525499277,0.));
#28838=CARTESIAN_POINT('Ctrl Pts',(15.2172585668056,35.9031525499277,18.));
#28839=CARTESIAN_POINT('Ctrl Pts',(15.2293360946131,35.9991531408727,0.));
#28840=CARTESIAN_POINT('Ctrl Pts',(15.2293360946131,35.9991531408727,18.));
#28841=CARTESIAN_POINT('Ctrl Pts',(15.240697754828,36.095357546697,0.));
#28842=CARTESIAN_POINT('Ctrl Pts',(15.240697754828,36.095357546697,18.));
#28843=CARTESIAN_POINT('Ctrl Pts',(15.2513334565427,36.1917659216814,0.));
#28844=CARTESIAN_POINT('Ctrl Pts',(15.2513334565427,36.1917659216814,18.));
#28845=CARTESIAN_POINT('Ctrl Pts',(15.2612053303774,36.2883880151607,0.));
#28846=CARTESIAN_POINT('Ctrl Pts',(15.2612053303774,36.2883880151607,18.));
#28847=CARTESIAN_POINT('Ctrl Pts',(15.2702711460937,36.3852352131887,0.));
#28848=CARTESIAN_POINT('Ctrl Pts',(15.2702711460937,36.3852352131887,18.));
#28849=CARTESIAN_POINT('Ctrl Pts',(15.2785104654792,36.4823116513289,0.));
#28850=CARTESIAN_POINT('Ctrl Pts',(15.2785104654792,36.4823116513289,18.));
#28851=CARTESIAN_POINT('Ctrl Pts',(15.2859343913094,36.5796108931244,0.));
#28852=CARTESIAN_POINT('Ctrl Pts',(15.2859343913094,36.5796108931244,18.));
#28853=CARTESIAN_POINT('Ctrl Pts',(15.2925717100767,36.6771206167756,0.));
#28854=CARTESIAN_POINT('Ctrl Pts',(15.2925717100767,36.6771206167756,18.));
#28855=CARTESIAN_POINT('Ctrl Pts',(15.2984606286737,36.7748254044502,0.));
#28856=CARTESIAN_POINT('Ctrl Pts',(15.2984606286737,36.7748254044502,18.));
#28857=CARTESIAN_POINT('Ctrl Pts',(15.3036390436952,36.8727100302512,0.));
#28858=CARTESIAN_POINT('Ctrl Pts',(15.3036390436952,36.8727100302512,18.));
#28859=CARTESIAN_POINT('Ctrl Pts',(15.3081335446406,36.970763176802,0.));
#28860=CARTESIAN_POINT('Ctrl Pts',(15.3081335446406,36.970763176802,18.));
#28861=CARTESIAN_POINT('Ctrl Pts',(15.3119562971444,37.0689784837457,0.));
#28862=CARTESIAN_POINT('Ctrl Pts',(15.3119562971444,37.0689784837457,18.));
#28863=CARTESIAN_POINT('Ctrl Pts',(15.3151109648809,37.1673525354642,0.));
#28864=CARTESIAN_POINT('Ctrl Pts',(15.3151109648809,37.1673525354642,18.));
#28865=CARTESIAN_POINT('Ctrl Pts',(15.3175963510698,37.2658836214694,0.));
#28866=CARTESIAN_POINT('Ctrl Pts',(15.3175963510698,37.2658836214694,18.));
#28867=CARTESIAN_POINT('Ctrl Pts',(15.3194106233801,37.3645702997848,0.));
#28868=CARTESIAN_POINT('Ctrl Pts',(15.3194106233801,37.3645702997848,18.));
#28869=CARTESIAN_POINT('Ctrl Pts',(15.3205561366169,37.4634097578665,0.));
#28870=CARTESIAN_POINT('Ctrl Pts',(15.3205561366169,37.4634097578665,18.));
#28871=CARTESIAN_POINT('Ctrl Pts',(15.3210406145546,37.562397408596,0.));
#28872=CARTESIAN_POINT('Ctrl Pts',(15.3210406145546,37.562397408596,18.));
#28873=CARTESIAN_POINT('Ctrl Pts',(15.3208746890781,37.6615277218027,0.));
#28874=CARTESIAN_POINT('Ctrl Pts',(15.3208746890781,37.6615277218027,18.));
#28875=CARTESIAN_POINT('Ctrl Pts',(15.320070396385,37.7607947318286,0.));
#28876=CARTESIAN_POINT('Ctrl Pts',(15.320070396385,37.7607947318286,18.));
#28877=CARTESIAN_POINT('Ctrl Pts',(15.3186394335023,37.8601926265378,0.));
#28878=CARTESIAN_POINT('Ctrl Pts',(15.3186394335023,37.8601926265378,18.));
#28879=CARTESIAN_POINT('Ctrl Pts',(15.3165911656268,37.959716421934,0.));
#28880=CARTESIAN_POINT('Ctrl Pts',(15.3165911656268,37.959716421934,18.));
#28881=CARTESIAN_POINT('Ctrl Pts',(15.3139321941687,38.0593621055415,0.));
#28882=CARTESIAN_POINT('Ctrl Pts',(15.3139321941687,38.0593621055415,18.));
#28883=CARTESIAN_POINT('Ctrl Pts',(15.310667421514,38.1591262705847,0.));
#28884=CARTESIAN_POINT('Ctrl Pts',(15.310667421514,38.1591262705847,18.));
#28885=CARTESIAN_POINT('Ctrl Pts',(15.3068007250314,38.2590058835965,0.));
#28886=CARTESIAN_POINT('Ctrl Pts',(15.3068007250314,38.2590058835965,18.));
#28887=CARTESIAN_POINT('Ctrl Pts',(15.3023357307483,38.3589980188324,0.));
#28888=CARTESIAN_POINT('Ctrl Pts',(15.3023357307483,38.3589980188324,18.));
#28889=CARTESIAN_POINT('Ctrl Pts',(15.297276703747,38.4590995527814,0.));
#28890=CARTESIAN_POINT('Ctrl Pts',(15.297276703747,38.4590995527814,18.));
#28891=CARTESIAN_POINT('Ctrl Pts',(15.2916287700102,38.5593070891769,0.));
#28892=CARTESIAN_POINT('Ctrl Pts',(15.2916287700102,38.5593070891769,18.));
#28893=CARTESIAN_POINT('Ctrl Pts',(15.2853974668211,38.659617115053,0.));
#28894=CARTESIAN_POINT('Ctrl Pts',(15.2853974668211,38.659617115053,18.));
#28895=CARTESIAN_POINT('Ctrl Pts',(15.2785884727112,38.7600260961351,0.));
#28896=CARTESIAN_POINT('Ctrl Pts',(15.2785884727112,38.7600260961351,18.));
#28897=CARTESIAN_POINT('Ctrl Pts',(15.2712072937639,38.860530586589,0.));
#28898=CARTESIAN_POINT('Ctrl Pts',(15.2712072937639,38.860530586589,18.));
#28899=CARTESIAN_POINT('Ctrl Pts',(15.2632589109473,38.9611273555758,0.));
#28900=CARTESIAN_POINT('Ctrl Pts',(15.2632589109473,38.9611273555758,18.));
#28901=CARTESIAN_POINT('Ctrl Pts',(15.2547476855825,39.061813415425,0.));
#28902=CARTESIAN_POINT('Ctrl Pts',(15.2547476855825,39.061813415425,18.));
#28903=CARTESIAN_POINT('Ctrl Pts',(15.2456775636447,39.1625859371304,0.));
#28904=CARTESIAN_POINT('Ctrl Pts',(15.2456775636447,39.1625859371304,18.));
#28905=CARTESIAN_POINT('Ctrl Pts',(15.2360522089072,39.2634421927888,0.));
#28906=CARTESIAN_POINT('Ctrl Pts',(15.2360522089072,39.2634421927888,18.));
#28907=CARTESIAN_POINT('Ctrl Pts',(15.225875156307,39.3643794927167,0.));
#28908=CARTESIAN_POINT('Ctrl Pts',(15.225875156307,39.3643794927167,18.));
#28909=CARTESIAN_POINT('Ctrl Pts',(15.2151499908149,39.4653951093947,0.));
#28910=CARTESIAN_POINT('Ctrl Pts',(15.2151499908149,39.4653951093947,18.));
#28911=CARTESIAN_POINT('Ctrl Pts',(15.2038804098649,39.5664862602472,0.));
#28912=CARTESIAN_POINT('Ctrl Pts',(15.2038804098649,39.5664862602472,18.));
#28913=CARTESIAN_POINT('Ctrl Pts',(15.1920701163804,39.6676501731673,0.));
#28914=CARTESIAN_POINT('Ctrl Pts',(15.1920701163804,39.6676501731673,18.));
#28915=CARTESIAN_POINT('Ctrl Pts',(15.1797227547562,39.7688841338802,0.));
#28916=CARTESIAN_POINT('Ctrl Pts',(15.1797227547562,39.7688841338802,18.));
#28917=CARTESIAN_POINT('Ctrl Pts',(15.1668418393198,39.8701855339908,0.));
#28918=CARTESIAN_POINT('Ctrl Pts',(15.1668418393198,39.8701855339908,18.));
#28919=CARTESIAN_POINT('Ctrl Pts',(15.1534306754871,39.9715519332134,0.));
#28920=CARTESIAN_POINT('Ctrl Pts',(15.1534306754871,39.9715519332134,18.));
#28921=CARTESIAN_POINT('Ctrl Pts',(15.1394923361537,40.0729810652204,0.));
#28922=CARTESIAN_POINT('Ctrl Pts',(15.1394923361537,40.0729810652204,18.));
#28923=CARTESIAN_POINT('Ctrl Pts',(15.1250297462408,40.1744707357902,0.));
#28924=CARTESIAN_POINT('Ctrl Pts',(15.1250297462408,40.1744707357902,18.));
#28925=CARTESIAN_POINT('Ctrl Pts',(15.1100457495259,40.2760187401822,0.));
#28926=CARTESIAN_POINT('Ctrl Pts',(15.1100457495259,40.2760187401822,18.));
#28927=CARTESIAN_POINT('Ctrl Pts',(15.0945431800724,40.3776227809037,0.));
#28928=CARTESIAN_POINT('Ctrl Pts',(15.0945431800724,40.3776227809037,18.));
#28929=CARTESIAN_POINT('Ctrl Pts',(15.0785249502524,40.4792803645352,0.));
#28930=CARTESIAN_POINT('Ctrl Pts',(15.0785249502524,40.4792803645352,18.));
#28931=CARTESIAN_POINT('Ctrl Pts',(15.0619940893017,40.5809887704301,0.));
#28932=CARTESIAN_POINT('Ctrl Pts',(15.0619940893017,40.5809887704301,18.));
#28933=CARTESIAN_POINT('Ctrl Pts',(15.0449536183143,40.6827452453667,0.));
#28934=CARTESIAN_POINT('Ctrl Pts',(15.0449536183143,40.6827452453667,18.));
#28935=CARTESIAN_POINT('Ctrl Pts',(15.0274064563211,40.7845471608654,0.));
#28936=CARTESIAN_POINT('Ctrl Pts',(15.0274064563211,40.7845471608654,18.));
#28937=CARTESIAN_POINT('Ctrl Pts',(15.0093553188655,40.8863921801,0.));
#28938=CARTESIAN_POINT('Ctrl Pts',(15.0093553188655,40.8863921801,18.));
#28939=CARTESIAN_POINT('Ctrl Pts',(14.9908026205824,40.9882784321884,0.));
#28940=CARTESIAN_POINT('Ctrl Pts',(14.9908026205824,40.9882784321884,18.));
#28941=CARTESIAN_POINT('Ctrl Pts',(14.9717503874227,41.0902046498729,0.));
#28942=CARTESIAN_POINT('Ctrl Pts',(14.9717503874227,41.0902046498729,18.));
#28943=CARTESIAN_POINT('Ctrl Pts',(14.9522002356298,41.1921700381957,0.));
#28944=CARTESIAN_POINT('Ctrl Pts',(14.9522002356298,41.1921700381957,18.));
#28945=CARTESIAN_POINT('Ctrl Pts',(14.936162723752,41.2737733455422,0.));
#28946=CARTESIAN_POINT('Ctrl Pts',(14.936162723752,41.2737733455422,18.));
#28947=CARTESIAN_POINT('Ctrl Pts',(14.9239113834707,41.3349931861715,0.));
#28948=CARTESIAN_POINT('Ctrl Pts',(14.9239113834707,41.3349931861715,18.));
#28949=CARTESIAN_POINT('Ctrl Pts',(14.9156446533966,41.3758141263348,0.));
#28950=CARTESIAN_POINT('Ctrl Pts',(14.9156446533966,41.3758141263348,18.));
#28951=CARTESIAN_POINT('Ctrl Pts',(14.911486495888,41.396226524684,0.));
#28952=CARTESIAN_POINT('Ctrl Pts',(14.911486495888,41.396226524684,18.));
#28953=CARTESIAN_POINT('Ctrl Pts',(14.9001523628048,34.5082745737944,0.));
#28954=CARTESIAN_POINT('Ctrl Pts',(14.9076710061311,34.525687510388,0.));
#28955=CARTESIAN_POINT('Ctrl Pts',(14.9222326355678,34.5606858566713,0.));
#28956=CARTESIAN_POINT('Ctrl Pts',(14.9426481276593,34.6137007885254,0.));
#28957=CARTESIAN_POINT('Ctrl Pts',(14.9671565602316,34.6853717911269,0.));
#28958=CARTESIAN_POINT('Ctrl Pts',(14.9940927023322,34.7763085406486,0.));
#28959=CARTESIAN_POINT('Ctrl Pts',(15.0183713484962,34.8682205930809,0.));
#28960=CARTESIAN_POINT('Ctrl Pts',(15.041018569143,34.9607388363587,0.));
#28961=CARTESIAN_POINT('Ctrl Pts',(15.0627878528202,35.0535882932913,0.));
#28962=CARTESIAN_POINT('Ctrl Pts',(15.08395927165,35.1466591020976,0.));
#28963=CARTESIAN_POINT('Ctrl Pts',(15.104500806927,35.2399506932815,0.));
#28964=CARTESIAN_POINT('Ctrl Pts',(15.1241934020682,35.3335286891314,0.));
#28965=CARTESIAN_POINT('Ctrl Pts',(15.1427632633831,35.4274792115857,0.));
#28966=CARTESIAN_POINT('Ctrl Pts',(15.1600260710384,35.5218591529746,0.));
#28967=CARTESIAN_POINT('Ctrl Pts',(15.1759785763051,35.6166644736253,0.));
#28968=CARTESIAN_POINT('Ctrl Pts',(15.1907243629659,35.7118553943773,0.));
#28969=CARTESIAN_POINT('Ctrl Pts',(15.2044274601769,35.8073720252878,0.));
#28970=CARTESIAN_POINT('Ctrl Pts',(15.2172585668056,35.9031525499277,0.));
#28971=CARTESIAN_POINT('Ctrl Pts',(15.2293360946131,35.9991531408727,0.));
#28972=CARTESIAN_POINT('Ctrl Pts',(15.240697754828,36.095357546697,0.));
#28973=CARTESIAN_POINT('Ctrl Pts',(15.2513334565427,36.1917659216814,0.));
#28974=CARTESIAN_POINT('Ctrl Pts',(15.2612053303774,36.2883880151607,0.));
#28975=CARTESIAN_POINT('Ctrl Pts',(15.2702711460937,36.3852352131887,0.));
#28976=CARTESIAN_POINT('Ctrl Pts',(15.2785104654792,36.4823116513289,0.));
#28977=CARTESIAN_POINT('Ctrl Pts',(15.2859343913094,36.5796108931244,0.));
#28978=CARTESIAN_POINT('Ctrl Pts',(15.2925717100767,36.6771206167756,0.));
#28979=CARTESIAN_POINT('Ctrl Pts',(15.2984606286737,36.7748254044502,0.));
#28980=CARTESIAN_POINT('Ctrl Pts',(15.3036390436952,36.8727100302512,0.));
#28981=CARTESIAN_POINT('Ctrl Pts',(15.3081335446406,36.970763176802,0.));
#28982=CARTESIAN_POINT('Ctrl Pts',(15.3119562971444,37.0689784837457,0.));
#28983=CARTESIAN_POINT('Ctrl Pts',(15.3151109648809,37.1673525354642,0.));
#28984=CARTESIAN_POINT('Ctrl Pts',(15.3175963510698,37.2658836214694,0.));
#28985=CARTESIAN_POINT('Ctrl Pts',(15.3194106233801,37.3645702997848,0.));
#28986=CARTESIAN_POINT('Ctrl Pts',(15.3205561366169,37.4634097578665,0.));
#28987=CARTESIAN_POINT('Ctrl Pts',(15.3210406145546,37.562397408596,0.));
#28988=CARTESIAN_POINT('Ctrl Pts',(15.3208746890781,37.6615277218027,0.));
#28989=CARTESIAN_POINT('Ctrl Pts',(15.320070396385,37.7607947318286,0.));
#28990=CARTESIAN_POINT('Ctrl Pts',(15.3186394335023,37.8601926265378,0.));
#28991=CARTESIAN_POINT('Ctrl Pts',(15.3165911656268,37.959716421934,0.));
#28992=CARTESIAN_POINT('Ctrl Pts',(15.3139321941687,38.0593621055415,0.));
#28993=CARTESIAN_POINT('Ctrl Pts',(15.310667421514,38.1591262705847,0.));
#28994=CARTESIAN_POINT('Ctrl Pts',(15.3068007250314,38.2590058835965,0.));
#28995=CARTESIAN_POINT('Ctrl Pts',(15.3023357307483,38.3589980188324,0.));
#28996=CARTESIAN_POINT('Ctrl Pts',(15.297276703747,38.4590995527814,0.));
#28997=CARTESIAN_POINT('Ctrl Pts',(15.2916287700102,38.5593070891769,0.));
#28998=CARTESIAN_POINT('Ctrl Pts',(15.2853974668211,38.659617115053,0.));
#28999=CARTESIAN_POINT('Ctrl Pts',(15.2785884727112,38.7600260961351,0.));
#29000=CARTESIAN_POINT('Ctrl Pts',(15.2712072937639,38.860530586589,0.));
#29001=CARTESIAN_POINT('Ctrl Pts',(15.2632589109473,38.9611273555758,0.));
#29002=CARTESIAN_POINT('Ctrl Pts',(15.2547476855825,39.061813415425,0.));
#29003=CARTESIAN_POINT('Ctrl Pts',(15.2456775636447,39.1625859371304,0.));
#29004=CARTESIAN_POINT('Ctrl Pts',(15.2360522089072,39.2634421927888,0.));
#29005=CARTESIAN_POINT('Ctrl Pts',(15.225875156307,39.3643794927167,0.));
#29006=CARTESIAN_POINT('Ctrl Pts',(15.2151499908149,39.4653951093947,0.));
#29007=CARTESIAN_POINT('Ctrl Pts',(15.2038804098649,39.5664862602472,0.));
#29008=CARTESIAN_POINT('Ctrl Pts',(15.1920701163804,39.6676501731673,0.));
#29009=CARTESIAN_POINT('Ctrl Pts',(15.1797227547562,39.7688841338802,0.));
#29010=CARTESIAN_POINT('Ctrl Pts',(15.1668418393198,39.8701855339908,0.));
#29011=CARTESIAN_POINT('Ctrl Pts',(15.1534306754871,39.9715519332134,0.));
#29012=CARTESIAN_POINT('Ctrl Pts',(15.1394923361537,40.0729810652204,0.));
#29013=CARTESIAN_POINT('Ctrl Pts',(15.1250297462408,40.1744707357902,0.));
#29014=CARTESIAN_POINT('Ctrl Pts',(15.1100457495259,40.2760187401822,0.));
#29015=CARTESIAN_POINT('Ctrl Pts',(15.0945431800724,40.3776227809037,0.));
#29016=CARTESIAN_POINT('Ctrl Pts',(15.0785249502524,40.4792803645352,0.));
#29017=CARTESIAN_POINT('Ctrl Pts',(15.0619940893017,40.5809887704301,0.));
#29018=CARTESIAN_POINT('Ctrl Pts',(15.0449536183143,40.6827452453667,0.));
#29019=CARTESIAN_POINT('Ctrl Pts',(15.0274064563211,40.7845471608654,0.));
#29020=CARTESIAN_POINT('Ctrl Pts',(15.0093553188655,40.8863921801,0.));
#29021=CARTESIAN_POINT('Ctrl Pts',(14.9908026205824,40.9882784321884,0.));
#29022=CARTESIAN_POINT('Ctrl Pts',(14.9679399407908,41.1105898934098,0.));
#29023=CARTESIAN_POINT('Ctrl Pts',(14.9482653093396,41.2125650743922,0.));
#29024=CARTESIAN_POINT('Ctrl Pts',(14.9321285285561,41.2941761025922,0.));
#29025=CARTESIAN_POINT('Ctrl Pts',(14.919802810928,41.3554017279611,0.));
#29026=CARTESIAN_POINT('Ctrl Pts',(14.911486495888,41.396226524684,0.));
#29027=CARTESIAN_POINT('Ctrl Pts',(14.9001523628048,34.5082745737944,15.));
#29028=CARTESIAN_POINT('Ctrl Pts',(14.9076710061311,34.525687510388,15.));
#29029=CARTESIAN_POINT('Ctrl Pts',(14.9222326355678,34.5606858566713,15.));
#29030=CARTESIAN_POINT('Ctrl Pts',(14.9426481276593,34.6137007885254,15.));
#29031=CARTESIAN_POINT('Ctrl Pts',(14.9671565602316,34.6853717911269,15.));
#29032=CARTESIAN_POINT('Ctrl Pts',(14.9940927023322,34.7763085406486,15.));
#29033=CARTESIAN_POINT('Ctrl Pts',(15.0183713484962,34.8682205930809,15.));
#29034=CARTESIAN_POINT('Ctrl Pts',(15.041018569143,34.9607388363587,15.));
#29035=CARTESIAN_POINT('Ctrl Pts',(15.0627878528202,35.0535882932913,15.));
#29036=CARTESIAN_POINT('Ctrl Pts',(15.08395927165,35.1466591020976,15.));
#29037=CARTESIAN_POINT('Ctrl Pts',(15.104500806927,35.2399506932815,15.));
#29038=CARTESIAN_POINT('Ctrl Pts',(15.1241934020682,35.3335286891314,15.));
#29039=CARTESIAN_POINT('Ctrl Pts',(15.1427632633831,35.4274792115857,15.));
#29040=CARTESIAN_POINT('Ctrl Pts',(15.1600260710384,35.5218591529746,15.));
#29041=CARTESIAN_POINT('Ctrl Pts',(15.1759785763051,35.6166644736253,15.));
#29042=CARTESIAN_POINT('Ctrl Pts',(15.1907243629659,35.7118553943773,15.));
#29043=CARTESIAN_POINT('Ctrl Pts',(15.2044274601769,35.8073720252878,15.));
#29044=CARTESIAN_POINT('Ctrl Pts',(15.2172585668056,35.9031525499277,15.));
#29045=CARTESIAN_POINT('Ctrl Pts',(15.2293360946131,35.9991531408727,15.));
#29046=CARTESIAN_POINT('Ctrl Pts',(15.240697754828,36.095357546697,15.));
#29047=CARTESIAN_POINT('Ctrl Pts',(15.2513334565427,36.1917659216814,15.));
#29048=CARTESIAN_POINT('Ctrl Pts',(15.2612053303774,36.2883880151607,15.));
#29049=CARTESIAN_POINT('Ctrl Pts',(15.2702711460937,36.3852352131887,15.));
#29050=CARTESIAN_POINT('Ctrl Pts',(15.2785104654792,36.4823116513289,15.));
#29051=CARTESIAN_POINT('Ctrl Pts',(15.2859343913094,36.5796108931244,15.));
#29052=CARTESIAN_POINT('Ctrl Pts',(15.2925717100767,36.6771206167756,15.));
#29053=CARTESIAN_POINT('Ctrl Pts',(15.2984606286737,36.7748254044502,15.));
#29054=CARTESIAN_POINT('Ctrl Pts',(15.3036390436952,36.8727100302512,15.));
#29055=CARTESIAN_POINT('Ctrl Pts',(15.3081335446406,36.970763176802,15.));
#29056=CARTESIAN_POINT('Ctrl Pts',(15.3119562971444,37.0689784837457,15.));
#29057=CARTESIAN_POINT('Ctrl Pts',(15.3151109648809,37.1673525354642,15.));
#29058=CARTESIAN_POINT('Ctrl Pts',(15.3175963510698,37.2658836214694,15.));
#29059=CARTESIAN_POINT('Ctrl Pts',(15.3194106233801,37.3645702997848,15.));
#29060=CARTESIAN_POINT('Ctrl Pts',(15.3205561366169,37.4634097578665,15.));
#29061=CARTESIAN_POINT('Ctrl Pts',(15.3210406145546,37.562397408596,15.));
#29062=CARTESIAN_POINT('Ctrl Pts',(15.3208746890781,37.6615277218027,15.));
#29063=CARTESIAN_POINT('Ctrl Pts',(15.320070396385,37.7607947318286,15.));
#29064=CARTESIAN_POINT('Ctrl Pts',(15.3186394335023,37.8601926265378,15.));
#29065=CARTESIAN_POINT('Ctrl Pts',(15.3165911656268,37.959716421934,15.));
#29066=CARTESIAN_POINT('Ctrl Pts',(15.3139321941687,38.0593621055415,15.));
#29067=CARTESIAN_POINT('Ctrl Pts',(15.310667421514,38.1591262705847,15.));
#29068=CARTESIAN_POINT('Ctrl Pts',(15.3068007250314,38.2590058835965,15.));
#29069=CARTESIAN_POINT('Ctrl Pts',(15.3023357307483,38.3589980188324,15.));
#29070=CARTESIAN_POINT('Ctrl Pts',(15.297276703747,38.4590995527814,15.));
#29071=CARTESIAN_POINT('Ctrl Pts',(15.2916287700102,38.5593070891769,15.));
#29072=CARTESIAN_POINT('Ctrl Pts',(15.2853974668211,38.659617115053,15.));
#29073=CARTESIAN_POINT('Ctrl Pts',(15.2785884727112,38.7600260961351,15.));
#29074=CARTESIAN_POINT('Ctrl Pts',(15.2712072937639,38.860530586589,15.));
#29075=CARTESIAN_POINT('Ctrl Pts',(15.2632589109473,38.9611273555758,15.));
#29076=CARTESIAN_POINT('Ctrl Pts',(15.2547476855825,39.061813415425,15.));
#29077=CARTESIAN_POINT('Ctrl Pts',(15.2456775636447,39.1625859371304,15.));
#29078=CARTESIAN_POINT('Ctrl Pts',(15.2360522089072,39.2634421927888,15.));
#29079=CARTESIAN_POINT('Ctrl Pts',(15.225875156307,39.3643794927167,15.));
#29080=CARTESIAN_POINT('Ctrl Pts',(15.2151499908149,39.4653951093947,15.));
#29081=CARTESIAN_POINT('Ctrl Pts',(15.2038804098649,39.5664862602472,15.));
#29082=CARTESIAN_POINT('Ctrl Pts',(15.1920701163804,39.6676501731673,15.));
#29083=CARTESIAN_POINT('Ctrl Pts',(15.1797227547562,39.7688841338802,15.));
#29084=CARTESIAN_POINT('Ctrl Pts',(15.1668418393198,39.8701855339908,15.));
#29085=CARTESIAN_POINT('Ctrl Pts',(15.1534306754871,39.9715519332134,15.));
#29086=CARTESIAN_POINT('Ctrl Pts',(15.1394923361537,40.0729810652204,15.));
#29087=CARTESIAN_POINT('Ctrl Pts',(15.1250297462408,40.1744707357902,15.));
#29088=CARTESIAN_POINT('Ctrl Pts',(15.1100457495259,40.2760187401822,15.));
#29089=CARTESIAN_POINT('Ctrl Pts',(15.0945431800724,40.3776227809037,15.));
#29090=CARTESIAN_POINT('Ctrl Pts',(15.0785249502524,40.4792803645352,15.));
#29091=CARTESIAN_POINT('Ctrl Pts',(15.0619940893017,40.5809887704301,15.));
#29092=CARTESIAN_POINT('Ctrl Pts',(15.0449536183143,40.6827452453667,15.));
#29093=CARTESIAN_POINT('Ctrl Pts',(15.0274064563211,40.7845471608654,15.));
#29094=CARTESIAN_POINT('Ctrl Pts',(15.0093553188655,40.8863921801,15.));
#29095=CARTESIAN_POINT('Ctrl Pts',(14.9908026205824,40.9882784321884,15.));
#29096=CARTESIAN_POINT('Ctrl Pts',(14.9679399407908,41.1105898934098,15.));
#29097=CARTESIAN_POINT('Ctrl Pts',(14.9482653093396,41.2125650743922,15.));
#29098=CARTESIAN_POINT('Ctrl Pts',(14.9321285285561,41.2941761025922,15.));
#29099=CARTESIAN_POINT('Ctrl Pts',(14.919802810928,41.3554017279611,15.));
#29100=CARTESIAN_POINT('Ctrl Pts',(14.911486495888,41.396226524684,15.));
#29101=CARTESIAN_POINT('Ctrl Pts',(24.725498909423,36.3957374383337,0.));
#29102=CARTESIAN_POINT('Ctrl Pts',(24.725498909423,36.3957374383337,18.));
#29103=CARTESIAN_POINT('Ctrl Pts',(24.7065408286023,36.3871033517098,0.));
#29104=CARTESIAN_POINT('Ctrl Pts',(24.7065408286023,36.3871033517098,18.));
#29105=CARTESIAN_POINT('Ctrl Pts',(24.6686569322616,36.369797330215,0.));
#29106=CARTESIAN_POINT('Ctrl Pts',(24.6686569322616,36.369797330215,18.));
#29107=CARTESIAN_POINT('Ctrl Pts',(24.6119278836614,36.3437247532368,0.));
#29108=CARTESIAN_POINT('Ctrl Pts',(24.6119278836614,36.3437247532368,18.));
#29109=CARTESIAN_POINT('Ctrl Pts',(24.5364828082556,36.3087341522969,0.));
#29110=CARTESIAN_POINT('Ctrl Pts',(24.5364828082556,36.3087341522969,18.));
#29111=CARTESIAN_POINT('Ctrl Pts',(24.4424997853604,36.2646168058395,0.));
#29112=CARTESIAN_POINT('Ctrl Pts',(24.4424997853604,36.2646168058395,18.));
#29113=CARTESIAN_POINT('Ctrl Pts',(24.3488411214068,36.2201196586696,0.));
#29114=CARTESIAN_POINT('Ctrl Pts',(24.3488411214068,36.2201196586696,18.));
#29115=CARTESIAN_POINT('Ctrl Pts',(24.2555084095332,36.1752418704833,0.));
#29116=CARTESIAN_POINT('Ctrl Pts',(24.2555084095332,36.1752418704833,18.));
#29117=CARTESIAN_POINT('Ctrl Pts',(24.1625038657964,36.1299825471271,0.));
#29118=CARTESIAN_POINT('Ctrl Pts',(24.1625038657964,36.1299825471271,18.));
#29119=CARTESIAN_POINT('Ctrl Pts',(24.0698304230588,36.0843408347974,0.));
#29120=CARTESIAN_POINT('Ctrl Pts',(24.0698304230588,36.0843408347974,18.));
#29121=CARTESIAN_POINT('Ctrl Pts',(23.9774915680089,36.0383159101253,0.));
#29122=CARTESIAN_POINT('Ctrl Pts',(23.9774915680089,36.0383159101253,18.));
#29123=CARTESIAN_POINT('Ctrl Pts',(23.8854911428946,35.9919069565469,0.));
#29124=CARTESIAN_POINT('Ctrl Pts',(23.8854911428946,35.9919069565469,18.));
#29125=CARTESIAN_POINT('Ctrl Pts',(23.7938331508737,35.9451131482488,0.));
#29126=CARTESIAN_POINT('Ctrl Pts',(23.7938331508737,35.9451131482488,18.));
#29127=CARTESIAN_POINT('Ctrl Pts',(23.7025215735353,35.8979336336837,0.));
#29128=CARTESIAN_POINT('Ctrl Pts',(23.7025215735353,35.8979336336837,18.));
#29129=CARTESIAN_POINT('Ctrl Pts',(23.611560139948,35.8503675222885,0.));
#29130=CARTESIAN_POINT('Ctrl Pts',(23.611560139948,35.8503675222885,18.));
#29131=CARTESIAN_POINT('Ctrl Pts',(23.5209523746427,35.8024138716897,0.));
#29132=CARTESIAN_POINT('Ctrl Pts',(23.5209523746427,35.8024138716897,18.));
#29133=CARTESIAN_POINT('Ctrl Pts',(23.4307017328227,35.7540716771372,0.));
#29134=CARTESIAN_POINT('Ctrl Pts',(23.4307017328227,35.7540716771372,18.));
#29135=CARTESIAN_POINT('Ctrl Pts',(23.3408117088761,35.7053398620512,0.));
#29136=CARTESIAN_POINT('Ctrl Pts',(23.3408117088761,35.7053398620512,18.));
#29137=CARTESIAN_POINT('Ctrl Pts',(23.2512859425032,35.6562172725207,0.));
#29138=CARTESIAN_POINT('Ctrl Pts',(23.2512859425032,35.6562172725207,18.));
#29139=CARTESIAN_POINT('Ctrl Pts',(23.1621283508111,35.6067026687722,0.));
#29140=CARTESIAN_POINT('Ctrl Pts',(23.1621283508111,35.6067026687722,18.));
#29141=CARTESIAN_POINT('Ctrl Pts',(23.0733431097058,35.5567947408311,0.));
#29142=CARTESIAN_POINT('Ctrl Pts',(23.0733431097058,35.5567947408311,18.));
#29143=CARTESIAN_POINT('Ctrl Pts',(22.9849345572033,35.5064921357308,0.));
#29144=CARTESIAN_POINT('Ctrl Pts',(22.9849345572033,35.5064921357308,18.));
#29145=CARTESIAN_POINT('Ctrl Pts',(22.8969071125089,35.4557934871468,0.));
#29146=CARTESIAN_POINT('Ctrl Pts',(22.8969071125089,35.4557934871468,18.));
#29147=CARTESIAN_POINT('Ctrl Pts',(22.8092652000706,35.4046974393492,0.));
#29148=CARTESIAN_POINT('Ctrl Pts',(22.8092652000706,35.4046974393492,18.));
#29149=CARTESIAN_POINT('Ctrl Pts',(22.7220131336912,35.3532026952313,0.));
#29150=CARTESIAN_POINT('Ctrl Pts',(22.7220131336912,35.3532026952313,18.));
#29151=CARTESIAN_POINT('Ctrl Pts',(22.635155167154,35.3013079759252,0.));
#29152=CARTESIAN_POINT('Ctrl Pts',(22.635155167154,35.3013079759252,18.));
#29153=CARTESIAN_POINT('Ctrl Pts',(22.5486956608909,35.2490119207975,0.));
#29154=CARTESIAN_POINT('Ctrl Pts',(22.5486956608909,35.2490119207975,18.));
#29155=CARTESIAN_POINT('Ctrl Pts',(22.4626392230023,35.1963130003352,0.));
#29156=CARTESIAN_POINT('Ctrl Pts',(22.4626392230023,35.1963130003352,18.));
#29157=CARTESIAN_POINT('Ctrl Pts',(22.3769908340843,35.1432094422642,0.));
#29158=CARTESIAN_POINT('Ctrl Pts',(22.3769908340843,35.1432094422642,18.));
#29159=CARTESIAN_POINT('Ctrl Pts',(22.2917560356803,35.0896991159359,0.));
#29160=CARTESIAN_POINT('Ctrl Pts',(22.2917560356803,35.0896991159359,18.));
#29161=CARTESIAN_POINT('Ctrl Pts',(22.2069408519232,35.0357795922459,0.));
#29162=CARTESIAN_POINT('Ctrl Pts',(22.2069408519232,35.0357795922459,18.));
#29163=CARTESIAN_POINT('Ctrl Pts',(22.1225514798584,34.9814483545602,0.));
#29164=CARTESIAN_POINT('Ctrl Pts',(22.1225514798584,34.9814483545602,18.));
#29165=CARTESIAN_POINT('Ctrl Pts',(22.0385940162683,34.9267029879922,0.));
#29166=CARTESIAN_POINT('Ctrl Pts',(22.0385940162683,34.9267029879922,18.));
#29167=CARTESIAN_POINT('Ctrl Pts',(21.9550742217675,34.8715413418101,0.));
#29168=CARTESIAN_POINT('Ctrl Pts',(21.9550742217675,34.8715413418101,18.));
#29169=CARTESIAN_POINT('Ctrl Pts',(21.8719971302817,34.8159618014436,0.));
#29170=CARTESIAN_POINT('Ctrl Pts',(21.8719971302817,34.8159618014436,18.));
#29171=CARTESIAN_POINT('Ctrl Pts',(21.7893672401137,34.7599631530844,0.));
#29172=CARTESIAN_POINT('Ctrl Pts',(21.7893672401137,34.7599631530844,18.));
#29173=CARTESIAN_POINT('Ctrl Pts',(21.7071892844497,34.7035440429025,0.));
#29174=CARTESIAN_POINT('Ctrl Pts',(21.7071892844497,34.7035440429025,18.));
#29175=CARTESIAN_POINT('Ctrl Pts',(21.6254689009796,34.6467025072367,0.));
#29176=CARTESIAN_POINT('Ctrl Pts',(21.6254689009796,34.6467025072367,18.));
#29177=CARTESIAN_POINT('Ctrl Pts',(21.5442132160757,34.5894355639082,0.));
#29178=CARTESIAN_POINT('Ctrl Pts',(21.5442132160757,34.5894355639082,18.));
#29179=CARTESIAN_POINT('Ctrl Pts',(21.4634317666005,34.5317385658329,0.));
#29180=CARTESIAN_POINT('Ctrl Pts',(21.4634317666005,34.5317385658329,18.));
#29181=CARTESIAN_POINT('Ctrl Pts',(21.3831361300104,34.4736054662052,0.));
#29182=CARTESIAN_POINT('Ctrl Pts',(21.3831361300104,34.4736054662052,18.));
#29183=CARTESIAN_POINT('Ctrl Pts',(21.3033382073239,34.4150300340623,0.));
#29184=CARTESIAN_POINT('Ctrl Pts',(21.3033382073239,34.4150300340623,18.));
#29185=CARTESIAN_POINT('Ctrl Pts',(21.2240487218079,34.3560069185815,0.));
#29186=CARTESIAN_POINT('Ctrl Pts',(21.2240487218079,34.3560069185815,18.));
#29187=CARTESIAN_POINT('Ctrl Pts',(21.1452759244399,34.2965325673384,0.));
#29188=CARTESIAN_POINT('Ctrl Pts',(21.1452759244399,34.2965325673384,18.));
#29189=CARTESIAN_POINT('Ctrl Pts',(21.0670234747355,34.2366067284279,0.));
#29190=CARTESIAN_POINT('Ctrl Pts',(21.0670234747355,34.2366067284279,18.));
#29191=CARTESIAN_POINT('Ctrl Pts',(20.9892914622612,34.176231731809,0.));
#29192=CARTESIAN_POINT('Ctrl Pts',(20.9892914622612,34.176231731809,18.));
#29193=CARTESIAN_POINT('Ctrl Pts',(20.9120805673809,34.1154095510973,0.));
#29194=CARTESIAN_POINT('Ctrl Pts',(20.9120805673809,34.1154095510973,18.));
#29195=CARTESIAN_POINT('Ctrl Pts',(20.8353957068415,34.0541392299678,0.));
#29196=CARTESIAN_POINT('Ctrl Pts',(20.8353957068415,34.0541392299678,18.));
#29197=CARTESIAN_POINT('Ctrl Pts',(20.7592491770603,33.9924146647395,0.));
#29198=CARTESIAN_POINT('Ctrl Pts',(20.7592491770603,33.9924146647395,18.));
#29199=CARTESIAN_POINT('Ctrl Pts',(20.683665762903,33.9302209962425,0.));
#29200=CARTESIAN_POINT('Ctrl Pts',(20.683665762903,33.9302209962425,18.));
#29201=CARTESIAN_POINT('Ctrl Pts',(20.6086800574386,33.8675365150454,0.));
#29202=CARTESIAN_POINT('Ctrl Pts',(20.6086800574386,33.8675365150454,18.));
#29203=CARTESIAN_POINT('Ctrl Pts',(20.5343269914034,33.8043393734971,0.));
#29204=CARTESIAN_POINT('Ctrl Pts',(20.5343269914034,33.8043393734971,18.));
#29205=CARTESIAN_POINT('Ctrl Pts',(20.4606334536183,33.7406135254082,0.));
#29206=CARTESIAN_POINT('Ctrl Pts',(20.4606334536183,33.7406135254082,18.));
#29207=CARTESIAN_POINT('Ctrl Pts',(20.3876111773341,33.6763537716992,0.));
#29208=CARTESIAN_POINT('Ctrl Pts',(20.3876111773341,33.6763537716992,18.));
#29209=CARTESIAN_POINT('Ctrl Pts',(20.3152448035298,33.6115742164079,0.));
#29210=CARTESIAN_POINT('Ctrl Pts',(20.3152448035298,33.6115742164079,18.));
#29211=CARTESIAN_POINT('Ctrl Pts',(20.243500298383,33.5463023319603,0.));
#29212=CARTESIAN_POINT('Ctrl Pts',(20.243500298383,33.5463023319603,18.));
#29213=CARTESIAN_POINT('Ctrl Pts',(20.1723475154533,33.480563024813,0.));
#29214=CARTESIAN_POINT('Ctrl Pts',(20.1723475154533,33.480563024813,18.));
#29215=CARTESIAN_POINT('Ctrl Pts',(20.1017803986381,33.4143643679979,0.));
#29216=CARTESIAN_POINT('Ctrl Pts',(20.1017803986381,33.4143643679979,18.));
#29217=CARTESIAN_POINT('Ctrl Pts',(20.0318342617212,33.3476854048385,0.));
#29218=CARTESIAN_POINT('Ctrl Pts',(20.0318342617212,33.3476854048385,18.));
#29219=CARTESIAN_POINT('Ctrl Pts',(19.9626141625205,33.2804560993213,0.));
#29220=CARTESIAN_POINT('Ctrl Pts',(19.9626141625205,33.2804560993213,18.));
#29221=CARTESIAN_POINT('Ctrl Pts',(19.8942704458546,33.2125746879471,0.));
#29222=CARTESIAN_POINT('Ctrl Pts',(19.8942704458546,33.2125746879471,18.));
#29223=CARTESIAN_POINT('Ctrl Pts',(19.8269479776239,33.1439436707661,0.));
#29224=CARTESIAN_POINT('Ctrl Pts',(19.8269479776239,33.1439436707661,18.));
#29225=CARTESIAN_POINT('Ctrl Pts',(19.7607398248651,33.0745026283418,0.));
#29226=CARTESIAN_POINT('Ctrl Pts',(19.7607398248651,33.0745026283418,18.));
#29227=CARTESIAN_POINT('Ctrl Pts',(19.6956473461873,33.004256563411,0.));
#29228=CARTESIAN_POINT('Ctrl Pts',(19.6956473461873,33.004256563411,18.));
#29229=CARTESIAN_POINT('Ctrl Pts',(19.6315161742485,32.9333211533788,0.));
#29230=CARTESIAN_POINT('Ctrl Pts',(19.6315161742485,32.9333211533788,18.));
#29231=CARTESIAN_POINT('Ctrl Pts',(19.5681157030437,32.8618672807884,0.));
#29232=CARTESIAN_POINT('Ctrl Pts',(19.5681157030437,32.8618672807884,18.));
#29233=CARTESIAN_POINT('Ctrl Pts',(19.5052640847974,32.7900335943248,0.));
#29234=CARTESIAN_POINT('Ctrl Pts',(19.5052640847974,32.7900335943248,18.));
#29235=CARTESIAN_POINT('Ctrl Pts',(19.4429429601189,32.7178463324062,0.));
#29236=CARTESIAN_POINT('Ctrl Pts',(19.4429429601189,32.7178463324062,18.));
#29237=CARTESIAN_POINT('Ctrl Pts',(19.381405831319,32.6451434870609,0.));
#29238=CARTESIAN_POINT('Ctrl Pts',(19.381405831319,32.6451434870609,18.));
#29239=CARTESIAN_POINT('Ctrl Pts',(19.3213180490743,32.5714771007861,0.));
#29240=CARTESIAN_POINT('Ctrl Pts',(19.3213180490743,32.5714771007861,18.));
#29241=CARTESIAN_POINT('Ctrl Pts',(19.2635813403783,32.4962340238036,0.));
#29242=CARTESIAN_POINT('Ctrl Pts',(19.2635813403783,32.4962340238036,18.));
#29243=CARTESIAN_POINT('Ctrl Pts',(19.2200039764927,32.4342791270009,0.));
#29244=CARTESIAN_POINT('Ctrl Pts',(19.2200039764927,32.4342791270009,18.));
#29245=CARTESIAN_POINT('Ctrl Pts',(19.1891139208368,32.3866012518553,0.));
#29246=CARTESIAN_POINT('Ctrl Pts',(19.1891139208368,32.3866012518553,18.));
#29247=CARTESIAN_POINT('Ctrl Pts',(19.1693587749508,32.3542491343753,0.));
#29248=CARTESIAN_POINT('Ctrl Pts',(19.1693587749508,32.3542491343753,18.));
#29249=CARTESIAN_POINT('Ctrl Pts',(19.1596907609891,32.3379313568208,0.));
#29250=CARTESIAN_POINT('Ctrl Pts',(19.1596907609891,32.3379313568208,18.));
#29251=CARTESIAN_POINT('',(24.7254989094229,36.3957374383337,0.));
#29252=CARTESIAN_POINT('Ctrl Pts',(19.1596907609891,32.3379313568208,0.));
#29253=CARTESIAN_POINT('Ctrl Pts',(19.1693587749508,32.3542491343753,0.));
#29254=CARTESIAN_POINT('Ctrl Pts',(19.1891139208368,32.3866012518553,0.));
#29255=CARTESIAN_POINT('Ctrl Pts',(19.2200039764927,32.4342791270009,0.));
#29256=CARTESIAN_POINT('Ctrl Pts',(19.2635813403783,32.4962340238036,0.));
#29257=CARTESIAN_POINT('Ctrl Pts',(19.3213180490743,32.5714771007861,0.));
#29258=CARTESIAN_POINT('Ctrl Pts',(19.381405831319,32.6451434870609,0.));
#29259=CARTESIAN_POINT('Ctrl Pts',(19.4429429601189,32.7178463324062,0.));
#29260=CARTESIAN_POINT('Ctrl Pts',(19.5052640847974,32.7900335943248,0.));
#29261=CARTESIAN_POINT('Ctrl Pts',(19.5681157030437,32.8618672807884,0.));
#29262=CARTESIAN_POINT('Ctrl Pts',(19.6315161742485,32.9333211533788,0.));
#29263=CARTESIAN_POINT('Ctrl Pts',(19.6956473461873,33.004256563411,0.));
#29264=CARTESIAN_POINT('Ctrl Pts',(19.7607398248651,33.0745026283418,0.));
#29265=CARTESIAN_POINT('Ctrl Pts',(19.8269479776239,33.1439436707661,0.));
#29266=CARTESIAN_POINT('Ctrl Pts',(19.8942704458546,33.2125746879471,0.));
#29267=CARTESIAN_POINT('Ctrl Pts',(19.9626141625205,33.2804560993213,0.));
#29268=CARTESIAN_POINT('Ctrl Pts',(20.0318342617212,33.3476854048385,0.));
#29269=CARTESIAN_POINT('Ctrl Pts',(20.1017803986381,33.4143643679979,0.));
#29270=CARTESIAN_POINT('Ctrl Pts',(20.1723475154533,33.480563024813,0.));
#29271=CARTESIAN_POINT('Ctrl Pts',(20.243500298383,33.5463023319603,0.));
#29272=CARTESIAN_POINT('Ctrl Pts',(20.3152448035298,33.6115742164079,0.));
#29273=CARTESIAN_POINT('Ctrl Pts',(20.3876111773341,33.6763537716992,0.));
#29274=CARTESIAN_POINT('Ctrl Pts',(20.4606334536183,33.7406135254082,0.));
#29275=CARTESIAN_POINT('Ctrl Pts',(20.5343269914034,33.8043393734971,0.));
#29276=CARTESIAN_POINT('Ctrl Pts',(20.6086800574386,33.8675365150454,0.));
#29277=CARTESIAN_POINT('Ctrl Pts',(20.683665762903,33.9302209962425,0.));
#29278=CARTESIAN_POINT('Ctrl Pts',(20.7592491770603,33.9924146647395,0.));
#29279=CARTESIAN_POINT('Ctrl Pts',(20.8353957068415,34.0541392299678,0.));
#29280=CARTESIAN_POINT('Ctrl Pts',(20.9120805673809,34.1154095510973,0.));
#29281=CARTESIAN_POINT('Ctrl Pts',(20.9892914622612,34.176231731809,0.));
#29282=CARTESIAN_POINT('Ctrl Pts',(21.0670234747355,34.2366067284279,0.));
#29283=CARTESIAN_POINT('Ctrl Pts',(21.1452759244399,34.2965325673384,0.));
#29284=CARTESIAN_POINT('Ctrl Pts',(21.2240487218079,34.3560069185815,0.));
#29285=CARTESIAN_POINT('Ctrl Pts',(21.3033382073239,34.4150300340623,0.));
#29286=CARTESIAN_POINT('Ctrl Pts',(21.3831361300104,34.4736054662052,0.));
#29287=CARTESIAN_POINT('Ctrl Pts',(21.4634317666005,34.5317385658329,0.));
#29288=CARTESIAN_POINT('Ctrl Pts',(21.5442132160757,34.5894355639082,0.));
#29289=CARTESIAN_POINT('Ctrl Pts',(21.6254689009796,34.6467025072367,0.));
#29290=CARTESIAN_POINT('Ctrl Pts',(21.7071892844497,34.7035440429025,0.));
#29291=CARTESIAN_POINT('Ctrl Pts',(21.7893672401137,34.7599631530844,0.));
#29292=CARTESIAN_POINT('Ctrl Pts',(21.8719971302817,34.8159618014436,0.));
#29293=CARTESIAN_POINT('Ctrl Pts',(21.9550742217675,34.8715413418101,0.));
#29294=CARTESIAN_POINT('Ctrl Pts',(22.0385940162683,34.9267029879922,0.));
#29295=CARTESIAN_POINT('Ctrl Pts',(22.1225514798584,34.9814483545602,0.));
#29296=CARTESIAN_POINT('Ctrl Pts',(22.2069408519232,35.0357795922459,0.));
#29297=CARTESIAN_POINT('Ctrl Pts',(22.2917560356803,35.0896991159359,0.));
#29298=CARTESIAN_POINT('Ctrl Pts',(22.3769908340843,35.1432094422642,0.));
#29299=CARTESIAN_POINT('Ctrl Pts',(22.4626392230023,35.1963130003352,0.));
#29300=CARTESIAN_POINT('Ctrl Pts',(22.5486956608909,35.2490119207975,0.));
#29301=CARTESIAN_POINT('Ctrl Pts',(22.635155167154,35.3013079759252,0.));
#29302=CARTESIAN_POINT('Ctrl Pts',(22.7220131336912,35.3532026952313,0.));
#29303=CARTESIAN_POINT('Ctrl Pts',(22.8092652000706,35.4046974393492,0.));
#29304=CARTESIAN_POINT('Ctrl Pts',(22.8969071125089,35.4557934871468,0.));
#29305=CARTESIAN_POINT('Ctrl Pts',(22.9849345572033,35.5064921357308,0.));
#29306=CARTESIAN_POINT('Ctrl Pts',(23.0733431097058,35.5567947408311,0.));
#29307=CARTESIAN_POINT('Ctrl Pts',(23.1621283508111,35.6067026687722,0.));
#29308=CARTESIAN_POINT('Ctrl Pts',(23.2512859425032,35.6562172725207,0.));
#29309=CARTESIAN_POINT('Ctrl Pts',(23.3408117088761,35.7053398620512,0.));
#29310=CARTESIAN_POINT('Ctrl Pts',(23.4307017328227,35.7540716771372,0.));
#29311=CARTESIAN_POINT('Ctrl Pts',(23.5209523746427,35.8024138716897,0.));
#29312=CARTESIAN_POINT('Ctrl Pts',(23.611560139948,35.8503675222885,0.));
#29313=CARTESIAN_POINT('Ctrl Pts',(23.7025215735353,35.8979336336837,0.));
#29314=CARTESIAN_POINT('Ctrl Pts',(23.7938331508737,35.9451131482488,0.));
#29315=CARTESIAN_POINT('Ctrl Pts',(23.8854911428946,35.9919069565469,0.));
#29316=CARTESIAN_POINT('Ctrl Pts',(23.9774915680089,36.0383159101253,0.));
#29317=CARTESIAN_POINT('Ctrl Pts',(24.0698304230588,36.0843408347974,0.));
#29318=CARTESIAN_POINT('Ctrl Pts',(24.1625038657964,36.1299825471271,0.));
#29319=CARTESIAN_POINT('Ctrl Pts',(24.2555084095332,36.1752418704833,0.));
#29320=CARTESIAN_POINT('Ctrl Pts',(24.3488411214068,36.2201196586696,0.));
#29321=CARTESIAN_POINT('Ctrl Pts',(24.4612315181511,36.2735162352735,0.));
#29322=CARTESIAN_POINT('Ctrl Pts',(24.5552956307817,36.3175386315528,0.));
#29323=CARTESIAN_POINT('Ctrl Pts',(24.630805301288,36.3524534604648,0.));
#29324=CARTESIAN_POINT('Ctrl Pts',(24.6875827477484,36.3784692650901,0.));
#29325=CARTESIAN_POINT('Ctrl Pts',(24.725498909423,36.3957374383337,0.));
#29326=CARTESIAN_POINT('',(24.7254989094229,36.3957374383337,15.));
#29327=CARTESIAN_POINT('Ctrl Pts',(24.725498909423,36.3957374383337,15.));
#29328=CARTESIAN_POINT('Ctrl Pts',(24.7065408286023,36.3871033517098,15.));
#29329=CARTESIAN_POINT('Ctrl Pts',(24.6686569322616,36.369797330215,15.));
#29330=CARTESIAN_POINT('Ctrl Pts',(24.6119278836614,36.3437247532368,15.));
#29331=CARTESIAN_POINT('Ctrl Pts',(24.5364828082556,36.3087341522969,15.));
#29332=CARTESIAN_POINT('Ctrl Pts',(24.4424997853604,36.2646168058395,15.));
#29333=CARTESIAN_POINT('Ctrl Pts',(24.3488411214068,36.2201196586696,15.));
#29334=CARTESIAN_POINT('Ctrl Pts',(24.2555084095332,36.1752418704833,15.));
#29335=CARTESIAN_POINT('Ctrl Pts',(24.1625038657964,36.1299825471271,15.));
#29336=CARTESIAN_POINT('Ctrl Pts',(24.0698304230588,36.0843408347974,15.));
#29337=CARTESIAN_POINT('Ctrl Pts',(23.9774915680089,36.0383159101253,15.));
#29338=CARTESIAN_POINT('Ctrl Pts',(23.8854911428946,35.9919069565469,15.));
#29339=CARTESIAN_POINT('Ctrl Pts',(23.7938331508737,35.9451131482488,15.));
#29340=CARTESIAN_POINT('Ctrl Pts',(23.7025215735353,35.8979336336837,15.));
#29341=CARTESIAN_POINT('Ctrl Pts',(23.611560139948,35.8503675222885,15.));
#29342=CARTESIAN_POINT('Ctrl Pts',(23.5209523746427,35.8024138716897,15.));
#29343=CARTESIAN_POINT('Ctrl Pts',(23.4307017328227,35.7540716771372,15.));
#29344=CARTESIAN_POINT('Ctrl Pts',(23.3408117088761,35.7053398620512,15.));
#29345=CARTESIAN_POINT('Ctrl Pts',(23.2512859425032,35.6562172725207,15.));
#29346=CARTESIAN_POINT('Ctrl Pts',(23.1621283508111,35.6067026687722,15.));
#29347=CARTESIAN_POINT('Ctrl Pts',(23.0733431097058,35.5567947408311,15.));
#29348=CARTESIAN_POINT('Ctrl Pts',(22.9849345572033,35.5064921357308,15.));
#29349=CARTESIAN_POINT('Ctrl Pts',(22.8969071125089,35.4557934871468,15.));
#29350=CARTESIAN_POINT('Ctrl Pts',(22.8092652000706,35.4046974393492,15.));
#29351=CARTESIAN_POINT('Ctrl Pts',(22.7220131336912,35.3532026952313,15.));
#29352=CARTESIAN_POINT('Ctrl Pts',(22.635155167154,35.3013079759252,15.));
#29353=CARTESIAN_POINT('Ctrl Pts',(22.5486956608909,35.2490119207975,15.));
#29354=CARTESIAN_POINT('Ctrl Pts',(22.4626392230023,35.1963130003352,15.));
#29355=CARTESIAN_POINT('Ctrl Pts',(22.3769908340843,35.1432094422642,15.));
#29356=CARTESIAN_POINT('Ctrl Pts',(22.2917560356803,35.0896991159359,15.));
#29357=CARTESIAN_POINT('Ctrl Pts',(22.2069408519232,35.0357795922459,15.));
#29358=CARTESIAN_POINT('Ctrl Pts',(22.1225514798584,34.9814483545602,15.));
#29359=CARTESIAN_POINT('Ctrl Pts',(22.0385940162683,34.9267029879922,15.));
#29360=CARTESIAN_POINT('Ctrl Pts',(21.9550742217675,34.8715413418101,15.));
#29361=CARTESIAN_POINT('Ctrl Pts',(21.8719971302817,34.8159618014436,15.));
#29362=CARTESIAN_POINT('Ctrl Pts',(21.7893672401137,34.7599631530844,15.));
#29363=CARTESIAN_POINT('Ctrl Pts',(21.7071892844497,34.7035440429025,15.));
#29364=CARTESIAN_POINT('Ctrl Pts',(21.6254689009796,34.6467025072367,15.));
#29365=CARTESIAN_POINT('Ctrl Pts',(21.5442132160757,34.5894355639082,15.));
#29366=CARTESIAN_POINT('Ctrl Pts',(21.4634317666005,34.5317385658329,15.));
#29367=CARTESIAN_POINT('Ctrl Pts',(21.3831361300104,34.4736054662052,15.));
#29368=CARTESIAN_POINT('Ctrl Pts',(21.3033382073239,34.4150300340623,15.));
#29369=CARTESIAN_POINT('Ctrl Pts',(21.2240487218079,34.3560069185815,15.));
#29370=CARTESIAN_POINT('Ctrl Pts',(21.1452759244399,34.2965325673384,15.));
#29371=CARTESIAN_POINT('Ctrl Pts',(21.0670234747355,34.2366067284279,15.));
#29372=CARTESIAN_POINT('Ctrl Pts',(20.9892914622612,34.176231731809,15.));
#29373=CARTESIAN_POINT('Ctrl Pts',(20.9120805673809,34.1154095510973,15.));
#29374=CARTESIAN_POINT('Ctrl Pts',(20.8353957068415,34.0541392299678,15.));
#29375=CARTESIAN_POINT('Ctrl Pts',(20.7592491770603,33.9924146647395,15.));
#29376=CARTESIAN_POINT('Ctrl Pts',(20.683665762903,33.9302209962425,15.));
#29377=CARTESIAN_POINT('Ctrl Pts',(20.6086800574386,33.8675365150454,15.));
#29378=CARTESIAN_POINT('Ctrl Pts',(20.5343269914034,33.8043393734971,15.));
#29379=CARTESIAN_POINT('Ctrl Pts',(20.4606334536183,33.7406135254082,15.));
#29380=CARTESIAN_POINT('Ctrl Pts',(20.3876111773341,33.6763537716992,15.));
#29381=CARTESIAN_POINT('Ctrl Pts',(20.3152448035298,33.6115742164079,15.));
#29382=CARTESIAN_POINT('Ctrl Pts',(20.243500298383,33.5463023319603,15.));
#29383=CARTESIAN_POINT('Ctrl Pts',(20.1723475154533,33.480563024813,15.));
#29384=CARTESIAN_POINT('Ctrl Pts',(20.1017803986381,33.4143643679979,15.));
#29385=CARTESIAN_POINT('Ctrl Pts',(20.0318342617212,33.3476854048385,15.));
#29386=CARTESIAN_POINT('Ctrl Pts',(19.9626141625205,33.2804560993213,15.));
#29387=CARTESIAN_POINT('Ctrl Pts',(19.8942704458546,33.2125746879471,15.));
#29388=CARTESIAN_POINT('Ctrl Pts',(19.8269479776239,33.1439436707661,15.));
#29389=CARTESIAN_POINT('Ctrl Pts',(19.7607398248651,33.0745026283418,15.));
#29390=CARTESIAN_POINT('Ctrl Pts',(19.6956473461873,33.004256563411,15.));
#29391=CARTESIAN_POINT('Ctrl Pts',(19.6315161742485,32.9333211533788,15.));
#29392=CARTESIAN_POINT('Ctrl Pts',(19.5681157030437,32.8618672807884,15.));
#29393=CARTESIAN_POINT('Ctrl Pts',(19.5052640847974,32.7900335943248,15.));
#29394=CARTESIAN_POINT('Ctrl Pts',(19.4429429601189,32.7178463324062,15.));
#29395=CARTESIAN_POINT('Ctrl Pts',(19.381405831319,32.6451434870609,15.));
#29396=CARTESIAN_POINT('Ctrl Pts',(19.3213180490743,32.5714771007861,15.));
#29397=CARTESIAN_POINT('Ctrl Pts',(19.2635813403783,32.4962340238036,15.));
#29398=CARTESIAN_POINT('Ctrl Pts',(19.2200039764927,32.4342791270009,15.));
#29399=CARTESIAN_POINT('Ctrl Pts',(19.1891139208368,32.3866012518553,15.));
#29400=CARTESIAN_POINT('Ctrl Pts',(19.1693587749508,32.3542491343753,15.));
#29401=CARTESIAN_POINT('Ctrl Pts',(19.1596907609891,32.3379313568208,15.));
#29402=CARTESIAN_POINT('',(24.7254989094229,36.3957374383337,0.));
#29403=CARTESIAN_POINT('Origin',(6.66146233219319E-12,9.16871631793044E-12,
0.));
#29404=CARTESIAN_POINT('',(26.9738038986838,34.762248247709,0.));
#29405=CARTESIAN_POINT('Origin',(6.66146233219319E-12,9.16871631793044E-12,
0.));
#29406=CARTESIAN_POINT('',(26.9738038986838,34.762248247709,15.));
#29407=CARTESIAN_POINT('Origin',(6.66146233219319E-12,9.16871631793044E-12,
15.));
#29408=CARTESIAN_POINT('',(26.9738038986838,34.762248247709,0.));
#29409=CARTESIAN_POINT('Ctrl Pts',(24.8345302882955,28.2149191006268,0.));
#29410=CARTESIAN_POINT('Ctrl Pts',(24.8345302882955,28.2149191006268,18.));
#29411=CARTESIAN_POINT('Ctrl Pts',(24.8470618363541,28.2291563988796,0.));
#29412=CARTESIAN_POINT('Ctrl Pts',(24.8470618363541,28.2291563988796,18.));
#29413=CARTESIAN_POINT('Ctrl Pts',(24.8717258526943,28.2579420132101,0.));
#29414=CARTESIAN_POINT('Ctrl Pts',(24.8717258526943,28.2579420132101,18.));
#29415=CARTESIAN_POINT('Ctrl Pts',(24.9075246543798,28.3020534756061,0.));
#29416=CARTESIAN_POINT('Ctrl Pts',(24.9075246543798,28.3020534756061,18.));
#29417=CARTESIAN_POINT('Ctrl Pts',(24.9529811166897,28.3626431274892,0.));
#29418=CARTESIAN_POINT('Ctrl Pts',(24.9529811166897,28.3626431274892,18.));
#29419=CARTESIAN_POINT('Ctrl Pts',(25.0066999111736,28.4408053900206,0.));
#29420=CARTESIAN_POINT('Ctrl Pts',(25.0066999111736,28.4408053900206,18.));
#29421=CARTESIAN_POINT('Ctrl Pts',(25.0581926620043,28.5207164321473,0.));
#29422=CARTESIAN_POINT('Ctrl Pts',(25.0581926620043,28.5207164321473,18.));
#29423=CARTESIAN_POINT('Ctrl Pts',(25.1083211582389,28.6017081342376,0.));
#29424=CARTESIAN_POINT('Ctrl Pts',(25.1083211582389,28.6017081342376,18.));
#29425=CARTESIAN_POINT('Ctrl Pts',(25.1577170374459,28.6832861366762,0.));
#29426=CARTESIAN_POINT('Ctrl Pts',(25.1577170374459,28.6832861366762,18.));
#29427=CARTESIAN_POINT('Ctrl Pts',(25.2066127148845,28.7652594076549,0.));
#29428=CARTESIAN_POINT('Ctrl Pts',(25.2066127148845,28.7652594076549,18.));
#29429=CARTESIAN_POINT('Ctrl Pts',(25.2549775629725,28.8476372998748,0.));
#29430=CARTESIAN_POINT('Ctrl Pts',(25.2549775629725,28.8476372998748,18.));
#29431=CARTESIAN_POINT('Ctrl Pts',(25.3026235249214,28.9305499160476,0.));
#29432=CARTESIAN_POINT('Ctrl Pts',(25.3026235249214,28.9305499160476,18.));
#29433=CARTESIAN_POINT('Ctrl Pts',(25.3493168206005,29.0141637699076,0.));
#29434=CARTESIAN_POINT('Ctrl Pts',(25.3493168206005,29.0141637699076,18.));
#29435=CARTESIAN_POINT('Ctrl Pts',(25.3948997321279,29.098589927237,0.));
#29436=CARTESIAN_POINT('Ctrl Pts',(25.3948997321279,29.098589927237,18.));
#29437=CARTESIAN_POINT('Ctrl Pts',(25.4393679214513,29.183825549991,0.));
#29438=CARTESIAN_POINT('Ctrl Pts',(25.4393679214513,29.183825549991,18.));
#29439=CARTESIAN_POINT('Ctrl Pts',(25.4828076101654,29.2698007967907,0.));
#29440=CARTESIAN_POINT('Ctrl Pts',(25.4828076101654,29.2698007967907,18.));
#29441=CARTESIAN_POINT('Ctrl Pts',(25.5253562922582,29.356408021119,0.));
#29442=CARTESIAN_POINT('Ctrl Pts',(25.5253562922582,29.356408021119,18.));
#29443=CARTESIAN_POINT('Ctrl Pts',(25.5671572096726,29.443535683207,0.));
#29444=CARTESIAN_POINT('Ctrl Pts',(25.5671572096726,29.443535683207,18.));
#29445=CARTESIAN_POINT('Ctrl Pts',(25.6083094352667,29.5311055094509,0.));
#29446=CARTESIAN_POINT('Ctrl Pts',(25.6083094352667,29.5311055094509,18.));
#29447=CARTESIAN_POINT('Ctrl Pts',(25.6488438125835,29.6190903904157,0.));
#29448=CARTESIAN_POINT('Ctrl Pts',(25.6488438125835,29.6190903904157,18.));
#29449=CARTESIAN_POINT('Ctrl Pts',(25.6887507922748,29.7074935910931,0.));
#29450=CARTESIAN_POINT('Ctrl Pts',(25.6887507922748,29.7074935910931,18.));
#29451=CARTESIAN_POINT('Ctrl Pts',(25.7279973711305,29.7963360859334,0.));
#29452=CARTESIAN_POINT('Ctrl Pts',(25.7279973711305,29.7963360859334,18.));
#29453=CARTESIAN_POINT('Ctrl Pts',(25.7665469042913,29.8856417535786,0.));
#29454=CARTESIAN_POINT('Ctrl Pts',(25.7665469042913,29.8856417535786,18.));
#29455=CARTESIAN_POINT('Ctrl Pts',(25.8043812318214,29.9754208429384,0.));
#29456=CARTESIAN_POINT('Ctrl Pts',(25.8043812318214,29.9754208429384,18.));
#29457=CARTESIAN_POINT('Ctrl Pts',(25.8415089241134,30.0656638016321,0.));
#29458=CARTESIAN_POINT('Ctrl Pts',(25.8415089241134,30.0656638016321,18.));
#29459=CARTESIAN_POINT('Ctrl Pts',(25.8779535511027,30.1563500154165,0.));
#29460=CARTESIAN_POINT('Ctrl Pts',(25.8779535511027,30.1563500154165,18.));
#29461=CARTESIAN_POINT('Ctrl Pts',(25.9137466853317,30.2474530144827,0.));
#29462=CARTESIAN_POINT('Ctrl Pts',(25.9137466853317,30.2474530144827,18.));
#29463=CARTESIAN_POINT('Ctrl Pts',(25.9489196635424,30.3389466074503,0.));
#29464=CARTESIAN_POINT('Ctrl Pts',(25.9489196635424,30.3389466074503,18.));
#29465=CARTESIAN_POINT('Ctrl Pts',(25.9834942765902,30.4308118142473,0.));
#29466=CARTESIAN_POINT('Ctrl Pts',(25.9834942765902,30.4308118142473,18.));
#29467=CARTESIAN_POINT('Ctrl Pts',(26.0174801292225,30.5230388264271,0.));
#29468=CARTESIAN_POINT('Ctrl Pts',(26.0174801292225,30.5230388264271,18.));
#29469=CARTESIAN_POINT('Ctrl Pts',(26.0508796503166,30.6156232634061,0.));
#29470=CARTESIAN_POINT('Ctrl Pts',(26.0508796503166,30.6156232634061,18.));
#29471=CARTESIAN_POINT('Ctrl Pts',(26.0836911730968,30.7085638682391,0.));
#29472=CARTESIAN_POINT('Ctrl Pts',(26.0836911730968,30.7085638682391,18.));
#29473=CARTESIAN_POINT('Ctrl Pts',(26.1159125093178,30.8018598357461,0.));
#29474=CARTESIAN_POINT('Ctrl Pts',(26.1159125093178,30.8018598357461,18.));
#29475=CARTESIAN_POINT('Ctrl Pts',(26.1475450294082,30.8955077633644,0.));
#29476=CARTESIAN_POINT('Ctrl Pts',(26.1475450294082,30.8955077633644,18.));
#29477=CARTESIAN_POINT('Ctrl Pts',(26.1785946616165,30.9895009017073,0.));
#29478=CARTESIAN_POINT('Ctrl Pts',(26.1785946616165,30.9895009017073,18.));
#29479=CARTESIAN_POINT('Ctrl Pts',(26.2090698085494,31.0838307058369,0.));
#29480=CARTESIAN_POINT('Ctrl Pts',(26.2090698085494,31.0838307058369,18.));
#29481=CARTESIAN_POINT('Ctrl Pts',(26.2389800738215,31.1784877826858,0.));
#29482=CARTESIAN_POINT('Ctrl Pts',(26.2389800738215,31.1784877826858,18.));
#29483=CARTESIAN_POINT('Ctrl Pts',(26.2683347859175,31.2734629900041,0.));
#29484=CARTESIAN_POINT('Ctrl Pts',(26.2683347859175,31.2734629900041,18.));
#29485=CARTESIAN_POINT('Ctrl Pts',(26.2971413115295,31.3687486937246,0.));
#29486=CARTESIAN_POINT('Ctrl Pts',(26.2971413115295,31.3687486937246,18.));
#29487=CARTESIAN_POINT('Ctrl Pts',(26.3254046890485,31.4643390378084,0.));
#29488=CARTESIAN_POINT('Ctrl Pts',(26.3254046890485,31.4643390378084,18.));
#29489=CARTESIAN_POINT('Ctrl Pts',(26.353128528169,31.5602292672984,0.));
#29490=CARTESIAN_POINT('Ctrl Pts',(26.353128528169,31.5602292672984,18.));
#29491=CARTESIAN_POINT('Ctrl Pts',(26.3803155790949,31.6564152990236,0.));
#29492=CARTESIAN_POINT('Ctrl Pts',(26.3803155790949,31.6564152990236,18.));
#29493=CARTESIAN_POINT('Ctrl Pts',(26.4069683862784,31.7528932299312,0.));
#29494=CARTESIAN_POINT('Ctrl Pts',(26.4069683862784,31.7528932299312,18.));
#29495=CARTESIAN_POINT('Ctrl Pts',(26.433090040836,31.849658771403,0.));
#29496=CARTESIAN_POINT('Ctrl Pts',(26.433090040836,31.849658771403,18.));
#29497=CARTESIAN_POINT('Ctrl Pts',(26.4586843683627,31.9467071093816,0.));
#29498=CARTESIAN_POINT('Ctrl Pts',(26.4586843683627,31.9467071093816,18.));
#29499=CARTESIAN_POINT('Ctrl Pts',(26.4837555495616,32.0440331917233,0.));
#29500=CARTESIAN_POINT('Ctrl Pts',(26.4837555495616,32.0440331917233,18.));
#29501=CARTESIAN_POINT('Ctrl Pts',(26.5083078928862,32.1416319023705,0.));
#29502=CARTESIAN_POINT('Ctrl Pts',(26.5083078928862,32.1416319023705,18.));
#29503=CARTESIAN_POINT('Ctrl Pts',(26.5323455701117,32.2394982626669,0.));
#29504=CARTESIAN_POINT('Ctrl Pts',(26.5323455701117,32.2394982626669,18.));
#29505=CARTESIAN_POINT('Ctrl Pts',(26.5558723200361,32.3376276606981,0.));
#29506=CARTESIAN_POINT('Ctrl Pts',(26.5558723200361,32.3376276606981,18.));
#29507=CARTESIAN_POINT('Ctrl Pts',(26.5788913672813,32.4360159072985,0.));
#29508=CARTESIAN_POINT('Ctrl Pts',(26.5788913672813,32.4360159072985,18.));
#29509=CARTESIAN_POINT('Ctrl Pts',(26.6014055904817,32.5346590925498,0.));
#29510=CARTESIAN_POINT('Ctrl Pts',(26.6014055904817,32.5346590925498,18.));
#29511=CARTESIAN_POINT('Ctrl Pts',(26.6234176311245,32.6335534898935,0.));
#29512=CARTESIAN_POINT('Ctrl Pts',(26.6234176311245,32.6335534898935,18.));
#29513=CARTESIAN_POINT('Ctrl Pts',(26.6449300199763,32.7326954489334,0.));
#29514=CARTESIAN_POINT('Ctrl Pts',(26.6449300199763,32.7326954489334,18.));
#29515=CARTESIAN_POINT('Ctrl Pts',(26.6659453236976,32.8320812678271,0.));
#29516=CARTESIAN_POINT('Ctrl Pts',(26.6659453236976,32.8320812678271,18.));
#29517=CARTESIAN_POINT('Ctrl Pts',(26.6864661988935,32.9317071576181,0.));
#29518=CARTESIAN_POINT('Ctrl Pts',(26.6864661988935,32.9317071576181,18.));
#29519=CARTESIAN_POINT('Ctrl Pts',(26.7064953106254,33.03156933761,0.));
#29520=CARTESIAN_POINT('Ctrl Pts',(26.7064953106254,33.03156933761,18.));
#29521=CARTESIAN_POINT('Ctrl Pts',(26.7260352861619,33.131664100194,0.));
#29522=CARTESIAN_POINT('Ctrl Pts',(26.7260352861619,33.131664100194,18.));
#29523=CARTESIAN_POINT('Ctrl Pts',(26.7450886617884,33.2319878786519,0.));
#29524=CARTESIAN_POINT('Ctrl Pts',(26.7450886617884,33.2319878786519,18.));
#29525=CARTESIAN_POINT('Ctrl Pts',(26.7636578270526,33.3325373307046,0.));
#29526=CARTESIAN_POINT('Ctrl Pts',(26.7636578270526,33.3325373307046,18.));
#29527=CARTESIAN_POINT('Ctrl Pts',(26.7817450041181,33.4333093513694,0.));
#29528=CARTESIAN_POINT('Ctrl Pts',(26.7817450041181,33.4333093513694,18.));
#29529=CARTESIAN_POINT('Ctrl Pts',(26.7993522966985,33.5343009499673,0.));
#29530=CARTESIAN_POINT('Ctrl Pts',(26.7993522966985,33.5343009499673,18.));
#29531=CARTESIAN_POINT('Ctrl Pts',(26.8164817280846,33.6355091508895,0.));
#29532=CARTESIAN_POINT('Ctrl Pts',(26.8164817280846,33.6355091508895,18.));
#29533=CARTESIAN_POINT('Ctrl Pts',(26.8331352836667,33.7369308933173,0.));
#29534=CARTESIAN_POINT('Ctrl Pts',(26.8331352836667,33.7369308933173,18.));
#29535=CARTESIAN_POINT('Ctrl Pts',(26.8493149627661,33.838562905895,0.));
#29536=CARTESIAN_POINT('Ctrl Pts',(26.8493149627661,33.838562905895,18.));
#29537=CARTESIAN_POINT('Ctrl Pts',(26.8650228056313,33.9404016650487,0.));
#29538=CARTESIAN_POINT('Ctrl Pts',(26.8650228056313,33.9404016650487,18.));
#29539=CARTESIAN_POINT('Ctrl Pts',(26.880260834701,34.0424436187397,0.));
#29540=CARTESIAN_POINT('Ctrl Pts',(26.880260834701,34.0424436187397,18.));
#29541=CARTESIAN_POINT('Ctrl Pts',(26.8950310138939,34.1446853651051,0.));
#29542=CARTESIAN_POINT('Ctrl Pts',(26.8950310138939,34.1446853651051,18.));
#29543=CARTESIAN_POINT('Ctrl Pts',(26.9093352037262,34.2471238425419,0.));
#29544=CARTESIAN_POINT('Ctrl Pts',(26.9093352037262,34.2471238425419,18.));
#29545=CARTESIAN_POINT('Ctrl Pts',(26.9231751225177,34.3497565255724,0.));
#29546=CARTESIAN_POINT('Ctrl Pts',(26.9231751225177,34.3497565255724,18.));
#29547=CARTESIAN_POINT('Ctrl Pts',(26.9365523054581,34.4525815829097,0.));
#29548=CARTESIAN_POINT('Ctrl Pts',(26.9365523054581,34.4525815829097,18.));
#29549=CARTESIAN_POINT('Ctrl Pts',(26.9494680440307,34.5555977590573,0.));
#29550=CARTESIAN_POINT('Ctrl Pts',(26.9494680440307,34.5555977590573,18.));
#29551=CARTESIAN_POINT('Ctrl Pts',(26.9594322726214,34.6381629799782,0.));
#29552=CARTESIAN_POINT('Ctrl Pts',(26.9594322726214,34.6381629799782,18.));
#29553=CARTESIAN_POINT('Ctrl Pts',(26.9666985267608,34.700172380686,0.));
#29554=CARTESIAN_POINT('Ctrl Pts',(26.9666985267608,34.700172380686,18.));
#29555=CARTESIAN_POINT('Ctrl Pts',(26.9714507634923,34.7415499619104,0.));
#29556=CARTESIAN_POINT('Ctrl Pts',(26.9714507634923,34.7415499619104,18.));
#29557=CARTESIAN_POINT('Ctrl Pts',(26.9738038986838,34.7622482477091,0.));
#29558=CARTESIAN_POINT('Ctrl Pts',(26.9738038986838,34.7622482477091,18.));
#29559=CARTESIAN_POINT('Ctrl Pts',(24.8345302882955,28.2149191006268,0.));
#29560=CARTESIAN_POINT('Ctrl Pts',(24.8470618363541,28.2291563988796,0.));
#29561=CARTESIAN_POINT('Ctrl Pts',(24.8717258526943,28.2579420132101,0.));
#29562=CARTESIAN_POINT('Ctrl Pts',(24.9075246543798,28.3020534756061,0.));
#29563=CARTESIAN_POINT('Ctrl Pts',(24.9529811166897,28.3626431274892,0.));
#29564=CARTESIAN_POINT('Ctrl Pts',(25.0066999111736,28.4408053900206,0.));
#29565=CARTESIAN_POINT('Ctrl Pts',(25.0581926620043,28.5207164321473,0.));
#29566=CARTESIAN_POINT('Ctrl Pts',(25.1083211582389,28.6017081342376,0.));
#29567=CARTESIAN_POINT('Ctrl Pts',(25.1577170374459,28.6832861366762,0.));
#29568=CARTESIAN_POINT('Ctrl Pts',(25.2066127148845,28.7652594076549,0.));
#29569=CARTESIAN_POINT('Ctrl Pts',(25.2549775629725,28.8476372998748,0.));
#29570=CARTESIAN_POINT('Ctrl Pts',(25.3026235249214,28.9305499160476,0.));
#29571=CARTESIAN_POINT('Ctrl Pts',(25.3493168206005,29.0141637699076,0.));
#29572=CARTESIAN_POINT('Ctrl Pts',(25.3948997321279,29.098589927237,0.));
#29573=CARTESIAN_POINT('Ctrl Pts',(25.4393679214513,29.183825549991,0.));
#29574=CARTESIAN_POINT('Ctrl Pts',(25.4828076101654,29.2698007967907,0.));
#29575=CARTESIAN_POINT('Ctrl Pts',(25.5253562922582,29.356408021119,0.));
#29576=CARTESIAN_POINT('Ctrl Pts',(25.5671572096726,29.443535683207,0.));
#29577=CARTESIAN_POINT('Ctrl Pts',(25.6083094352667,29.5311055094509,0.));
#29578=CARTESIAN_POINT('Ctrl Pts',(25.6488438125835,29.6190903904157,0.));
#29579=CARTESIAN_POINT('Ctrl Pts',(25.6887507922748,29.7074935910931,0.));
#29580=CARTESIAN_POINT('Ctrl Pts',(25.7279973711305,29.7963360859334,0.));
#29581=CARTESIAN_POINT('Ctrl Pts',(25.7665469042913,29.8856417535786,0.));
#29582=CARTESIAN_POINT('Ctrl Pts',(25.8043812318214,29.9754208429384,0.));
#29583=CARTESIAN_POINT('Ctrl Pts',(25.8415089241134,30.0656638016321,0.));
#29584=CARTESIAN_POINT('Ctrl Pts',(25.8779535511027,30.1563500154165,0.));
#29585=CARTESIAN_POINT('Ctrl Pts',(25.9137466853317,30.2474530144827,0.));
#29586=CARTESIAN_POINT('Ctrl Pts',(25.9489196635424,30.3389466074503,0.));
#29587=CARTESIAN_POINT('Ctrl Pts',(25.9834942765902,30.4308118142473,0.));
#29588=CARTESIAN_POINT('Ctrl Pts',(26.0174801292225,30.5230388264271,0.));
#29589=CARTESIAN_POINT('Ctrl Pts',(26.0508796503166,30.6156232634061,0.));
#29590=CARTESIAN_POINT('Ctrl Pts',(26.0836911730968,30.7085638682391,0.));
#29591=CARTESIAN_POINT('Ctrl Pts',(26.1159125093178,30.8018598357461,0.));
#29592=CARTESIAN_POINT('Ctrl Pts',(26.1475450294082,30.8955077633644,0.));
#29593=CARTESIAN_POINT('Ctrl Pts',(26.1785946616165,30.9895009017073,0.));
#29594=CARTESIAN_POINT('Ctrl Pts',(26.2090698085494,31.0838307058369,0.));
#29595=CARTESIAN_POINT('Ctrl Pts',(26.2389800738215,31.1784877826858,0.));
#29596=CARTESIAN_POINT('Ctrl Pts',(26.2683347859175,31.2734629900041,0.));
#29597=CARTESIAN_POINT('Ctrl Pts',(26.2971413115295,31.3687486937246,0.));
#29598=CARTESIAN_POINT('Ctrl Pts',(26.3254046890485,31.4643390378084,0.));
#29599=CARTESIAN_POINT('Ctrl Pts',(26.353128528169,31.5602292672984,0.));
#29600=CARTESIAN_POINT('Ctrl Pts',(26.3803155790949,31.6564152990236,0.));
#29601=CARTESIAN_POINT('Ctrl Pts',(26.4069683862784,31.7528932299312,0.));
#29602=CARTESIAN_POINT('Ctrl Pts',(26.433090040836,31.849658771403,0.));
#29603=CARTESIAN_POINT('Ctrl Pts',(26.4586843683627,31.9467071093816,0.));
#29604=CARTESIAN_POINT('Ctrl Pts',(26.4837555495616,32.0440331917233,0.));
#29605=CARTESIAN_POINT('Ctrl Pts',(26.5083078928862,32.1416319023705,0.));
#29606=CARTESIAN_POINT('Ctrl Pts',(26.5323455701117,32.2394982626669,0.));
#29607=CARTESIAN_POINT('Ctrl Pts',(26.5558723200361,32.3376276606981,0.));
#29608=CARTESIAN_POINT('Ctrl Pts',(26.5788913672813,32.4360159072985,0.));
#29609=CARTESIAN_POINT('Ctrl Pts',(26.6014055904817,32.5346590925498,0.));
#29610=CARTESIAN_POINT('Ctrl Pts',(26.6234176311245,32.6335534898935,0.));
#29611=CARTESIAN_POINT('Ctrl Pts',(26.6449300199763,32.7326954489334,0.));
#29612=CARTESIAN_POINT('Ctrl Pts',(26.6659453236976,32.8320812678271,0.));
#29613=CARTESIAN_POINT('Ctrl Pts',(26.6864661988935,32.9317071576181,0.));
#29614=CARTESIAN_POINT('Ctrl Pts',(26.7064953106254,33.03156933761,0.));
#29615=CARTESIAN_POINT('Ctrl Pts',(26.7260352861619,33.131664100194,0.));
#29616=CARTESIAN_POINT('Ctrl Pts',(26.7450886617884,33.2319878786519,0.));
#29617=CARTESIAN_POINT('Ctrl Pts',(26.7636578270526,33.3325373307046,0.));
#29618=CARTESIAN_POINT('Ctrl Pts',(26.7817450041181,33.4333093513694,0.));
#29619=CARTESIAN_POINT('Ctrl Pts',(26.7993522966985,33.5343009499673,0.));
#29620=CARTESIAN_POINT('Ctrl Pts',(26.8164817280846,33.6355091508895,0.));
#29621=CARTESIAN_POINT('Ctrl Pts',(26.8331352836667,33.7369308933173,0.));
#29622=CARTESIAN_POINT('Ctrl Pts',(26.8493149627661,33.838562905895,0.));
#29623=CARTESIAN_POINT('Ctrl Pts',(26.8650228056313,33.9404016650487,0.));
#29624=CARTESIAN_POINT('Ctrl Pts',(26.880260834701,34.0424436187397,0.));
#29625=CARTESIAN_POINT('Ctrl Pts',(26.8950310138939,34.1446853651051,0.));
#29626=CARTESIAN_POINT('Ctrl Pts',(26.9093352037262,34.2471238425419,0.));
#29627=CARTESIAN_POINT('Ctrl Pts',(26.9231751225177,34.3497565255724,0.));
#29628=CARTESIAN_POINT('Ctrl Pts',(26.9392277420462,34.4731465943772,0.));
#29629=CARTESIAN_POINT('Ctrl Pts',(26.9520281195268,34.5762105502273,0.));
#29630=CARTESIAN_POINT('Ctrl Pts',(26.9619003236529,34.6588137898952,0.));
#29631=CARTESIAN_POINT('Ctrl Pts',(26.9690976283147,34.7208516760814,0.));
#29632=CARTESIAN_POINT('Ctrl Pts',(26.9738038986838,34.7622482477091,0.));
#29633=CARTESIAN_POINT('Ctrl Pts',(24.8345302882955,28.2149191006268,15.));
#29634=CARTESIAN_POINT('Ctrl Pts',(24.8470618363541,28.2291563988796,15.));
#29635=CARTESIAN_POINT('Ctrl Pts',(24.8717258526943,28.2579420132101,15.));
#29636=CARTESIAN_POINT('Ctrl Pts',(24.9075246543798,28.3020534756061,15.));
#29637=CARTESIAN_POINT('Ctrl Pts',(24.9529811166897,28.3626431274892,15.));
#29638=CARTESIAN_POINT('Ctrl Pts',(25.0066999111736,28.4408053900206,15.));
#29639=CARTESIAN_POINT('Ctrl Pts',(25.0581926620043,28.5207164321473,15.));
#29640=CARTESIAN_POINT('Ctrl Pts',(25.1083211582389,28.6017081342376,15.));
#29641=CARTESIAN_POINT('Ctrl Pts',(25.1577170374459,28.6832861366762,15.));
#29642=CARTESIAN_POINT('Ctrl Pts',(25.2066127148845,28.7652594076549,15.));
#29643=CARTESIAN_POINT('Ctrl Pts',(25.2549775629725,28.8476372998748,15.));
#29644=CARTESIAN_POINT('Ctrl Pts',(25.3026235249214,28.9305499160476,15.));
#29645=CARTESIAN_POINT('Ctrl Pts',(25.3493168206005,29.0141637699076,15.));
#29646=CARTESIAN_POINT('Ctrl Pts',(25.3948997321279,29.098589927237,15.));
#29647=CARTESIAN_POINT('Ctrl Pts',(25.4393679214513,29.183825549991,15.));
#29648=CARTESIAN_POINT('Ctrl Pts',(25.4828076101654,29.2698007967907,15.));
#29649=CARTESIAN_POINT('Ctrl Pts',(25.5253562922582,29.356408021119,15.));
#29650=CARTESIAN_POINT('Ctrl Pts',(25.5671572096726,29.443535683207,15.));
#29651=CARTESIAN_POINT('Ctrl Pts',(25.6083094352667,29.5311055094509,15.));
#29652=CARTESIAN_POINT('Ctrl Pts',(25.6488438125835,29.6190903904157,15.));
#29653=CARTESIAN_POINT('Ctrl Pts',(25.6887507922748,29.7074935910931,15.));
#29654=CARTESIAN_POINT('Ctrl Pts',(25.7279973711305,29.7963360859334,15.));
#29655=CARTESIAN_POINT('Ctrl Pts',(25.7665469042913,29.8856417535786,15.));
#29656=CARTESIAN_POINT('Ctrl Pts',(25.8043812318214,29.9754208429384,15.));
#29657=CARTESIAN_POINT('Ctrl Pts',(25.8415089241134,30.0656638016321,15.));
#29658=CARTESIAN_POINT('Ctrl Pts',(25.8779535511027,30.1563500154165,15.));
#29659=CARTESIAN_POINT('Ctrl Pts',(25.9137466853317,30.2474530144827,15.));
#29660=CARTESIAN_POINT('Ctrl Pts',(25.9489196635424,30.3389466074503,15.));
#29661=CARTESIAN_POINT('Ctrl Pts',(25.9834942765902,30.4308118142473,15.));
#29662=CARTESIAN_POINT('Ctrl Pts',(26.0174801292225,30.5230388264271,15.));
#29663=CARTESIAN_POINT('Ctrl Pts',(26.0508796503166,30.6156232634061,15.));
#29664=CARTESIAN_POINT('Ctrl Pts',(26.0836911730968,30.7085638682391,15.));
#29665=CARTESIAN_POINT('Ctrl Pts',(26.1159125093178,30.8018598357461,15.));
#29666=CARTESIAN_POINT('Ctrl Pts',(26.1475450294082,30.8955077633644,15.));
#29667=CARTESIAN_POINT('Ctrl Pts',(26.1785946616165,30.9895009017073,15.));
#29668=CARTESIAN_POINT('Ctrl Pts',(26.2090698085494,31.0838307058369,15.));
#29669=CARTESIAN_POINT('Ctrl Pts',(26.2389800738215,31.1784877826858,15.));
#29670=CARTESIAN_POINT('Ctrl Pts',(26.2683347859175,31.2734629900041,15.));
#29671=CARTESIAN_POINT('Ctrl Pts',(26.2971413115295,31.3687486937246,15.));
#29672=CARTESIAN_POINT('Ctrl Pts',(26.3254046890485,31.4643390378084,15.));
#29673=CARTESIAN_POINT('Ctrl Pts',(26.353128528169,31.5602292672984,15.));
#29674=CARTESIAN_POINT('Ctrl Pts',(26.3803155790949,31.6564152990236,15.));
#29675=CARTESIAN_POINT('Ctrl Pts',(26.4069683862784,31.7528932299312,15.));
#29676=CARTESIAN_POINT('Ctrl Pts',(26.433090040836,31.849658771403,15.));
#29677=CARTESIAN_POINT('Ctrl Pts',(26.4586843683627,31.9467071093816,15.));
#29678=CARTESIAN_POINT('Ctrl Pts',(26.4837555495616,32.0440331917233,15.));
#29679=CARTESIAN_POINT('Ctrl Pts',(26.5083078928862,32.1416319023705,15.));
#29680=CARTESIAN_POINT('Ctrl Pts',(26.5323455701117,32.2394982626669,15.));
#29681=CARTESIAN_POINT('Ctrl Pts',(26.5558723200361,32.3376276606981,15.));
#29682=CARTESIAN_POINT('Ctrl Pts',(26.5788913672813,32.4360159072985,15.));
#29683=CARTESIAN_POINT('Ctrl Pts',(26.6014055904817,32.5346590925498,15.));
#29684=CARTESIAN_POINT('Ctrl Pts',(26.6234176311245,32.6335534898935,15.));
#29685=CARTESIAN_POINT('Ctrl Pts',(26.6449300199763,32.7326954489334,15.));
#29686=CARTESIAN_POINT('Ctrl Pts',(26.6659453236976,32.8320812678271,15.));
#29687=CARTESIAN_POINT('Ctrl Pts',(26.6864661988935,32.9317071576181,15.));
#29688=CARTESIAN_POINT('Ctrl Pts',(26.7064953106254,33.03156933761,15.));
#29689=CARTESIAN_POINT('Ctrl Pts',(26.7260352861619,33.131664100194,15.));
#29690=CARTESIAN_POINT('Ctrl Pts',(26.7450886617884,33.2319878786519,15.));
#29691=CARTESIAN_POINT('Ctrl Pts',(26.7636578270526,33.3325373307046,15.));
#29692=CARTESIAN_POINT('Ctrl Pts',(26.7817450041181,33.4333093513694,15.));
#29693=CARTESIAN_POINT('Ctrl Pts',(26.7993522966985,33.5343009499673,15.));
#29694=CARTESIAN_POINT('Ctrl Pts',(26.8164817280846,33.6355091508895,15.));
#29695=CARTESIAN_POINT('Ctrl Pts',(26.8331352836667,33.7369308933173,15.));
#29696=CARTESIAN_POINT('Ctrl Pts',(26.8493149627661,33.838562905895,15.));
#29697=CARTESIAN_POINT('Ctrl Pts',(26.8650228056313,33.9404016650487,15.));
#29698=CARTESIAN_POINT('Ctrl Pts',(26.880260834701,34.0424436187397,15.));
#29699=CARTESIAN_POINT('Ctrl Pts',(26.8950310138939,34.1446853651051,15.));
#29700=CARTESIAN_POINT('Ctrl Pts',(26.9093352037262,34.2471238425419,15.));
#29701=CARTESIAN_POINT('Ctrl Pts',(26.9231751225177,34.3497565255724,15.));
#29702=CARTESIAN_POINT('Ctrl Pts',(26.9392277420462,34.4731465943772,15.));
#29703=CARTESIAN_POINT('Ctrl Pts',(26.9520281195268,34.5762105502273,15.));
#29704=CARTESIAN_POINT('Ctrl Pts',(26.9619003236529,34.6588137898952,15.));
#29705=CARTESIAN_POINT('Ctrl Pts',(26.9690976283147,34.7208516760814,15.));
#29706=CARTESIAN_POINT('Ctrl Pts',(26.9738038986838,34.7622482477091,15.));
#29707=CARTESIAN_POINT('Ctrl Pts',(34.7622482477091,26.9738038986838,0.));
#29708=CARTESIAN_POINT('Ctrl Pts',(34.7622482477091,26.9738038986838,18.));
#29709=CARTESIAN_POINT('Ctrl Pts',(34.7415499619104,26.9714507634923,0.));
#29710=CARTESIAN_POINT('Ctrl Pts',(34.7415499619104,26.9714507634923,18.));
#29711=CARTESIAN_POINT('Ctrl Pts',(34.700172380686,26.9666985267608,0.));
#29712=CARTESIAN_POINT('Ctrl Pts',(34.700172380686,26.9666985267608,18.));
#29713=CARTESIAN_POINT('Ctrl Pts',(34.6381629799782,26.9594322726214,0.));
#29714=CARTESIAN_POINT('Ctrl Pts',(34.6381629799782,26.9594322726214,18.));
#29715=CARTESIAN_POINT('Ctrl Pts',(34.5555977590573,26.9494680440307,0.));
#29716=CARTESIAN_POINT('Ctrl Pts',(34.5555977590573,26.9494680440307,18.));
#29717=CARTESIAN_POINT('Ctrl Pts',(34.4525815829097,26.936552305458,0.));
#29718=CARTESIAN_POINT('Ctrl Pts',(34.4525815829097,26.936552305458,18.));
#29719=CARTESIAN_POINT('Ctrl Pts',(34.3497565255724,26.9231751225177,0.));
#29720=CARTESIAN_POINT('Ctrl Pts',(34.3497565255724,26.9231751225177,18.));
#29721=CARTESIAN_POINT('Ctrl Pts',(34.2471238425419,26.9093352037262,0.));
#29722=CARTESIAN_POINT('Ctrl Pts',(34.2471238425419,26.9093352037262,18.));
#29723=CARTESIAN_POINT('Ctrl Pts',(34.1446853651051,26.8950310138939,0.));
#29724=CARTESIAN_POINT('Ctrl Pts',(34.1446853651051,26.8950310138939,18.));
#29725=CARTESIAN_POINT('Ctrl Pts',(34.0424436187397,26.880260834701,0.));
#29726=CARTESIAN_POINT('Ctrl Pts',(34.0424436187397,26.880260834701,18.));
#29727=CARTESIAN_POINT('Ctrl Pts',(33.9404016650487,26.8650228056313,0.));
#29728=CARTESIAN_POINT('Ctrl Pts',(33.9404016650487,26.8650228056313,18.));
#29729=CARTESIAN_POINT('Ctrl Pts',(33.838562905895,26.8493149627661,0.));
#29730=CARTESIAN_POINT('Ctrl Pts',(33.838562905895,26.8493149627661,18.));
#29731=CARTESIAN_POINT('Ctrl Pts',(33.7369308933173,26.8331352836666,0.));
#29732=CARTESIAN_POINT('Ctrl Pts',(33.7369308933173,26.8331352836666,18.));
#29733=CARTESIAN_POINT('Ctrl Pts',(33.6355091508895,26.8164817280846,0.));
#29734=CARTESIAN_POINT('Ctrl Pts',(33.6355091508895,26.8164817280846,18.));
#29735=CARTESIAN_POINT('Ctrl Pts',(33.5343009499673,26.7993522966985,0.));
#29736=CARTESIAN_POINT('Ctrl Pts',(33.5343009499673,26.7993522966985,18.));
#29737=CARTESIAN_POINT('Ctrl Pts',(33.4333093513694,26.7817450041181,0.));
#29738=CARTESIAN_POINT('Ctrl Pts',(33.4333093513694,26.7817450041181,18.));
#29739=CARTESIAN_POINT('Ctrl Pts',(33.3325373307046,26.7636578270526,0.));
#29740=CARTESIAN_POINT('Ctrl Pts',(33.3325373307046,26.7636578270526,18.));
#29741=CARTESIAN_POINT('Ctrl Pts',(33.2319878786519,26.7450886617884,0.));
#29742=CARTESIAN_POINT('Ctrl Pts',(33.2319878786519,26.7450886617884,18.));
#29743=CARTESIAN_POINT('Ctrl Pts',(33.131664100194,26.7260352861619,0.));
#29744=CARTESIAN_POINT('Ctrl Pts',(33.131664100194,26.7260352861619,18.));
#29745=CARTESIAN_POINT('Ctrl Pts',(33.03156933761,26.7064953106254,0.));
#29746=CARTESIAN_POINT('Ctrl Pts',(33.03156933761,26.7064953106254,18.));
#29747=CARTESIAN_POINT('Ctrl Pts',(32.9317071576181,26.6864661988935,0.));
#29748=CARTESIAN_POINT('Ctrl Pts',(32.9317071576181,26.6864661988935,18.));
#29749=CARTESIAN_POINT('Ctrl Pts',(32.8320812678271,26.6659453236976,0.));
#29750=CARTESIAN_POINT('Ctrl Pts',(32.8320812678271,26.6659453236976,18.));
#29751=CARTESIAN_POINT('Ctrl Pts',(32.7326954489334,26.6449300199763,0.));
#29752=CARTESIAN_POINT('Ctrl Pts',(32.7326954489334,26.6449300199763,18.));
#29753=CARTESIAN_POINT('Ctrl Pts',(32.6335534898935,26.6234176311244,0.));
#29754=CARTESIAN_POINT('Ctrl Pts',(32.6335534898935,26.6234176311244,18.));
#29755=CARTESIAN_POINT('Ctrl Pts',(32.5346590925498,26.6014055904817,0.));
#29756=CARTESIAN_POINT('Ctrl Pts',(32.5346590925498,26.6014055904817,18.));
#29757=CARTESIAN_POINT('Ctrl Pts',(32.4360159072985,26.5788913672813,0.));
#29758=CARTESIAN_POINT('Ctrl Pts',(32.4360159072985,26.5788913672813,18.));
#29759=CARTESIAN_POINT('Ctrl Pts',(32.3376276606981,26.5558723200361,0.));
#29760=CARTESIAN_POINT('Ctrl Pts',(32.3376276606981,26.5558723200361,18.));
#29761=CARTESIAN_POINT('Ctrl Pts',(32.2394982626669,26.5323455701117,0.));
#29762=CARTESIAN_POINT('Ctrl Pts',(32.2394982626669,26.5323455701117,18.));
#29763=CARTESIAN_POINT('Ctrl Pts',(32.1416319023705,26.5083078928862,0.));
#29764=CARTESIAN_POINT('Ctrl Pts',(32.1416319023705,26.5083078928862,18.));
#29765=CARTESIAN_POINT('Ctrl Pts',(32.0440331917233,26.4837555495616,0.));
#29766=CARTESIAN_POINT('Ctrl Pts',(32.0440331917233,26.4837555495616,18.));
#29767=CARTESIAN_POINT('Ctrl Pts',(31.9467071093816,26.4586843683627,0.));
#29768=CARTESIAN_POINT('Ctrl Pts',(31.9467071093816,26.4586843683627,18.));
#29769=CARTESIAN_POINT('Ctrl Pts',(31.849658771403,26.433090040836,0.));
#29770=CARTESIAN_POINT('Ctrl Pts',(31.849658771403,26.433090040836,18.));
#29771=CARTESIAN_POINT('Ctrl Pts',(31.7528932299312,26.4069683862784,0.));
#29772=CARTESIAN_POINT('Ctrl Pts',(31.7528932299312,26.4069683862784,18.));
#29773=CARTESIAN_POINT('Ctrl Pts',(31.6564152990236,26.3803155790949,0.));
#29774=CARTESIAN_POINT('Ctrl Pts',(31.6564152990236,26.3803155790949,18.));
#29775=CARTESIAN_POINT('Ctrl Pts',(31.5602292672984,26.353128528169,0.));
#29776=CARTESIAN_POINT('Ctrl Pts',(31.5602292672984,26.353128528169,18.));
#29777=CARTESIAN_POINT('Ctrl Pts',(31.4643390378084,26.3254046890485,0.));
#29778=CARTESIAN_POINT('Ctrl Pts',(31.4643390378084,26.3254046890485,18.));
#29779=CARTESIAN_POINT('Ctrl Pts',(31.3687486937246,26.2971413115295,0.));
#29780=CARTESIAN_POINT('Ctrl Pts',(31.3687486937246,26.2971413115295,18.));
#29781=CARTESIAN_POINT('Ctrl Pts',(31.2734629900041,26.2683347859175,0.));
#29782=CARTESIAN_POINT('Ctrl Pts',(31.2734629900041,26.2683347859175,18.));
#29783=CARTESIAN_POINT('Ctrl Pts',(31.1784877826858,26.2389800738215,0.));
#29784=CARTESIAN_POINT('Ctrl Pts',(31.1784877826858,26.2389800738215,18.));
#29785=CARTESIAN_POINT('Ctrl Pts',(31.0838307058369,26.2090698085494,0.));
#29786=CARTESIAN_POINT('Ctrl Pts',(31.0838307058369,26.2090698085494,18.));
#29787=CARTESIAN_POINT('Ctrl Pts',(30.9895009017073,26.1785946616165,0.));
#29788=CARTESIAN_POINT('Ctrl Pts',(30.9895009017073,26.1785946616165,18.));
#29789=CARTESIAN_POINT('Ctrl Pts',(30.8955077633644,26.1475450294082,0.));
#29790=CARTESIAN_POINT('Ctrl Pts',(30.8955077633644,26.1475450294082,18.));
#29791=CARTESIAN_POINT('Ctrl Pts',(30.8018598357461,26.1159125093178,0.));
#29792=CARTESIAN_POINT('Ctrl Pts',(30.8018598357461,26.1159125093178,18.));
#29793=CARTESIAN_POINT('Ctrl Pts',(30.7085638682391,26.0836911730968,0.));
#29794=CARTESIAN_POINT('Ctrl Pts',(30.7085638682391,26.0836911730968,18.));
#29795=CARTESIAN_POINT('Ctrl Pts',(30.6156232634061,26.0508796503166,0.));
#29796=CARTESIAN_POINT('Ctrl Pts',(30.6156232634061,26.0508796503166,18.));
#29797=CARTESIAN_POINT('Ctrl Pts',(30.5230388264271,26.0174801292225,0.));
#29798=CARTESIAN_POINT('Ctrl Pts',(30.5230388264271,26.0174801292225,18.));
#29799=CARTESIAN_POINT('Ctrl Pts',(30.4308118142473,25.9834942765902,0.));
#29800=CARTESIAN_POINT('Ctrl Pts',(30.4308118142473,25.9834942765902,18.));
#29801=CARTESIAN_POINT('Ctrl Pts',(30.3389466074503,25.9489196635424,0.));
#29802=CARTESIAN_POINT('Ctrl Pts',(30.3389466074503,25.9489196635424,18.));
#29803=CARTESIAN_POINT('Ctrl Pts',(30.2474530144827,25.9137466853317,0.));
#29804=CARTESIAN_POINT('Ctrl Pts',(30.2474530144827,25.9137466853317,18.));
#29805=CARTESIAN_POINT('Ctrl Pts',(30.1563500154165,25.8779535511027,0.));
#29806=CARTESIAN_POINT('Ctrl Pts',(30.1563500154165,25.8779535511027,18.));
#29807=CARTESIAN_POINT('Ctrl Pts',(30.0656638016321,25.8415089241134,0.));
#29808=CARTESIAN_POINT('Ctrl Pts',(30.0656638016321,25.8415089241134,18.));
#29809=CARTESIAN_POINT('Ctrl Pts',(29.9754208429384,25.8043812318214,0.));
#29810=CARTESIAN_POINT('Ctrl Pts',(29.9754208429384,25.8043812318214,18.));
#29811=CARTESIAN_POINT('Ctrl Pts',(29.8856417535786,25.7665469042913,0.));
#29812=CARTESIAN_POINT('Ctrl Pts',(29.8856417535786,25.7665469042913,18.));
#29813=CARTESIAN_POINT('Ctrl Pts',(29.7963360859334,25.7279973711305,0.));
#29814=CARTESIAN_POINT('Ctrl Pts',(29.7963360859334,25.7279973711305,18.));
#29815=CARTESIAN_POINT('Ctrl Pts',(29.7074935910931,25.6887507922748,0.));
#29816=CARTESIAN_POINT('Ctrl Pts',(29.7074935910931,25.6887507922748,18.));
#29817=CARTESIAN_POINT('Ctrl Pts',(29.6190903904157,25.6488438125835,0.));
#29818=CARTESIAN_POINT('Ctrl Pts',(29.6190903904157,25.6488438125835,18.));
#29819=CARTESIAN_POINT('Ctrl Pts',(29.5311055094509,25.6083094352667,0.));
#29820=CARTESIAN_POINT('Ctrl Pts',(29.5311055094509,25.6083094352667,18.));
#29821=CARTESIAN_POINT('Ctrl Pts',(29.443535683207,25.5671572096726,0.));
#29822=CARTESIAN_POINT('Ctrl Pts',(29.443535683207,25.5671572096726,18.));
#29823=CARTESIAN_POINT('Ctrl Pts',(29.356408021119,25.5253562922582,0.));
#29824=CARTESIAN_POINT('Ctrl Pts',(29.356408021119,25.5253562922582,18.));
#29825=CARTESIAN_POINT('Ctrl Pts',(29.2698007967907,25.4828076101654,0.));
#29826=CARTESIAN_POINT('Ctrl Pts',(29.2698007967907,25.4828076101654,18.));
#29827=CARTESIAN_POINT('Ctrl Pts',(29.183825549991,25.4393679214513,0.));
#29828=CARTESIAN_POINT('Ctrl Pts',(29.183825549991,25.4393679214513,18.));
#29829=CARTESIAN_POINT('Ctrl Pts',(29.098589927237,25.3948997321279,0.));
#29830=CARTESIAN_POINT('Ctrl Pts',(29.098589927237,25.3948997321279,18.));
#29831=CARTESIAN_POINT('Ctrl Pts',(29.0141637699076,25.3493168206005,0.));
#29832=CARTESIAN_POINT('Ctrl Pts',(29.0141637699076,25.3493168206005,18.));
#29833=CARTESIAN_POINT('Ctrl Pts',(28.9305499160476,25.3026235249214,0.));
#29834=CARTESIAN_POINT('Ctrl Pts',(28.9305499160476,25.3026235249214,18.));
#29835=CARTESIAN_POINT('Ctrl Pts',(28.8476372998748,25.2549775629725,0.));
#29836=CARTESIAN_POINT('Ctrl Pts',(28.8476372998748,25.2549775629725,18.));
#29837=CARTESIAN_POINT('Ctrl Pts',(28.7652594076549,25.2066127148845,0.));
#29838=CARTESIAN_POINT('Ctrl Pts',(28.7652594076549,25.2066127148845,18.));
#29839=CARTESIAN_POINT('Ctrl Pts',(28.6832861366762,25.1577170374459,0.));
#29840=CARTESIAN_POINT('Ctrl Pts',(28.6832861366762,25.1577170374459,18.));
#29841=CARTESIAN_POINT('Ctrl Pts',(28.6017081342376,25.1083211582389,0.));
#29842=CARTESIAN_POINT('Ctrl Pts',(28.6017081342376,25.1083211582389,18.));
#29843=CARTESIAN_POINT('Ctrl Pts',(28.5207164321473,25.0581926620043,0.));
#29844=CARTESIAN_POINT('Ctrl Pts',(28.5207164321473,25.0581926620043,18.));
#29845=CARTESIAN_POINT('Ctrl Pts',(28.4408053900206,25.0066999111736,0.));
#29846=CARTESIAN_POINT('Ctrl Pts',(28.4408053900206,25.0066999111736,18.));
#29847=CARTESIAN_POINT('Ctrl Pts',(28.3626431274892,24.9529811166897,0.));
#29848=CARTESIAN_POINT('Ctrl Pts',(28.3626431274892,24.9529811166897,18.));
#29849=CARTESIAN_POINT('Ctrl Pts',(28.3020534756061,24.9075246543798,0.));
#29850=CARTESIAN_POINT('Ctrl Pts',(28.3020534756061,24.9075246543798,18.));
#29851=CARTESIAN_POINT('Ctrl Pts',(28.2579420132101,24.8717258526943,0.));
#29852=CARTESIAN_POINT('Ctrl Pts',(28.2579420132101,24.8717258526943,18.));
#29853=CARTESIAN_POINT('Ctrl Pts',(28.2291563988796,24.8470618363541,0.));
#29854=CARTESIAN_POINT('Ctrl Pts',(28.2291563988796,24.8470618363541,18.));
#29855=CARTESIAN_POINT('Ctrl Pts',(28.2149191006269,24.8345302882955,0.));
#29856=CARTESIAN_POINT('Ctrl Pts',(28.2149191006269,24.8345302882955,18.));
#29857=CARTESIAN_POINT('',(34.762248247709,26.9738038986839,0.));
#29858=CARTESIAN_POINT('Ctrl Pts',(28.2149191006269,24.8345302882955,0.));
#29859=CARTESIAN_POINT('Ctrl Pts',(28.2291563988796,24.8470618363541,0.));
#29860=CARTESIAN_POINT('Ctrl Pts',(28.2579420132101,24.8717258526943,0.));
#29861=CARTESIAN_POINT('Ctrl Pts',(28.3020534756061,24.9075246543798,0.));
#29862=CARTESIAN_POINT('Ctrl Pts',(28.3626431274892,24.9529811166897,0.));
#29863=CARTESIAN_POINT('Ctrl Pts',(28.4408053900206,25.0066999111736,0.));
#29864=CARTESIAN_POINT('Ctrl Pts',(28.5207164321473,25.0581926620043,0.));
#29865=CARTESIAN_POINT('Ctrl Pts',(28.6017081342376,25.1083211582389,0.));
#29866=CARTESIAN_POINT('Ctrl Pts',(28.6832861366762,25.1577170374459,0.));
#29867=CARTESIAN_POINT('Ctrl Pts',(28.7652594076549,25.2066127148845,0.));
#29868=CARTESIAN_POINT('Ctrl Pts',(28.8476372998748,25.2549775629725,0.));
#29869=CARTESIAN_POINT('Ctrl Pts',(28.9305499160476,25.3026235249214,0.));
#29870=CARTESIAN_POINT('Ctrl Pts',(29.0141637699076,25.3493168206005,0.));
#29871=CARTESIAN_POINT('Ctrl Pts',(29.098589927237,25.3948997321279,0.));
#29872=CARTESIAN_POINT('Ctrl Pts',(29.183825549991,25.4393679214513,0.));
#29873=CARTESIAN_POINT('Ctrl Pts',(29.2698007967907,25.4828076101654,0.));
#29874=CARTESIAN_POINT('Ctrl Pts',(29.356408021119,25.5253562922582,0.));
#29875=CARTESIAN_POINT('Ctrl Pts',(29.443535683207,25.5671572096726,0.));
#29876=CARTESIAN_POINT('Ctrl Pts',(29.5311055094509,25.6083094352667,0.));
#29877=CARTESIAN_POINT('Ctrl Pts',(29.6190903904157,25.6488438125835,0.));
#29878=CARTESIAN_POINT('Ctrl Pts',(29.7074935910931,25.6887507922748,0.));
#29879=CARTESIAN_POINT('Ctrl Pts',(29.7963360859334,25.7279973711305,0.));
#29880=CARTESIAN_POINT('Ctrl Pts',(29.8856417535786,25.7665469042913,0.));
#29881=CARTESIAN_POINT('Ctrl Pts',(29.9754208429384,25.8043812318214,0.));
#29882=CARTESIAN_POINT('Ctrl Pts',(30.0656638016321,25.8415089241134,0.));
#29883=CARTESIAN_POINT('Ctrl Pts',(30.1563500154165,25.8779535511027,0.));
#29884=CARTESIAN_POINT('Ctrl Pts',(30.2474530144827,25.9137466853317,0.));
#29885=CARTESIAN_POINT('Ctrl Pts',(30.3389466074503,25.9489196635424,0.));
#29886=CARTESIAN_POINT('Ctrl Pts',(30.4308118142473,25.9834942765902,0.));
#29887=CARTESIAN_POINT('Ctrl Pts',(30.5230388264271,26.0174801292225,0.));
#29888=CARTESIAN_POINT('Ctrl Pts',(30.6156232634061,26.0508796503166,0.));
#29889=CARTESIAN_POINT('Ctrl Pts',(30.7085638682391,26.0836911730968,0.));
#29890=CARTESIAN_POINT('Ctrl Pts',(30.8018598357461,26.1159125093178,0.));
#29891=CARTESIAN_POINT('Ctrl Pts',(30.8955077633644,26.1475450294082,0.));
#29892=CARTESIAN_POINT('Ctrl Pts',(30.9895009017073,26.1785946616165,0.));
#29893=CARTESIAN_POINT('Ctrl Pts',(31.0838307058369,26.2090698085494,0.));
#29894=CARTESIAN_POINT('Ctrl Pts',(31.1784877826858,26.2389800738215,0.));
#29895=CARTESIAN_POINT('Ctrl Pts',(31.2734629900041,26.2683347859175,0.));
#29896=CARTESIAN_POINT('Ctrl Pts',(31.3687486937246,26.2971413115295,0.));
#29897=CARTESIAN_POINT('Ctrl Pts',(31.4643390378084,26.3254046890485,0.));
#29898=CARTESIAN_POINT('Ctrl Pts',(31.5602292672984,26.353128528169,0.));
#29899=CARTESIAN_POINT('Ctrl Pts',(31.6564152990236,26.3803155790949,0.));
#29900=CARTESIAN_POINT('Ctrl Pts',(31.7528932299312,26.4069683862784,0.));
#29901=CARTESIAN_POINT('Ctrl Pts',(31.849658771403,26.433090040836,0.));
#29902=CARTESIAN_POINT('Ctrl Pts',(31.9467071093816,26.4586843683627,0.));
#29903=CARTESIAN_POINT('Ctrl Pts',(32.0440331917233,26.4837555495616,0.));
#29904=CARTESIAN_POINT('Ctrl Pts',(32.1416319023705,26.5083078928862,0.));
#29905=CARTESIAN_POINT('Ctrl Pts',(32.2394982626669,26.5323455701117,0.));
#29906=CARTESIAN_POINT('Ctrl Pts',(32.3376276606981,26.5558723200361,0.));
#29907=CARTESIAN_POINT('Ctrl Pts',(32.4360159072985,26.5788913672813,0.));
#29908=CARTESIAN_POINT('Ctrl Pts',(32.5346590925498,26.6014055904817,0.));
#29909=CARTESIAN_POINT('Ctrl Pts',(32.6335534898935,26.6234176311244,0.));
#29910=CARTESIAN_POINT('Ctrl Pts',(32.7326954489334,26.6449300199763,0.));
#29911=CARTESIAN_POINT('Ctrl Pts',(32.8320812678271,26.6659453236976,0.));
#29912=CARTESIAN_POINT('Ctrl Pts',(32.9317071576181,26.6864661988935,0.));
#29913=CARTESIAN_POINT('Ctrl Pts',(33.03156933761,26.7064953106254,0.));
#29914=CARTESIAN_POINT('Ctrl Pts',(33.131664100194,26.7260352861619,0.));
#29915=CARTESIAN_POINT('Ctrl Pts',(33.2319878786519,26.7450886617884,0.));
#29916=CARTESIAN_POINT('Ctrl Pts',(33.3325373307046,26.7636578270526,0.));
#29917=CARTESIAN_POINT('Ctrl Pts',(33.4333093513694,26.7817450041181,0.));
#29918=CARTESIAN_POINT('Ctrl Pts',(33.5343009499673,26.7993522966985,0.));
#29919=CARTESIAN_POINT('Ctrl Pts',(33.6355091508895,26.8164817280846,0.));
#29920=CARTESIAN_POINT('Ctrl Pts',(33.7369308933173,26.8331352836666,0.));
#29921=CARTESIAN_POINT('Ctrl Pts',(33.838562905895,26.8493149627661,0.));
#29922=CARTESIAN_POINT('Ctrl Pts',(33.9404016650487,26.8650228056313,0.));
#29923=CARTESIAN_POINT('Ctrl Pts',(34.0424436187397,26.880260834701,0.));
#29924=CARTESIAN_POINT('Ctrl Pts',(34.1446853651051,26.8950310138939,0.));
#29925=CARTESIAN_POINT('Ctrl Pts',(34.2471238425419,26.9093352037262,0.));
#29926=CARTESIAN_POINT('Ctrl Pts',(34.3497565255724,26.9231751225177,0.));
#29927=CARTESIAN_POINT('Ctrl Pts',(34.4731465943772,26.9392277420461,0.));
#29928=CARTESIAN_POINT('Ctrl Pts',(34.5762105502273,26.9520281195269,0.));
#29929=CARTESIAN_POINT('Ctrl Pts',(34.6588137898952,26.9619003236529,0.));
#29930=CARTESIAN_POINT('Ctrl Pts',(34.7208516760814,26.9690976283147,0.));
#29931=CARTESIAN_POINT('Ctrl Pts',(34.7622482477091,26.9738038986838,0.));
#29932=CARTESIAN_POINT('',(34.762248247709,26.9738038986839,15.));
#29933=CARTESIAN_POINT('Ctrl Pts',(34.7622482477091,26.9738038986838,15.));
#29934=CARTESIAN_POINT('Ctrl Pts',(34.7415499619104,26.9714507634923,15.));
#29935=CARTESIAN_POINT('Ctrl Pts',(34.700172380686,26.9666985267608,15.));
#29936=CARTESIAN_POINT('Ctrl Pts',(34.6381629799782,26.9594322726214,15.));
#29937=CARTESIAN_POINT('Ctrl Pts',(34.5555977590573,26.9494680440307,15.));
#29938=CARTESIAN_POINT('Ctrl Pts',(34.4525815829097,26.936552305458,15.));
#29939=CARTESIAN_POINT('Ctrl Pts',(34.3497565255724,26.9231751225177,15.));
#29940=CARTESIAN_POINT('Ctrl Pts',(34.2471238425419,26.9093352037262,15.));
#29941=CARTESIAN_POINT('Ctrl Pts',(34.1446853651051,26.8950310138939,15.));
#29942=CARTESIAN_POINT('Ctrl Pts',(34.0424436187397,26.880260834701,15.));
#29943=CARTESIAN_POINT('Ctrl Pts',(33.9404016650487,26.8650228056313,15.));
#29944=CARTESIAN_POINT('Ctrl Pts',(33.838562905895,26.8493149627661,15.));
#29945=CARTESIAN_POINT('Ctrl Pts',(33.7369308933173,26.8331352836666,15.));
#29946=CARTESIAN_POINT('Ctrl Pts',(33.6355091508895,26.8164817280846,15.));
#29947=CARTESIAN_POINT('Ctrl Pts',(33.5343009499673,26.7993522966985,15.));
#29948=CARTESIAN_POINT('Ctrl Pts',(33.4333093513694,26.7817450041181,15.));
#29949=CARTESIAN_POINT('Ctrl Pts',(33.3325373307046,26.7636578270526,15.));
#29950=CARTESIAN_POINT('Ctrl Pts',(33.2319878786519,26.7450886617884,15.));
#29951=CARTESIAN_POINT('Ctrl Pts',(33.131664100194,26.7260352861619,15.));
#29952=CARTESIAN_POINT('Ctrl Pts',(33.03156933761,26.7064953106254,15.));
#29953=CARTESIAN_POINT('Ctrl Pts',(32.9317071576181,26.6864661988935,15.));
#29954=CARTESIAN_POINT('Ctrl Pts',(32.8320812678271,26.6659453236976,15.));
#29955=CARTESIAN_POINT('Ctrl Pts',(32.7326954489334,26.6449300199763,15.));
#29956=CARTESIAN_POINT('Ctrl Pts',(32.6335534898935,26.6234176311244,15.));
#29957=CARTESIAN_POINT('Ctrl Pts',(32.5346590925498,26.6014055904817,15.));
#29958=CARTESIAN_POINT('Ctrl Pts',(32.4360159072985,26.5788913672813,15.));
#29959=CARTESIAN_POINT('Ctrl Pts',(32.3376276606981,26.5558723200361,15.));
#29960=CARTESIAN_POINT('Ctrl Pts',(32.2394982626669,26.5323455701117,15.));
#29961=CARTESIAN_POINT('Ctrl Pts',(32.1416319023705,26.5083078928862,15.));
#29962=CARTESIAN_POINT('Ctrl Pts',(32.0440331917233,26.4837555495616,15.));
#29963=CARTESIAN_POINT('Ctrl Pts',(31.9467071093816,26.4586843683627,15.));
#29964=CARTESIAN_POINT('Ctrl Pts',(31.849658771403,26.433090040836,15.));
#29965=CARTESIAN_POINT('Ctrl Pts',(31.7528932299312,26.4069683862784,15.));
#29966=CARTESIAN_POINT('Ctrl Pts',(31.6564152990236,26.3803155790949,15.));
#29967=CARTESIAN_POINT('Ctrl Pts',(31.5602292672984,26.353128528169,15.));
#29968=CARTESIAN_POINT('Ctrl Pts',(31.4643390378084,26.3254046890485,15.));
#29969=CARTESIAN_POINT('Ctrl Pts',(31.3687486937246,26.2971413115295,15.));
#29970=CARTESIAN_POINT('Ctrl Pts',(31.2734629900041,26.2683347859175,15.));
#29971=CARTESIAN_POINT('Ctrl Pts',(31.1784877826858,26.2389800738215,15.));
#29972=CARTESIAN_POINT('Ctrl Pts',(31.0838307058369,26.2090698085494,15.));
#29973=CARTESIAN_POINT('Ctrl Pts',(30.9895009017073,26.1785946616165,15.));
#29974=CARTESIAN_POINT('Ctrl Pts',(30.8955077633644,26.1475450294082,15.));
#29975=CARTESIAN_POINT('Ctrl Pts',(30.8018598357461,26.1159125093178,15.));
#29976=CARTESIAN_POINT('Ctrl Pts',(30.7085638682391,26.0836911730968,15.));
#29977=CARTESIAN_POINT('Ctrl Pts',(30.6156232634061,26.0508796503166,15.));
#29978=CARTESIAN_POINT('Ctrl Pts',(30.5230388264271,26.0174801292225,15.));
#29979=CARTESIAN_POINT('Ctrl Pts',(30.4308118142473,25.9834942765902,15.));
#29980=CARTESIAN_POINT('Ctrl Pts',(30.3389466074503,25.9489196635424,15.));
#29981=CARTESIAN_POINT('Ctrl Pts',(30.2474530144827,25.9137466853317,15.));
#29982=CARTESIAN_POINT('Ctrl Pts',(30.1563500154165,25.8779535511027,15.));
#29983=CARTESIAN_POINT('Ctrl Pts',(30.0656638016321,25.8415089241134,15.));
#29984=CARTESIAN_POINT('Ctrl Pts',(29.9754208429384,25.8043812318214,15.));
#29985=CARTESIAN_POINT('Ctrl Pts',(29.8856417535786,25.7665469042913,15.));
#29986=CARTESIAN_POINT('Ctrl Pts',(29.7963360859334,25.7279973711305,15.));
#29987=CARTESIAN_POINT('Ctrl Pts',(29.7074935910931,25.6887507922748,15.));
#29988=CARTESIAN_POINT('Ctrl Pts',(29.6190903904157,25.6488438125835,15.));
#29989=CARTESIAN_POINT('Ctrl Pts',(29.5311055094509,25.6083094352667,15.));
#29990=CARTESIAN_POINT('Ctrl Pts',(29.443535683207,25.5671572096726,15.));
#29991=CARTESIAN_POINT('Ctrl Pts',(29.356408021119,25.5253562922582,15.));
#29992=CARTESIAN_POINT('Ctrl Pts',(29.2698007967907,25.4828076101654,15.));
#29993=CARTESIAN_POINT('Ctrl Pts',(29.183825549991,25.4393679214513,15.));
#29994=CARTESIAN_POINT('Ctrl Pts',(29.098589927237,25.3948997321279,15.));
#29995=CARTESIAN_POINT('Ctrl Pts',(29.0141637699076,25.3493168206005,15.));
#29996=CARTESIAN_POINT('Ctrl Pts',(28.9305499160476,25.3026235249214,15.));
#29997=CARTESIAN_POINT('Ctrl Pts',(28.8476372998748,25.2549775629725,15.));
#29998=CARTESIAN_POINT('Ctrl Pts',(28.7652594076549,25.2066127148845,15.));
#29999=CARTESIAN_POINT('Ctrl Pts',(28.6832861366762,25.1577170374459,15.));
#30000=CARTESIAN_POINT('Ctrl Pts',(28.6017081342376,25.1083211582389,15.));
#30001=CARTESIAN_POINT('Ctrl Pts',(28.5207164321473,25.0581926620043,15.));
#30002=CARTESIAN_POINT('Ctrl Pts',(28.4408053900206,25.0066999111736,15.));
#30003=CARTESIAN_POINT('Ctrl Pts',(28.3626431274892,24.9529811166897,15.));
#30004=CARTESIAN_POINT('Ctrl Pts',(28.3020534756061,24.9075246543798,15.));
#30005=CARTESIAN_POINT('Ctrl Pts',(28.2579420132101,24.8717258526943,15.));
#30006=CARTESIAN_POINT('Ctrl Pts',(28.2291563988796,24.8470618363541,15.));
#30007=CARTESIAN_POINT('Ctrl Pts',(28.2149191006269,24.8345302882955,15.));
#30008=CARTESIAN_POINT('',(34.762248247709,26.9738038986839,0.));
#30009=CARTESIAN_POINT('Origin',(9.16871631793044E-12,6.66146233219319E-12,
0.));
#30010=CARTESIAN_POINT('',(36.3957374383337,24.725498909423,0.));
#30011=CARTESIAN_POINT('Origin',(9.16871631793044E-12,6.66146233219319E-12,
0.));
#30012=CARTESIAN_POINT('',(36.3957374383337,24.725498909423,15.));
#30013=CARTESIAN_POINT('Origin',(9.16871631793044E-12,6.66146233219319E-12,
15.));
#30014=CARTESIAN_POINT('',(36.3957374383337,24.725498909423,0.));
#30015=CARTESIAN_POINT('Ctrl Pts',(32.3379313568208,19.1596907609891,0.));
#30016=CARTESIAN_POINT('Ctrl Pts',(32.3379313568208,19.1596907609891,18.));
#30017=CARTESIAN_POINT('Ctrl Pts',(32.3542491343753,19.1693587749508,0.));
#30018=CARTESIAN_POINT('Ctrl Pts',(32.3542491343753,19.1693587749508,18.));
#30019=CARTESIAN_POINT('Ctrl Pts',(32.3866012518553,19.1891139208368,0.));
#30020=CARTESIAN_POINT('Ctrl Pts',(32.3866012518553,19.1891139208368,18.));
#30021=CARTESIAN_POINT('Ctrl Pts',(32.4342791270009,19.2200039764927,0.));
#30022=CARTESIAN_POINT('Ctrl Pts',(32.4342791270009,19.2200039764927,18.));
#30023=CARTESIAN_POINT('Ctrl Pts',(32.4962340238036,19.2635813403783,0.));
#30024=CARTESIAN_POINT('Ctrl Pts',(32.4962340238036,19.2635813403783,18.));
#30025=CARTESIAN_POINT('Ctrl Pts',(32.5714771007861,19.3213180490743,0.));
#30026=CARTESIAN_POINT('Ctrl Pts',(32.5714771007861,19.3213180490743,18.));
#30027=CARTESIAN_POINT('Ctrl Pts',(32.6451434870609,19.381405831319,0.));
#30028=CARTESIAN_POINT('Ctrl Pts',(32.6451434870609,19.381405831319,18.));
#30029=CARTESIAN_POINT('Ctrl Pts',(32.7178463324062,19.4429429601189,0.));
#30030=CARTESIAN_POINT('Ctrl Pts',(32.7178463324062,19.4429429601189,18.));
#30031=CARTESIAN_POINT('Ctrl Pts',(32.7900335943248,19.5052640847974,0.));
#30032=CARTESIAN_POINT('Ctrl Pts',(32.7900335943248,19.5052640847974,18.));
#30033=CARTESIAN_POINT('Ctrl Pts',(32.8618672807884,19.5681157030437,0.));
#30034=CARTESIAN_POINT('Ctrl Pts',(32.8618672807884,19.5681157030437,18.));
#30035=CARTESIAN_POINT('Ctrl Pts',(32.9333211533788,19.6315161742485,0.));
#30036=CARTESIAN_POINT('Ctrl Pts',(32.9333211533788,19.6315161742485,18.));
#30037=CARTESIAN_POINT('Ctrl Pts',(33.004256563411,19.6956473461873,0.));
#30038=CARTESIAN_POINT('Ctrl Pts',(33.004256563411,19.6956473461873,18.));
#30039=CARTESIAN_POINT('Ctrl Pts',(33.0745026283418,19.7607398248651,0.));
#30040=CARTESIAN_POINT('Ctrl Pts',(33.0745026283418,19.7607398248651,18.));
#30041=CARTESIAN_POINT('Ctrl Pts',(33.1439436707661,19.8269479776239,0.));
#30042=CARTESIAN_POINT('Ctrl Pts',(33.1439436707661,19.8269479776239,18.));
#30043=CARTESIAN_POINT('Ctrl Pts',(33.2125746879471,19.8942704458546,0.));
#30044=CARTESIAN_POINT('Ctrl Pts',(33.2125746879471,19.8942704458546,18.));
#30045=CARTESIAN_POINT('Ctrl Pts',(33.2804560993213,19.9626141625205,0.));
#30046=CARTESIAN_POINT('Ctrl Pts',(33.2804560993213,19.9626141625205,18.));
#30047=CARTESIAN_POINT('Ctrl Pts',(33.3476854048385,20.0318342617212,0.));
#30048=CARTESIAN_POINT('Ctrl Pts',(33.3476854048385,20.0318342617212,18.));
#30049=CARTESIAN_POINT('Ctrl Pts',(33.4143643679979,20.1017803986381,0.));
#30050=CARTESIAN_POINT('Ctrl Pts',(33.4143643679979,20.1017803986381,18.));
#30051=CARTESIAN_POINT('Ctrl Pts',(33.480563024813,20.1723475154533,0.));
#30052=CARTESIAN_POINT('Ctrl Pts',(33.480563024813,20.1723475154533,18.));
#30053=CARTESIAN_POINT('Ctrl Pts',(33.5463023319603,20.243500298383,0.));
#30054=CARTESIAN_POINT('Ctrl Pts',(33.5463023319603,20.243500298383,18.));
#30055=CARTESIAN_POINT('Ctrl Pts',(33.6115742164079,20.3152448035298,0.));
#30056=CARTESIAN_POINT('Ctrl Pts',(33.6115742164079,20.3152448035298,18.));
#30057=CARTESIAN_POINT('Ctrl Pts',(33.6763537716992,20.3876111773341,0.));
#30058=CARTESIAN_POINT('Ctrl Pts',(33.6763537716992,20.3876111773341,18.));
#30059=CARTESIAN_POINT('Ctrl Pts',(33.7406135254082,20.4606334536183,0.));
#30060=CARTESIAN_POINT('Ctrl Pts',(33.7406135254082,20.4606334536183,18.));
#30061=CARTESIAN_POINT('Ctrl Pts',(33.8043393734971,20.5343269914034,0.));
#30062=CARTESIAN_POINT('Ctrl Pts',(33.8043393734971,20.5343269914034,18.));
#30063=CARTESIAN_POINT('Ctrl Pts',(33.8675365150454,20.6086800574386,0.));
#30064=CARTESIAN_POINT('Ctrl Pts',(33.8675365150454,20.6086800574386,18.));
#30065=CARTESIAN_POINT('Ctrl Pts',(33.9302209962425,20.683665762903,0.));
#30066=CARTESIAN_POINT('Ctrl Pts',(33.9302209962425,20.683665762903,18.));
#30067=CARTESIAN_POINT('Ctrl Pts',(33.9924146647395,20.7592491770603,0.));
#30068=CARTESIAN_POINT('Ctrl Pts',(33.9924146647395,20.7592491770603,18.));
#30069=CARTESIAN_POINT('Ctrl Pts',(34.0541392299678,20.8353957068415,0.));
#30070=CARTESIAN_POINT('Ctrl Pts',(34.0541392299678,20.8353957068415,18.));
#30071=CARTESIAN_POINT('Ctrl Pts',(34.1154095510973,20.9120805673809,0.));
#30072=CARTESIAN_POINT('Ctrl Pts',(34.1154095510973,20.9120805673809,18.));
#30073=CARTESIAN_POINT('Ctrl Pts',(34.176231731809,20.9892914622612,0.));
#30074=CARTESIAN_POINT('Ctrl Pts',(34.176231731809,20.9892914622612,18.));
#30075=CARTESIAN_POINT('Ctrl Pts',(34.2366067284279,21.0670234747355,0.));
#30076=CARTESIAN_POINT('Ctrl Pts',(34.2366067284279,21.0670234747355,18.));
#30077=CARTESIAN_POINT('Ctrl Pts',(34.2965325673384,21.1452759244399,0.));
#30078=CARTESIAN_POINT('Ctrl Pts',(34.2965325673384,21.1452759244399,18.));
#30079=CARTESIAN_POINT('Ctrl Pts',(34.3560069185815,21.2240487218079,0.));
#30080=CARTESIAN_POINT('Ctrl Pts',(34.3560069185815,21.2240487218079,18.));
#30081=CARTESIAN_POINT('Ctrl Pts',(34.4150300340623,21.3033382073239,0.));
#30082=CARTESIAN_POINT('Ctrl Pts',(34.4150300340623,21.3033382073239,18.));
#30083=CARTESIAN_POINT('Ctrl Pts',(34.4736054662052,21.3831361300104,0.));
#30084=CARTESIAN_POINT('Ctrl Pts',(34.4736054662052,21.3831361300104,18.));
#30085=CARTESIAN_POINT('Ctrl Pts',(34.5317385658329,21.4634317666005,0.));
#30086=CARTESIAN_POINT('Ctrl Pts',(34.5317385658329,21.4634317666005,18.));
#30087=CARTESIAN_POINT('Ctrl Pts',(34.5894355639082,21.5442132160757,0.));
#30088=CARTESIAN_POINT('Ctrl Pts',(34.5894355639082,21.5442132160757,18.));
#30089=CARTESIAN_POINT('Ctrl Pts',(34.6467025072367,21.6254689009796,0.));
#30090=CARTESIAN_POINT('Ctrl Pts',(34.6467025072367,21.6254689009796,18.));
#30091=CARTESIAN_POINT('Ctrl Pts',(34.7035440429025,21.7071892844497,0.));
#30092=CARTESIAN_POINT('Ctrl Pts',(34.7035440429025,21.7071892844497,18.));
#30093=CARTESIAN_POINT('Ctrl Pts',(34.7599631530844,21.7893672401137,0.));
#30094=CARTESIAN_POINT('Ctrl Pts',(34.7599631530844,21.7893672401137,18.));
#30095=CARTESIAN_POINT('Ctrl Pts',(34.8159618014436,21.8719971302817,0.));
#30096=CARTESIAN_POINT('Ctrl Pts',(34.8159618014436,21.8719971302817,18.));
#30097=CARTESIAN_POINT('Ctrl Pts',(34.8715413418101,21.9550742217675,0.));
#30098=CARTESIAN_POINT('Ctrl Pts',(34.8715413418101,21.9550742217675,18.));
#30099=CARTESIAN_POINT('Ctrl Pts',(34.9267029879922,22.0385940162683,0.));
#30100=CARTESIAN_POINT('Ctrl Pts',(34.9267029879922,22.0385940162683,18.));
#30101=CARTESIAN_POINT('Ctrl Pts',(34.9814483545602,22.1225514798584,0.));
#30102=CARTESIAN_POINT('Ctrl Pts',(34.9814483545602,22.1225514798584,18.));
#30103=CARTESIAN_POINT('Ctrl Pts',(35.0357795922459,22.2069408519232,0.));
#30104=CARTESIAN_POINT('Ctrl Pts',(35.0357795922459,22.2069408519232,18.));
#30105=CARTESIAN_POINT('Ctrl Pts',(35.0896991159359,22.2917560356803,0.));
#30106=CARTESIAN_POINT('Ctrl Pts',(35.0896991159359,22.2917560356803,18.));
#30107=CARTESIAN_POINT('Ctrl Pts',(35.1432094422642,22.3769908340843,0.));
#30108=CARTESIAN_POINT('Ctrl Pts',(35.1432094422642,22.3769908340843,18.));
#30109=CARTESIAN_POINT('Ctrl Pts',(35.1963130003352,22.4626392230023,0.));
#30110=CARTESIAN_POINT('Ctrl Pts',(35.1963130003352,22.4626392230023,18.));
#30111=CARTESIAN_POINT('Ctrl Pts',(35.2490119207975,22.5486956608909,0.));
#30112=CARTESIAN_POINT('Ctrl Pts',(35.2490119207975,22.5486956608909,18.));
#30113=CARTESIAN_POINT('Ctrl Pts',(35.3013079759252,22.635155167154,0.));
#30114=CARTESIAN_POINT('Ctrl Pts',(35.3013079759252,22.635155167154,18.));
#30115=CARTESIAN_POINT('Ctrl Pts',(35.3532026952313,22.7220131336912,0.));
#30116=CARTESIAN_POINT('Ctrl Pts',(35.3532026952313,22.7220131336912,18.));
#30117=CARTESIAN_POINT('Ctrl Pts',(35.4046974393492,22.8092652000706,0.));
#30118=CARTESIAN_POINT('Ctrl Pts',(35.4046974393492,22.8092652000706,18.));
#30119=CARTESIAN_POINT('Ctrl Pts',(35.4557934871468,22.8969071125089,0.));
#30120=CARTESIAN_POINT('Ctrl Pts',(35.4557934871468,22.8969071125089,18.));
#30121=CARTESIAN_POINT('Ctrl Pts',(35.5064921357308,22.9849345572033,0.));
#30122=CARTESIAN_POINT('Ctrl Pts',(35.5064921357308,22.9849345572033,18.));
#30123=CARTESIAN_POINT('Ctrl Pts',(35.5567947408311,23.0733431097058,0.));
#30124=CARTESIAN_POINT('Ctrl Pts',(35.5567947408311,23.0733431097058,18.));
#30125=CARTESIAN_POINT('Ctrl Pts',(35.6067026687722,23.1621283508111,0.));
#30126=CARTESIAN_POINT('Ctrl Pts',(35.6067026687722,23.1621283508111,18.));
#30127=CARTESIAN_POINT('Ctrl Pts',(35.6562172725207,23.2512859425032,0.));
#30128=CARTESIAN_POINT('Ctrl Pts',(35.6562172725207,23.2512859425032,18.));
#30129=CARTESIAN_POINT('Ctrl Pts',(35.7053398620512,23.3408117088761,0.));
#30130=CARTESIAN_POINT('Ctrl Pts',(35.7053398620512,23.3408117088761,18.));
#30131=CARTESIAN_POINT('Ctrl Pts',(35.7540716771372,23.4307017328227,0.));
#30132=CARTESIAN_POINT('Ctrl Pts',(35.7540716771372,23.4307017328227,18.));
#30133=CARTESIAN_POINT('Ctrl Pts',(35.8024138716897,23.5209523746427,0.));
#30134=CARTESIAN_POINT('Ctrl Pts',(35.8024138716897,23.5209523746427,18.));
#30135=CARTESIAN_POINT('Ctrl Pts',(35.8503675222884,23.611560139948,0.));
#30136=CARTESIAN_POINT('Ctrl Pts',(35.8503675222884,23.611560139948,18.));
#30137=CARTESIAN_POINT('Ctrl Pts',(35.8979336336837,23.7025215735353,0.));
#30138=CARTESIAN_POINT('Ctrl Pts',(35.8979336336837,23.7025215735353,18.));
#30139=CARTESIAN_POINT('Ctrl Pts',(35.9451131482488,23.7938331508737,0.));
#30140=CARTESIAN_POINT('Ctrl Pts',(35.9451131482488,23.7938331508737,18.));
#30141=CARTESIAN_POINT('Ctrl Pts',(35.991906956547,23.8854911428946,0.));
#30142=CARTESIAN_POINT('Ctrl Pts',(35.991906956547,23.8854911428946,18.));
#30143=CARTESIAN_POINT('Ctrl Pts',(36.0383159101253,23.9774915680089,0.));
#30144=CARTESIAN_POINT('Ctrl Pts',(36.0383159101253,23.9774915680089,18.));
#30145=CARTESIAN_POINT('Ctrl Pts',(36.0843408347974,24.0698304230588,0.));
#30146=CARTESIAN_POINT('Ctrl Pts',(36.0843408347974,24.0698304230588,18.));
#30147=CARTESIAN_POINT('Ctrl Pts',(36.1299825471271,24.1625038657964,0.));
#30148=CARTESIAN_POINT('Ctrl Pts',(36.1299825471271,24.1625038657964,18.));
#30149=CARTESIAN_POINT('Ctrl Pts',(36.1752418704833,24.2555084095332,0.));
#30150=CARTESIAN_POINT('Ctrl Pts',(36.1752418704833,24.2555084095332,18.));
#30151=CARTESIAN_POINT('Ctrl Pts',(36.2201196586696,24.3488411214068,0.));
#30152=CARTESIAN_POINT('Ctrl Pts',(36.2201196586696,24.3488411214068,18.));
#30153=CARTESIAN_POINT('Ctrl Pts',(36.2646168058395,24.4424997853604,0.));
#30154=CARTESIAN_POINT('Ctrl Pts',(36.2646168058395,24.4424997853604,18.));
#30155=CARTESIAN_POINT('Ctrl Pts',(36.308734152297,24.5364828082556,0.));
#30156=CARTESIAN_POINT('Ctrl Pts',(36.308734152297,24.5364828082556,18.));
#30157=CARTESIAN_POINT('Ctrl Pts',(36.3437247532368,24.6119278836614,0.));
#30158=CARTESIAN_POINT('Ctrl Pts',(36.3437247532368,24.6119278836614,18.));
#30159=CARTESIAN_POINT('Ctrl Pts',(36.369797330215,24.6686569322616,0.));
#30160=CARTESIAN_POINT('Ctrl Pts',(36.369797330215,24.6686569322616,18.));
#30161=CARTESIAN_POINT('Ctrl Pts',(36.3871033517098,24.7065408286023,0.));
#30162=CARTESIAN_POINT('Ctrl Pts',(36.3871033517098,24.7065408286023,18.));
#30163=CARTESIAN_POINT('Ctrl Pts',(36.3957374383337,24.725498909423,0.));
#30164=CARTESIAN_POINT('Ctrl Pts',(36.3957374383337,24.725498909423,18.));
#30165=CARTESIAN_POINT('Ctrl Pts',(32.3379313568208,19.1596907609891,0.));
#30166=CARTESIAN_POINT('Ctrl Pts',(32.3542491343753,19.1693587749508,0.));
#30167=CARTESIAN_POINT('Ctrl Pts',(32.3866012518553,19.1891139208368,0.));
#30168=CARTESIAN_POINT('Ctrl Pts',(32.4342791270009,19.2200039764927,0.));
#30169=CARTESIAN_POINT('Ctrl Pts',(32.4962340238036,19.2635813403783,0.));
#30170=CARTESIAN_POINT('Ctrl Pts',(32.5714771007861,19.3213180490743,0.));
#30171=CARTESIAN_POINT('Ctrl Pts',(32.6451434870609,19.381405831319,0.));
#30172=CARTESIAN_POINT('Ctrl Pts',(32.7178463324062,19.4429429601189,0.));
#30173=CARTESIAN_POINT('Ctrl Pts',(32.7900335943248,19.5052640847974,0.));
#30174=CARTESIAN_POINT('Ctrl Pts',(32.8618672807884,19.5681157030437,0.));
#30175=CARTESIAN_POINT('Ctrl Pts',(32.9333211533788,19.6315161742485,0.));
#30176=CARTESIAN_POINT('Ctrl Pts',(33.004256563411,19.6956473461873,0.));
#30177=CARTESIAN_POINT('Ctrl Pts',(33.0745026283418,19.7607398248651,0.));
#30178=CARTESIAN_POINT('Ctrl Pts',(33.1439436707661,19.8269479776239,0.));
#30179=CARTESIAN_POINT('Ctrl Pts',(33.2125746879471,19.8942704458546,0.));
#30180=CARTESIAN_POINT('Ctrl Pts',(33.2804560993213,19.9626141625205,0.));
#30181=CARTESIAN_POINT('Ctrl Pts',(33.3476854048385,20.0318342617212,0.));
#30182=CARTESIAN_POINT('Ctrl Pts',(33.4143643679979,20.1017803986381,0.));
#30183=CARTESIAN_POINT('Ctrl Pts',(33.480563024813,20.1723475154533,0.));
#30184=CARTESIAN_POINT('Ctrl Pts',(33.5463023319603,20.243500298383,0.));
#30185=CARTESIAN_POINT('Ctrl Pts',(33.6115742164079,20.3152448035298,0.));
#30186=CARTESIAN_POINT('Ctrl Pts',(33.6763537716992,20.3876111773341,0.));
#30187=CARTESIAN_POINT('Ctrl Pts',(33.7406135254082,20.4606334536183,0.));
#30188=CARTESIAN_POINT('Ctrl Pts',(33.8043393734971,20.5343269914034,0.));
#30189=CARTESIAN_POINT('Ctrl Pts',(33.8675365150454,20.6086800574386,0.));
#30190=CARTESIAN_POINT('Ctrl Pts',(33.9302209962425,20.683665762903,0.));
#30191=CARTESIAN_POINT('Ctrl Pts',(33.9924146647395,20.7592491770603,0.));
#30192=CARTESIAN_POINT('Ctrl Pts',(34.0541392299678,20.8353957068415,0.));
#30193=CARTESIAN_POINT('Ctrl Pts',(34.1154095510973,20.9120805673809,0.));
#30194=CARTESIAN_POINT('Ctrl Pts',(34.176231731809,20.9892914622612,0.));
#30195=CARTESIAN_POINT('Ctrl Pts',(34.2366067284279,21.0670234747355,0.));
#30196=CARTESIAN_POINT('Ctrl Pts',(34.2965325673384,21.1452759244399,0.));
#30197=CARTESIAN_POINT('Ctrl Pts',(34.3560069185815,21.2240487218079,0.));
#30198=CARTESIAN_POINT('Ctrl Pts',(34.4150300340623,21.3033382073239,0.));
#30199=CARTESIAN_POINT('Ctrl Pts',(34.4736054662052,21.3831361300104,0.));
#30200=CARTESIAN_POINT('Ctrl Pts',(34.5317385658329,21.4634317666005,0.));
#30201=CARTESIAN_POINT('Ctrl Pts',(34.5894355639082,21.5442132160757,0.));
#30202=CARTESIAN_POINT('Ctrl Pts',(34.6467025072367,21.6254689009796,0.));
#30203=CARTESIAN_POINT('Ctrl Pts',(34.7035440429025,21.7071892844497,0.));
#30204=CARTESIAN_POINT('Ctrl Pts',(34.7599631530844,21.7893672401137,0.));
#30205=CARTESIAN_POINT('Ctrl Pts',(34.8159618014436,21.8719971302817,0.));
#30206=CARTESIAN_POINT('Ctrl Pts',(34.8715413418101,21.9550742217675,0.));
#30207=CARTESIAN_POINT('Ctrl Pts',(34.9267029879922,22.0385940162683,0.));
#30208=CARTESIAN_POINT('Ctrl Pts',(34.9814483545602,22.1225514798584,0.));
#30209=CARTESIAN_POINT('Ctrl Pts',(35.0357795922459,22.2069408519232,0.));
#30210=CARTESIAN_POINT('Ctrl Pts',(35.0896991159359,22.2917560356803,0.));
#30211=CARTESIAN_POINT('Ctrl Pts',(35.1432094422642,22.3769908340843,0.));
#30212=CARTESIAN_POINT('Ctrl Pts',(35.1963130003352,22.4626392230023,0.));
#30213=CARTESIAN_POINT('Ctrl Pts',(35.2490119207975,22.5486956608909,0.));
#30214=CARTESIAN_POINT('Ctrl Pts',(35.3013079759252,22.635155167154,0.));
#30215=CARTESIAN_POINT('Ctrl Pts',(35.3532026952313,22.7220131336912,0.));
#30216=CARTESIAN_POINT('Ctrl Pts',(35.4046974393492,22.8092652000706,0.));
#30217=CARTESIAN_POINT('Ctrl Pts',(35.4557934871468,22.8969071125089,0.));
#30218=CARTESIAN_POINT('Ctrl Pts',(35.5064921357308,22.9849345572033,0.));
#30219=CARTESIAN_POINT('Ctrl Pts',(35.5567947408311,23.0733431097058,0.));
#30220=CARTESIAN_POINT('Ctrl Pts',(35.6067026687722,23.1621283508111,0.));
#30221=CARTESIAN_POINT('Ctrl Pts',(35.6562172725207,23.2512859425032,0.));
#30222=CARTESIAN_POINT('Ctrl Pts',(35.7053398620512,23.3408117088761,0.));
#30223=CARTESIAN_POINT('Ctrl Pts',(35.7540716771372,23.4307017328227,0.));
#30224=CARTESIAN_POINT('Ctrl Pts',(35.8024138716897,23.5209523746427,0.));
#30225=CARTESIAN_POINT('Ctrl Pts',(35.8503675222884,23.611560139948,0.));
#30226=CARTESIAN_POINT('Ctrl Pts',(35.8979336336837,23.7025215735353,0.));
#30227=CARTESIAN_POINT('Ctrl Pts',(35.9451131482488,23.7938331508737,0.));
#30228=CARTESIAN_POINT('Ctrl Pts',(35.991906956547,23.8854911428946,0.));
#30229=CARTESIAN_POINT('Ctrl Pts',(36.0383159101253,23.9774915680089,0.));
#30230=CARTESIAN_POINT('Ctrl Pts',(36.0843408347974,24.0698304230588,0.));
#30231=CARTESIAN_POINT('Ctrl Pts',(36.1299825471271,24.1625038657964,0.));
#30232=CARTESIAN_POINT('Ctrl Pts',(36.1752418704833,24.2555084095332,0.));
#30233=CARTESIAN_POINT('Ctrl Pts',(36.2201196586696,24.3488411214068,0.));
#30234=CARTESIAN_POINT('Ctrl Pts',(36.2735162352735,24.4612315181511,0.));
#30235=CARTESIAN_POINT('Ctrl Pts',(36.3175386315529,24.5552956307817,0.));
#30236=CARTESIAN_POINT('Ctrl Pts',(36.3524534604648,24.630805301288,0.));
#30237=CARTESIAN_POINT('Ctrl Pts',(36.3784692650901,24.6875827477484,0.));
#30238=CARTESIAN_POINT('Ctrl Pts',(36.3957374383337,24.725498909423,0.));
#30239=CARTESIAN_POINT('Ctrl Pts',(32.3379313568208,19.1596907609891,15.));
#30240=CARTESIAN_POINT('Ctrl Pts',(32.3542491343753,19.1693587749508,15.));
#30241=CARTESIAN_POINT('Ctrl Pts',(32.3866012518553,19.1891139208368,15.));
#30242=CARTESIAN_POINT('Ctrl Pts',(32.4342791270009,19.2200039764927,15.));
#30243=CARTESIAN_POINT('Ctrl Pts',(32.4962340238036,19.2635813403783,15.));
#30244=CARTESIAN_POINT('Ctrl Pts',(32.5714771007861,19.3213180490743,15.));
#30245=CARTESIAN_POINT('Ctrl Pts',(32.6451434870609,19.381405831319,15.));
#30246=CARTESIAN_POINT('Ctrl Pts',(32.7178463324062,19.4429429601189,15.));
#30247=CARTESIAN_POINT('Ctrl Pts',(32.7900335943248,19.5052640847974,15.));
#30248=CARTESIAN_POINT('Ctrl Pts',(32.8618672807884,19.5681157030437,15.));
#30249=CARTESIAN_POINT('Ctrl Pts',(32.9333211533788,19.6315161742485,15.));
#30250=CARTESIAN_POINT('Ctrl Pts',(33.004256563411,19.6956473461873,15.));
#30251=CARTESIAN_POINT('Ctrl Pts',(33.0745026283418,19.7607398248651,15.));
#30252=CARTESIAN_POINT('Ctrl Pts',(33.1439436707661,19.8269479776239,15.));
#30253=CARTESIAN_POINT('Ctrl Pts',(33.2125746879471,19.8942704458546,15.));
#30254=CARTESIAN_POINT('Ctrl Pts',(33.2804560993213,19.9626141625205,15.));
#30255=CARTESIAN_POINT('Ctrl Pts',(33.3476854048385,20.0318342617212,15.));
#30256=CARTESIAN_POINT('Ctrl Pts',(33.4143643679979,20.1017803986381,15.));
#30257=CARTESIAN_POINT('Ctrl Pts',(33.480563024813,20.1723475154533,15.));
#30258=CARTESIAN_POINT('Ctrl Pts',(33.5463023319603,20.243500298383,15.));
#30259=CARTESIAN_POINT('Ctrl Pts',(33.6115742164079,20.3152448035298,15.));
#30260=CARTESIAN_POINT('Ctrl Pts',(33.6763537716992,20.3876111773341,15.));
#30261=CARTESIAN_POINT('Ctrl Pts',(33.7406135254082,20.4606334536183,15.));
#30262=CARTESIAN_POINT('Ctrl Pts',(33.8043393734971,20.5343269914034,15.));
#30263=CARTESIAN_POINT('Ctrl Pts',(33.8675365150454,20.6086800574386,15.));
#30264=CARTESIAN_POINT('Ctrl Pts',(33.9302209962425,20.683665762903,15.));
#30265=CARTESIAN_POINT('Ctrl Pts',(33.9924146647395,20.7592491770603,15.));
#30266=CARTESIAN_POINT('Ctrl Pts',(34.0541392299678,20.8353957068415,15.));
#30267=CARTESIAN_POINT('Ctrl Pts',(34.1154095510973,20.9120805673809,15.));
#30268=CARTESIAN_POINT('Ctrl Pts',(34.176231731809,20.9892914622612,15.));
#30269=CARTESIAN_POINT('Ctrl Pts',(34.2366067284279,21.0670234747355,15.));
#30270=CARTESIAN_POINT('Ctrl Pts',(34.2965325673384,21.1452759244399,15.));
#30271=CARTESIAN_POINT('Ctrl Pts',(34.3560069185815,21.2240487218079,15.));
#30272=CARTESIAN_POINT('Ctrl Pts',(34.4150300340623,21.3033382073239,15.));
#30273=CARTESIAN_POINT('Ctrl Pts',(34.4736054662052,21.3831361300104,15.));
#30274=CARTESIAN_POINT('Ctrl Pts',(34.5317385658329,21.4634317666005,15.));
#30275=CARTESIAN_POINT('Ctrl Pts',(34.5894355639082,21.5442132160757,15.));
#30276=CARTESIAN_POINT('Ctrl Pts',(34.6467025072367,21.6254689009796,15.));
#30277=CARTESIAN_POINT('Ctrl Pts',(34.7035440429025,21.7071892844497,15.));
#30278=CARTESIAN_POINT('Ctrl Pts',(34.7599631530844,21.7893672401137,15.));
#30279=CARTESIAN_POINT('Ctrl Pts',(34.8159618014436,21.8719971302817,15.));
#30280=CARTESIAN_POINT('Ctrl Pts',(34.8715413418101,21.9550742217675,15.));
#30281=CARTESIAN_POINT('Ctrl Pts',(34.9267029879922,22.0385940162683,15.));
#30282=CARTESIAN_POINT('Ctrl Pts',(34.9814483545602,22.1225514798584,15.));
#30283=CARTESIAN_POINT('Ctrl Pts',(35.0357795922459,22.2069408519232,15.));
#30284=CARTESIAN_POINT('Ctrl Pts',(35.0896991159359,22.2917560356803,15.));
#30285=CARTESIAN_POINT('Ctrl Pts',(35.1432094422642,22.3769908340843,15.));
#30286=CARTESIAN_POINT('Ctrl Pts',(35.1963130003352,22.4626392230023,15.));
#30287=CARTESIAN_POINT('Ctrl Pts',(35.2490119207975,22.5486956608909,15.));
#30288=CARTESIAN_POINT('Ctrl Pts',(35.3013079759252,22.635155167154,15.));
#30289=CARTESIAN_POINT('Ctrl Pts',(35.3532026952313,22.7220131336912,15.));
#30290=CARTESIAN_POINT('Ctrl Pts',(35.4046974393492,22.8092652000706,15.));
#30291=CARTESIAN_POINT('Ctrl Pts',(35.4557934871468,22.8969071125089,15.));
#30292=CARTESIAN_POINT('Ctrl Pts',(35.5064921357308,22.9849345572033,15.));
#30293=CARTESIAN_POINT('Ctrl Pts',(35.5567947408311,23.0733431097058,15.));
#30294=CARTESIAN_POINT('Ctrl Pts',(35.6067026687722,23.1621283508111,15.));
#30295=CARTESIAN_POINT('Ctrl Pts',(35.6562172725207,23.2512859425032,15.));
#30296=CARTESIAN_POINT('Ctrl Pts',(35.7053398620512,23.3408117088761,15.));
#30297=CARTESIAN_POINT('Ctrl Pts',(35.7540716771372,23.4307017328227,15.));
#30298=CARTESIAN_POINT('Ctrl Pts',(35.8024138716897,23.5209523746427,15.));
#30299=CARTESIAN_POINT('Ctrl Pts',(35.8503675222884,23.611560139948,15.));
#30300=CARTESIAN_POINT('Ctrl Pts',(35.8979336336837,23.7025215735353,15.));
#30301=CARTESIAN_POINT('Ctrl Pts',(35.9451131482488,23.7938331508737,15.));
#30302=CARTESIAN_POINT('Ctrl Pts',(35.991906956547,23.8854911428946,15.));
#30303=CARTESIAN_POINT('Ctrl Pts',(36.0383159101253,23.9774915680089,15.));
#30304=CARTESIAN_POINT('Ctrl Pts',(36.0843408347974,24.0698304230588,15.));
#30305=CARTESIAN_POINT('Ctrl Pts',(36.1299825471271,24.1625038657964,15.));
#30306=CARTESIAN_POINT('Ctrl Pts',(36.1752418704833,24.2555084095332,15.));
#30307=CARTESIAN_POINT('Ctrl Pts',(36.2201196586696,24.3488411214068,15.));
#30308=CARTESIAN_POINT('Ctrl Pts',(36.2735162352735,24.4612315181511,15.));
#30309=CARTESIAN_POINT('Ctrl Pts',(36.3175386315529,24.5552956307817,15.));
#30310=CARTESIAN_POINT('Ctrl Pts',(36.3524534604648,24.630805301288,15.));
#30311=CARTESIAN_POINT('Ctrl Pts',(36.3784692650901,24.6875827477484,15.));
#30312=CARTESIAN_POINT('Ctrl Pts',(36.3957374383337,24.725498909423,15.));
#30313=CARTESIAN_POINT('Ctrl Pts',(41.396226524684,14.911486495888,0.));
#30314=CARTESIAN_POINT('Ctrl Pts',(41.396226524684,14.911486495888,18.));
#30315=CARTESIAN_POINT('Ctrl Pts',(41.3758141263348,14.9156446533966,0.));
#30316=CARTESIAN_POINT('Ctrl Pts',(41.3758141263348,14.9156446533966,18.));
#30317=CARTESIAN_POINT('Ctrl Pts',(41.3349931861715,14.9239113834707,0.));
#30318=CARTESIAN_POINT('Ctrl Pts',(41.3349931861715,14.9239113834707,18.));
#30319=CARTESIAN_POINT('Ctrl Pts',(41.2737733455422,14.936162723752,0.));
#30320=CARTESIAN_POINT('Ctrl Pts',(41.2737733455422,14.936162723752,18.));
#30321=CARTESIAN_POINT('Ctrl Pts',(41.1921700381957,14.9522002356298,0.));
#30322=CARTESIAN_POINT('Ctrl Pts',(41.1921700381957,14.9522002356298,18.));
#30323=CARTESIAN_POINT('Ctrl Pts',(41.0902046498729,14.9717503874227,0.));
#30324=CARTESIAN_POINT('Ctrl Pts',(41.0902046498729,14.9717503874227,18.));
#30325=CARTESIAN_POINT('Ctrl Pts',(40.9882784321884,14.9908026205824,0.));
#30326=CARTESIAN_POINT('Ctrl Pts',(40.9882784321884,14.9908026205824,18.));
#30327=CARTESIAN_POINT('Ctrl Pts',(40.8863921801,15.0093553188655,0.));
#30328=CARTESIAN_POINT('Ctrl Pts',(40.8863921801,15.0093553188655,18.));
#30329=CARTESIAN_POINT('Ctrl Pts',(40.7845471608654,15.0274064563211,0.));
#30330=CARTESIAN_POINT('Ctrl Pts',(40.7845471608654,15.0274064563211,18.));
#30331=CARTESIAN_POINT('Ctrl Pts',(40.6827452453667,15.0449536183143,0.));
#30332=CARTESIAN_POINT('Ctrl Pts',(40.6827452453667,15.0449536183143,18.));
#30333=CARTESIAN_POINT('Ctrl Pts',(40.58098877043,15.0619940893017,0.));
#30334=CARTESIAN_POINT('Ctrl Pts',(40.58098877043,15.0619940893017,18.));
#30335=CARTESIAN_POINT('Ctrl Pts',(40.4792803645352,15.0785249502524,0.));
#30336=CARTESIAN_POINT('Ctrl Pts',(40.4792803645352,15.0785249502524,18.));
#30337=CARTESIAN_POINT('Ctrl Pts',(40.3776227809037,15.0945431800723,0.));
#30338=CARTESIAN_POINT('Ctrl Pts',(40.3776227809037,15.0945431800723,18.));
#30339=CARTESIAN_POINT('Ctrl Pts',(40.2760187401821,15.1100457495259,0.));
#30340=CARTESIAN_POINT('Ctrl Pts',(40.2760187401821,15.1100457495259,18.));
#30341=CARTESIAN_POINT('Ctrl Pts',(40.1744707357902,15.1250297462408,0.));
#30342=CARTESIAN_POINT('Ctrl Pts',(40.1744707357902,15.1250297462408,18.));
#30343=CARTESIAN_POINT('Ctrl Pts',(40.0729810652204,15.1394923361537,0.));
#30344=CARTESIAN_POINT('Ctrl Pts',(40.0729810652204,15.1394923361537,18.));
#30345=CARTESIAN_POINT('Ctrl Pts',(39.9715519332134,15.1534306754871,0.));
#30346=CARTESIAN_POINT('Ctrl Pts',(39.9715519332134,15.1534306754871,18.));
#30347=CARTESIAN_POINT('Ctrl Pts',(39.8701855339908,15.1668418393198,0.));
#30348=CARTESIAN_POINT('Ctrl Pts',(39.8701855339908,15.1668418393198,18.));
#30349=CARTESIAN_POINT('Ctrl Pts',(39.7688841338802,15.1797227547561,0.));
#30350=CARTESIAN_POINT('Ctrl Pts',(39.7688841338802,15.1797227547561,18.));
#30351=CARTESIAN_POINT('Ctrl Pts',(39.6676501731673,15.1920701163803,0.));
#30352=CARTESIAN_POINT('Ctrl Pts',(39.6676501731673,15.1920701163803,18.));
#30353=CARTESIAN_POINT('Ctrl Pts',(39.5664862602472,15.2038804098649,0.));
#30354=CARTESIAN_POINT('Ctrl Pts',(39.5664862602472,15.2038804098649,18.));
#30355=CARTESIAN_POINT('Ctrl Pts',(39.4653951093947,15.2151499908149,0.));
#30356=CARTESIAN_POINT('Ctrl Pts',(39.4653951093947,15.2151499908149,18.));
#30357=CARTESIAN_POINT('Ctrl Pts',(39.3643794927167,15.225875156307,0.));
#30358=CARTESIAN_POINT('Ctrl Pts',(39.3643794927167,15.225875156307,18.));
#30359=CARTESIAN_POINT('Ctrl Pts',(39.2634421927888,15.2360522089072,0.));
#30360=CARTESIAN_POINT('Ctrl Pts',(39.2634421927888,15.2360522089072,18.));
#30361=CARTESIAN_POINT('Ctrl Pts',(39.1625859371304,15.2456775636447,0.));
#30362=CARTESIAN_POINT('Ctrl Pts',(39.1625859371304,15.2456775636447,18.));
#30363=CARTESIAN_POINT('Ctrl Pts',(39.061813415425,15.2547476855825,0.));
#30364=CARTESIAN_POINT('Ctrl Pts',(39.061813415425,15.2547476855825,18.));
#30365=CARTESIAN_POINT('Ctrl Pts',(38.9611273555758,15.2632589109473,0.));
#30366=CARTESIAN_POINT('Ctrl Pts',(38.9611273555758,15.2632589109473,18.));
#30367=CARTESIAN_POINT('Ctrl Pts',(38.860530586589,15.2712072937639,0.));
#30368=CARTESIAN_POINT('Ctrl Pts',(38.860530586589,15.2712072937639,18.));
#30369=CARTESIAN_POINT('Ctrl Pts',(38.7600260961351,15.2785884727112,0.));
#30370=CARTESIAN_POINT('Ctrl Pts',(38.7600260961351,15.2785884727112,18.));
#30371=CARTESIAN_POINT('Ctrl Pts',(38.659617115053,15.2853974668211,0.));
#30372=CARTESIAN_POINT('Ctrl Pts',(38.659617115053,15.2853974668211,18.));
#30373=CARTESIAN_POINT('Ctrl Pts',(38.5593070891769,15.2916287700102,0.));
#30374=CARTESIAN_POINT('Ctrl Pts',(38.5593070891769,15.2916287700102,18.));
#30375=CARTESIAN_POINT('Ctrl Pts',(38.4590995527814,15.2972767037469,0.));
#30376=CARTESIAN_POINT('Ctrl Pts',(38.4590995527814,15.2972767037469,18.));
#30377=CARTESIAN_POINT('Ctrl Pts',(38.3589980188324,15.3023357307483,0.));
#30378=CARTESIAN_POINT('Ctrl Pts',(38.3589980188324,15.3023357307483,18.));
#30379=CARTESIAN_POINT('Ctrl Pts',(38.2590058835965,15.3068007250314,0.));
#30380=CARTESIAN_POINT('Ctrl Pts',(38.2590058835965,15.3068007250314,18.));
#30381=CARTESIAN_POINT('Ctrl Pts',(38.1591262705847,15.310667421514,0.));
#30382=CARTESIAN_POINT('Ctrl Pts',(38.1591262705847,15.310667421514,18.));
#30383=CARTESIAN_POINT('Ctrl Pts',(38.0593621055415,15.3139321941687,0.));
#30384=CARTESIAN_POINT('Ctrl Pts',(38.0593621055415,15.3139321941687,18.));
#30385=CARTESIAN_POINT('Ctrl Pts',(37.959716421934,15.3165911656268,0.));
#30386=CARTESIAN_POINT('Ctrl Pts',(37.959716421934,15.3165911656268,18.));
#30387=CARTESIAN_POINT('Ctrl Pts',(37.8601926265378,15.3186394335023,0.));
#30388=CARTESIAN_POINT('Ctrl Pts',(37.8601926265378,15.3186394335023,18.));
#30389=CARTESIAN_POINT('Ctrl Pts',(37.7607947318286,15.320070396385,0.));
#30390=CARTESIAN_POINT('Ctrl Pts',(37.7607947318286,15.320070396385,18.));
#30391=CARTESIAN_POINT('Ctrl Pts',(37.6615277218027,15.320874689078,0.));
#30392=CARTESIAN_POINT('Ctrl Pts',(37.6615277218027,15.320874689078,18.));
#30393=CARTESIAN_POINT('Ctrl Pts',(37.562397408596,15.3210406145546,0.));
#30394=CARTESIAN_POINT('Ctrl Pts',(37.562397408596,15.3210406145546,18.));
#30395=CARTESIAN_POINT('Ctrl Pts',(37.4634097578665,15.3205561366169,0.));
#30396=CARTESIAN_POINT('Ctrl Pts',(37.4634097578665,15.3205561366169,18.));
#30397=CARTESIAN_POINT('Ctrl Pts',(37.3645702997848,15.3194106233801,0.));
#30398=CARTESIAN_POINT('Ctrl Pts',(37.3645702997848,15.3194106233801,18.));
#30399=CARTESIAN_POINT('Ctrl Pts',(37.2658836214694,15.3175963510698,0.));
#30400=CARTESIAN_POINT('Ctrl Pts',(37.2658836214694,15.3175963510698,18.));
#30401=CARTESIAN_POINT('Ctrl Pts',(37.1673525354642,15.3151109648809,0.));
#30402=CARTESIAN_POINT('Ctrl Pts',(37.1673525354642,15.3151109648809,18.));
#30403=CARTESIAN_POINT('Ctrl Pts',(37.0689784837457,15.3119562971444,0.));
#30404=CARTESIAN_POINT('Ctrl Pts',(37.0689784837457,15.3119562971444,18.));
#30405=CARTESIAN_POINT('Ctrl Pts',(36.970763176802,15.3081335446406,0.));
#30406=CARTESIAN_POINT('Ctrl Pts',(36.970763176802,15.3081335446406,18.));
#30407=CARTESIAN_POINT('Ctrl Pts',(36.8727100302512,15.3036390436952,0.));
#30408=CARTESIAN_POINT('Ctrl Pts',(36.8727100302512,15.3036390436952,18.));
#30409=CARTESIAN_POINT('Ctrl Pts',(36.7748254044502,15.2984606286737,0.));
#30410=CARTESIAN_POINT('Ctrl Pts',(36.7748254044502,15.2984606286737,18.));
#30411=CARTESIAN_POINT('Ctrl Pts',(36.6771206167755,15.2925717100767,0.));
#30412=CARTESIAN_POINT('Ctrl Pts',(36.6771206167755,15.2925717100767,18.));
#30413=CARTESIAN_POINT('Ctrl Pts',(36.5796108931244,15.2859343913094,0.));
#30414=CARTESIAN_POINT('Ctrl Pts',(36.5796108931244,15.2859343913094,18.));
#30415=CARTESIAN_POINT('Ctrl Pts',(36.4823116513289,15.2785104654792,0.));
#30416=CARTESIAN_POINT('Ctrl Pts',(36.4823116513289,15.2785104654792,18.));
#30417=CARTESIAN_POINT('Ctrl Pts',(36.3852352131887,15.2702711460937,0.));
#30418=CARTESIAN_POINT('Ctrl Pts',(36.3852352131887,15.2702711460937,18.));
#30419=CARTESIAN_POINT('Ctrl Pts',(36.2883880151607,15.2612053303773,0.));
#30420=CARTESIAN_POINT('Ctrl Pts',(36.2883880151607,15.2612053303773,18.));
#30421=CARTESIAN_POINT('Ctrl Pts',(36.1917659216814,15.2513334565427,0.));
#30422=CARTESIAN_POINT('Ctrl Pts',(36.1917659216814,15.2513334565427,18.));
#30423=CARTESIAN_POINT('Ctrl Pts',(36.095357546697,15.240697754828,0.));
#30424=CARTESIAN_POINT('Ctrl Pts',(36.095357546697,15.240697754828,18.));
#30425=CARTESIAN_POINT('Ctrl Pts',(35.9991531408727,15.2293360946131,0.));
#30426=CARTESIAN_POINT('Ctrl Pts',(35.9991531408727,15.2293360946131,18.));
#30427=CARTESIAN_POINT('Ctrl Pts',(35.9031525499277,15.2172585668056,0.));
#30428=CARTESIAN_POINT('Ctrl Pts',(35.9031525499277,15.2172585668056,18.));
#30429=CARTESIAN_POINT('Ctrl Pts',(35.8073720252878,15.2044274601769,0.));
#30430=CARTESIAN_POINT('Ctrl Pts',(35.8073720252878,15.2044274601769,18.));
#30431=CARTESIAN_POINT('Ctrl Pts',(35.7118553943773,15.1907243629659,0.));
#30432=CARTESIAN_POINT('Ctrl Pts',(35.7118553943773,15.1907243629659,18.));
#30433=CARTESIAN_POINT('Ctrl Pts',(35.6166644736253,15.1759785763051,0.));
#30434=CARTESIAN_POINT('Ctrl Pts',(35.6166644736253,15.1759785763051,18.));
#30435=CARTESIAN_POINT('Ctrl Pts',(35.5218591529745,15.1600260710384,0.));
#30436=CARTESIAN_POINT('Ctrl Pts',(35.5218591529745,15.1600260710384,18.));
#30437=CARTESIAN_POINT('Ctrl Pts',(35.4274792115856,15.1427632633831,0.));
#30438=CARTESIAN_POINT('Ctrl Pts',(35.4274792115856,15.1427632633831,18.));
#30439=CARTESIAN_POINT('Ctrl Pts',(35.3335286891314,15.1241934020681,0.));
#30440=CARTESIAN_POINT('Ctrl Pts',(35.3335286891314,15.1241934020681,18.));
#30441=CARTESIAN_POINT('Ctrl Pts',(35.2399506932815,15.104500806927,0.));
#30442=CARTESIAN_POINT('Ctrl Pts',(35.2399506932815,15.104500806927,18.));
#30443=CARTESIAN_POINT('Ctrl Pts',(35.1466591020976,15.08395927165,0.));
#30444=CARTESIAN_POINT('Ctrl Pts',(35.1466591020976,15.08395927165,18.));
#30445=CARTESIAN_POINT('Ctrl Pts',(35.0535882932913,15.0627878528202,0.));
#30446=CARTESIAN_POINT('Ctrl Pts',(35.0535882932913,15.0627878528202,18.));
#30447=CARTESIAN_POINT('Ctrl Pts',(34.9607388363587,15.041018569143,0.));
#30448=CARTESIAN_POINT('Ctrl Pts',(34.9607388363587,15.041018569143,18.));
#30449=CARTESIAN_POINT('Ctrl Pts',(34.8682205930809,15.0183713484962,0.));
#30450=CARTESIAN_POINT('Ctrl Pts',(34.8682205930809,15.0183713484962,18.));
#30451=CARTESIAN_POINT('Ctrl Pts',(34.7763085406486,14.9940927023322,0.));
#30452=CARTESIAN_POINT('Ctrl Pts',(34.7763085406486,14.9940927023322,18.));
#30453=CARTESIAN_POINT('Ctrl Pts',(34.6853717911268,14.9671565602316,0.));
#30454=CARTESIAN_POINT('Ctrl Pts',(34.6853717911268,14.9671565602316,18.));
#30455=CARTESIAN_POINT('Ctrl Pts',(34.6137007885254,14.9426481276593,0.));
#30456=CARTESIAN_POINT('Ctrl Pts',(34.6137007885254,14.9426481276593,18.));
#30457=CARTESIAN_POINT('Ctrl Pts',(34.5606858566713,14.9222326355678,0.));
#30458=CARTESIAN_POINT('Ctrl Pts',(34.5606858566713,14.9222326355678,18.));
#30459=CARTESIAN_POINT('Ctrl Pts',(34.525687510388,14.9076710061311,0.));
#30460=CARTESIAN_POINT('Ctrl Pts',(34.525687510388,14.9076710061311,18.));
#30461=CARTESIAN_POINT('Ctrl Pts',(34.5082745737944,14.9001523628048,0.));
#30462=CARTESIAN_POINT('Ctrl Pts',(34.5082745737944,14.9001523628048,18.));
#30463=CARTESIAN_POINT('',(41.3962265246839,14.9114864958881,0.));
#30464=CARTESIAN_POINT('Ctrl Pts',(34.5082745737944,14.9001523628048,0.));
#30465=CARTESIAN_POINT('Ctrl Pts',(34.525687510388,14.9076710061311,0.));
#30466=CARTESIAN_POINT('Ctrl Pts',(34.5606858566713,14.9222326355678,0.));
#30467=CARTESIAN_POINT('Ctrl Pts',(34.6137007885254,14.9426481276593,0.));
#30468=CARTESIAN_POINT('Ctrl Pts',(34.6853717911268,14.9671565602316,0.));
#30469=CARTESIAN_POINT('Ctrl Pts',(34.7763085406486,14.9940927023322,0.));
#30470=CARTESIAN_POINT('Ctrl Pts',(34.8682205930809,15.0183713484962,0.));
#30471=CARTESIAN_POINT('Ctrl Pts',(34.9607388363587,15.041018569143,0.));
#30472=CARTESIAN_POINT('Ctrl Pts',(35.0535882932913,15.0627878528202,0.));
#30473=CARTESIAN_POINT('Ctrl Pts',(35.1466591020976,15.08395927165,0.));
#30474=CARTESIAN_POINT('Ctrl Pts',(35.2399506932815,15.104500806927,0.));
#30475=CARTESIAN_POINT('Ctrl Pts',(35.3335286891314,15.1241934020681,0.));
#30476=CARTESIAN_POINT('Ctrl Pts',(35.4274792115856,15.1427632633831,0.));
#30477=CARTESIAN_POINT('Ctrl Pts',(35.5218591529745,15.1600260710384,0.));
#30478=CARTESIAN_POINT('Ctrl Pts',(35.6166644736253,15.1759785763051,0.));
#30479=CARTESIAN_POINT('Ctrl Pts',(35.7118553943773,15.1907243629659,0.));
#30480=CARTESIAN_POINT('Ctrl Pts',(35.8073720252878,15.2044274601769,0.));
#30481=CARTESIAN_POINT('Ctrl Pts',(35.9031525499277,15.2172585668056,0.));
#30482=CARTESIAN_POINT('Ctrl Pts',(35.9991531408727,15.2293360946131,0.));
#30483=CARTESIAN_POINT('Ctrl Pts',(36.095357546697,15.240697754828,0.));
#30484=CARTESIAN_POINT('Ctrl Pts',(36.1917659216814,15.2513334565427,0.));
#30485=CARTESIAN_POINT('Ctrl Pts',(36.2883880151607,15.2612053303773,0.));
#30486=CARTESIAN_POINT('Ctrl Pts',(36.3852352131887,15.2702711460937,0.));
#30487=CARTESIAN_POINT('Ctrl Pts',(36.4823116513289,15.2785104654792,0.));
#30488=CARTESIAN_POINT('Ctrl Pts',(36.5796108931244,15.2859343913094,0.));
#30489=CARTESIAN_POINT('Ctrl Pts',(36.6771206167755,15.2925717100767,0.));
#30490=CARTESIAN_POINT('Ctrl Pts',(36.7748254044502,15.2984606286737,0.));
#30491=CARTESIAN_POINT('Ctrl Pts',(36.8727100302512,15.3036390436952,0.));
#30492=CARTESIAN_POINT('Ctrl Pts',(36.970763176802,15.3081335446406,0.));
#30493=CARTESIAN_POINT('Ctrl Pts',(37.0689784837457,15.3119562971444,0.));
#30494=CARTESIAN_POINT('Ctrl Pts',(37.1673525354642,15.3151109648809,0.));
#30495=CARTESIAN_POINT('Ctrl Pts',(37.2658836214694,15.3175963510698,0.));
#30496=CARTESIAN_POINT('Ctrl Pts',(37.3645702997848,15.3194106233801,0.));
#30497=CARTESIAN_POINT('Ctrl Pts',(37.4634097578665,15.3205561366169,0.));
#30498=CARTESIAN_POINT('Ctrl Pts',(37.562397408596,15.3210406145546,0.));
#30499=CARTESIAN_POINT('Ctrl Pts',(37.6615277218027,15.320874689078,0.));
#30500=CARTESIAN_POINT('Ctrl Pts',(37.7607947318286,15.320070396385,0.));
#30501=CARTESIAN_POINT('Ctrl Pts',(37.8601926265378,15.3186394335023,0.));
#30502=CARTESIAN_POINT('Ctrl Pts',(37.959716421934,15.3165911656268,0.));
#30503=CARTESIAN_POINT('Ctrl Pts',(38.0593621055415,15.3139321941687,0.));
#30504=CARTESIAN_POINT('Ctrl Pts',(38.1591262705847,15.310667421514,0.));
#30505=CARTESIAN_POINT('Ctrl Pts',(38.2590058835965,15.3068007250314,0.));
#30506=CARTESIAN_POINT('Ctrl Pts',(38.3589980188324,15.3023357307483,0.));
#30507=CARTESIAN_POINT('Ctrl Pts',(38.4590995527814,15.2972767037469,0.));
#30508=CARTESIAN_POINT('Ctrl Pts',(38.5593070891769,15.2916287700102,0.));
#30509=CARTESIAN_POINT('Ctrl Pts',(38.659617115053,15.2853974668211,0.));
#30510=CARTESIAN_POINT('Ctrl Pts',(38.7600260961351,15.2785884727112,0.));
#30511=CARTESIAN_POINT('Ctrl Pts',(38.860530586589,15.2712072937639,0.));
#30512=CARTESIAN_POINT('Ctrl Pts',(38.9611273555758,15.2632589109473,0.));
#30513=CARTESIAN_POINT('Ctrl Pts',(39.061813415425,15.2547476855825,0.));
#30514=CARTESIAN_POINT('Ctrl Pts',(39.1625859371304,15.2456775636447,0.));
#30515=CARTESIAN_POINT('Ctrl Pts',(39.2634421927888,15.2360522089072,0.));
#30516=CARTESIAN_POINT('Ctrl Pts',(39.3643794927167,15.225875156307,0.));
#30517=CARTESIAN_POINT('Ctrl Pts',(39.4653951093947,15.2151499908149,0.));
#30518=CARTESIAN_POINT('Ctrl Pts',(39.5664862602472,15.2038804098649,0.));
#30519=CARTESIAN_POINT('Ctrl Pts',(39.6676501731673,15.1920701163803,0.));
#30520=CARTESIAN_POINT('Ctrl Pts',(39.7688841338802,15.1797227547561,0.));
#30521=CARTESIAN_POINT('Ctrl Pts',(39.8701855339908,15.1668418393198,0.));
#30522=CARTESIAN_POINT('Ctrl Pts',(39.9715519332134,15.1534306754871,0.));
#30523=CARTESIAN_POINT('Ctrl Pts',(40.0729810652204,15.1394923361537,0.));
#30524=CARTESIAN_POINT('Ctrl Pts',(40.1744707357902,15.1250297462408,0.));
#30525=CARTESIAN_POINT('Ctrl Pts',(40.2760187401821,15.1100457495259,0.));
#30526=CARTESIAN_POINT('Ctrl Pts',(40.3776227809037,15.0945431800723,0.));
#30527=CARTESIAN_POINT('Ctrl Pts',(40.4792803645352,15.0785249502524,0.));
#30528=CARTESIAN_POINT('Ctrl Pts',(40.58098877043,15.0619940893017,0.));
#30529=CARTESIAN_POINT('Ctrl Pts',(40.6827452453667,15.0449536183143,0.));
#30530=CARTESIAN_POINT('Ctrl Pts',(40.7845471608654,15.0274064563211,0.));
#30531=CARTESIAN_POINT('Ctrl Pts',(40.8863921801,15.0093553188655,0.));
#30532=CARTESIAN_POINT('Ctrl Pts',(40.9882784321884,14.9908026205824,0.));
#30533=CARTESIAN_POINT('Ctrl Pts',(41.1105898934098,14.9679399407908,0.));
#30534=CARTESIAN_POINT('Ctrl Pts',(41.2125650743922,14.9482653093396,0.));
#30535=CARTESIAN_POINT('Ctrl Pts',(41.2941761025922,14.9321285285561,0.));
#30536=CARTESIAN_POINT('Ctrl Pts',(41.3554017279611,14.919802810928,0.));
#30537=CARTESIAN_POINT('Ctrl Pts',(41.396226524684,14.911486495888,0.));
#30538=CARTESIAN_POINT('',(41.3962265246839,14.9114864958881,15.));
#30539=CARTESIAN_POINT('Ctrl Pts',(41.396226524684,14.911486495888,15.));
#30540=CARTESIAN_POINT('Ctrl Pts',(41.3758141263348,14.9156446533966,15.));
#30541=CARTESIAN_POINT('Ctrl Pts',(41.3349931861715,14.9239113834707,15.));
#30542=CARTESIAN_POINT('Ctrl Pts',(41.2737733455422,14.936162723752,15.));
#30543=CARTESIAN_POINT('Ctrl Pts',(41.1921700381957,14.9522002356298,15.));
#30544=CARTESIAN_POINT('Ctrl Pts',(41.0902046498729,14.9717503874227,15.));
#30545=CARTESIAN_POINT('Ctrl Pts',(40.9882784321884,14.9908026205824,15.));
#30546=CARTESIAN_POINT('Ctrl Pts',(40.8863921801,15.0093553188655,15.));
#30547=CARTESIAN_POINT('Ctrl Pts',(40.7845471608654,15.0274064563211,15.));
#30548=CARTESIAN_POINT('Ctrl Pts',(40.6827452453667,15.0449536183143,15.));
#30549=CARTESIAN_POINT('Ctrl Pts',(40.58098877043,15.0619940893017,15.));
#30550=CARTESIAN_POINT('Ctrl Pts',(40.4792803645352,15.0785249502524,15.));
#30551=CARTESIAN_POINT('Ctrl Pts',(40.3776227809037,15.0945431800723,15.));
#30552=CARTESIAN_POINT('Ctrl Pts',(40.2760187401821,15.1100457495259,15.));
#30553=CARTESIAN_POINT('Ctrl Pts',(40.1744707357902,15.1250297462408,15.));
#30554=CARTESIAN_POINT('Ctrl Pts',(40.0729810652204,15.1394923361537,15.));
#30555=CARTESIAN_POINT('Ctrl Pts',(39.9715519332134,15.1534306754871,15.));
#30556=CARTESIAN_POINT('Ctrl Pts',(39.8701855339908,15.1668418393198,15.));
#30557=CARTESIAN_POINT('Ctrl Pts',(39.7688841338802,15.1797227547561,15.));
#30558=CARTESIAN_POINT('Ctrl Pts',(39.6676501731673,15.1920701163803,15.));
#30559=CARTESIAN_POINT('Ctrl Pts',(39.5664862602472,15.2038804098649,15.));
#30560=CARTESIAN_POINT('Ctrl Pts',(39.4653951093947,15.2151499908149,15.));
#30561=CARTESIAN_POINT('Ctrl Pts',(39.3643794927167,15.225875156307,15.));
#30562=CARTESIAN_POINT('Ctrl Pts',(39.2634421927888,15.2360522089072,15.));
#30563=CARTESIAN_POINT('Ctrl Pts',(39.1625859371304,15.2456775636447,15.));
#30564=CARTESIAN_POINT('Ctrl Pts',(39.061813415425,15.2547476855825,15.));
#30565=CARTESIAN_POINT('Ctrl Pts',(38.9611273555758,15.2632589109473,15.));
#30566=CARTESIAN_POINT('Ctrl Pts',(38.860530586589,15.2712072937639,15.));
#30567=CARTESIAN_POINT('Ctrl Pts',(38.7600260961351,15.2785884727112,15.));
#30568=CARTESIAN_POINT('Ctrl Pts',(38.659617115053,15.2853974668211,15.));
#30569=CARTESIAN_POINT('Ctrl Pts',(38.5593070891769,15.2916287700102,15.));
#30570=CARTESIAN_POINT('Ctrl Pts',(38.4590995527814,15.2972767037469,15.));
#30571=CARTESIAN_POINT('Ctrl Pts',(38.3589980188324,15.3023357307483,15.));
#30572=CARTESIAN_POINT('Ctrl Pts',(38.2590058835965,15.3068007250314,15.));
#30573=CARTESIAN_POINT('Ctrl Pts',(38.1591262705847,15.310667421514,15.));
#30574=CARTESIAN_POINT('Ctrl Pts',(38.0593621055415,15.3139321941687,15.));
#30575=CARTESIAN_POINT('Ctrl Pts',(37.959716421934,15.3165911656268,15.));
#30576=CARTESIAN_POINT('Ctrl Pts',(37.8601926265378,15.3186394335023,15.));
#30577=CARTESIAN_POINT('Ctrl Pts',(37.7607947318286,15.320070396385,15.));
#30578=CARTESIAN_POINT('Ctrl Pts',(37.6615277218027,15.320874689078,15.));
#30579=CARTESIAN_POINT('Ctrl Pts',(37.562397408596,15.3210406145546,15.));
#30580=CARTESIAN_POINT('Ctrl Pts',(37.4634097578665,15.3205561366169,15.));
#30581=CARTESIAN_POINT('Ctrl Pts',(37.3645702997848,15.3194106233801,15.));
#30582=CARTESIAN_POINT('Ctrl Pts',(37.2658836214694,15.3175963510698,15.));
#30583=CARTESIAN_POINT('Ctrl Pts',(37.1673525354642,15.3151109648809,15.));
#30584=CARTESIAN_POINT('Ctrl Pts',(37.0689784837457,15.3119562971444,15.));
#30585=CARTESIAN_POINT('Ctrl Pts',(36.970763176802,15.3081335446406,15.));
#30586=CARTESIAN_POINT('Ctrl Pts',(36.8727100302512,15.3036390436952,15.));
#30587=CARTESIAN_POINT('Ctrl Pts',(36.7748254044502,15.2984606286737,15.));
#30588=CARTESIAN_POINT('Ctrl Pts',(36.6771206167755,15.2925717100767,15.));
#30589=CARTESIAN_POINT('Ctrl Pts',(36.5796108931244,15.2859343913094,15.));
#30590=CARTESIAN_POINT('Ctrl Pts',(36.4823116513289,15.2785104654792,15.));
#30591=CARTESIAN_POINT('Ctrl Pts',(36.3852352131887,15.2702711460937,15.));
#30592=CARTESIAN_POINT('Ctrl Pts',(36.2883880151607,15.2612053303773,15.));
#30593=CARTESIAN_POINT('Ctrl Pts',(36.1917659216814,15.2513334565427,15.));
#30594=CARTESIAN_POINT('Ctrl Pts',(36.095357546697,15.240697754828,15.));
#30595=CARTESIAN_POINT('Ctrl Pts',(35.9991531408727,15.2293360946131,15.));
#30596=CARTESIAN_POINT('Ctrl Pts',(35.9031525499277,15.2172585668056,15.));
#30597=CARTESIAN_POINT('Ctrl Pts',(35.8073720252878,15.2044274601769,15.));
#30598=CARTESIAN_POINT('Ctrl Pts',(35.7118553943773,15.1907243629659,15.));
#30599=CARTESIAN_POINT('Ctrl Pts',(35.6166644736253,15.1759785763051,15.));
#30600=CARTESIAN_POINT('Ctrl Pts',(35.5218591529745,15.1600260710384,15.));
#30601=CARTESIAN_POINT('Ctrl Pts',(35.4274792115856,15.1427632633831,15.));
#30602=CARTESIAN_POINT('Ctrl Pts',(35.3335286891314,15.1241934020681,15.));
#30603=CARTESIAN_POINT('Ctrl Pts',(35.2399506932815,15.104500806927,15.));
#30604=CARTESIAN_POINT('Ctrl Pts',(35.1466591020976,15.08395927165,15.));
#30605=CARTESIAN_POINT('Ctrl Pts',(35.0535882932913,15.0627878528202,15.));
#30606=CARTESIAN_POINT('Ctrl Pts',(34.9607388363587,15.041018569143,15.));
#30607=CARTESIAN_POINT('Ctrl Pts',(34.8682205930809,15.0183713484962,15.));
#30608=CARTESIAN_POINT('Ctrl Pts',(34.7763085406486,14.9940927023322,15.));
#30609=CARTESIAN_POINT('Ctrl Pts',(34.6853717911268,14.9671565602316,15.));
#30610=CARTESIAN_POINT('Ctrl Pts',(34.6137007885254,14.9426481276593,15.));
#30611=CARTESIAN_POINT('Ctrl Pts',(34.5606858566713,14.9222326355678,15.));
#30612=CARTESIAN_POINT('Ctrl Pts',(34.525687510388,14.9076710061311,15.));
#30613=CARTESIAN_POINT('Ctrl Pts',(34.5082745737944,14.9001523628048,15.));
#30614=CARTESIAN_POINT('',(41.3962265246839,14.9114864958881,0.));
#30615=CARTESIAN_POINT('Origin',(1.07784724682657E-11,3.50213800024364E-12,
0.));
#30616=CARTESIAN_POINT('',(42.2550026135057,12.2684454652018,0.));
#30617=CARTESIAN_POINT('Origin',(1.07784724682657E-11,3.50213800024364E-12,
0.));
#30618=CARTESIAN_POINT('',(42.2550026135057,12.2684454652018,15.));
#30619=CARTESIAN_POINT('Origin',(1.07784724682657E-11,3.50213800024364E-12,
15.));
#30620=CARTESIAN_POINT('',(42.2550026135057,12.2684454652018,0.));
#30621=CARTESIAN_POINT('Ctrl Pts',(36.6758703925241,8.22897839625061,0.));
#30622=CARTESIAN_POINT('Ctrl Pts',(36.6758703925241,8.22897839625061,18.));
#30623=CARTESIAN_POINT('Ctrl Pts',(36.6943771018148,8.23313075335376,0.));
#30624=CARTESIAN_POINT('Ctrl Pts',(36.6943771018148,8.23313075335376,18.));
#30625=CARTESIAN_POINT('Ctrl Pts',(36.7312504697652,8.24192165947367,0.));
#30626=CARTESIAN_POINT('Ctrl Pts',(36.7312504697652,8.24192165947367,18.));
#30627=CARTESIAN_POINT('Ctrl Pts',(36.7861403757604,8.2565665745182,0.));
#30628=CARTESIAN_POINT('Ctrl Pts',(36.7861403757604,8.2565665745182,18.));
#30629=CARTESIAN_POINT('Ctrl Pts',(36.8585291300917,8.27886599440785,0.));
#30630=CARTESIAN_POINT('Ctrl Pts',(36.8585291300917,8.27886599440785,18.));
#30631=CARTESIAN_POINT('Ctrl Pts',(36.9479311729484,8.31052547794591,0.));
#30632=CARTESIAN_POINT('Ctrl Pts',(36.9479311729484,8.31052547794591,18.));
#30633=CARTESIAN_POINT('Ctrl Pts',(37.0365602155148,8.34490818952639,0.));
#30634=CARTESIAN_POINT('Ctrl Pts',(37.0365602155148,8.34490818952639,18.));
#30635=CARTESIAN_POINT('Ctrl Pts',(37.1247207489179,8.38096706211448,0.));
#30636=CARTESIAN_POINT('Ctrl Pts',(37.1247207489179,8.38096706211448,18.));
#30637=CARTESIAN_POINT('Ctrl Pts',(37.2126332013933,8.4179308831326,0.));
#30638=CARTESIAN_POINT('Ctrl Pts',(37.2126332013933,8.4179308831326,18.));
#30639=CARTESIAN_POINT('Ctrl Pts',(37.3003733151561,8.4555084943396,0.));
#30640=CARTESIAN_POINT('Ctrl Pts',(37.3003733151561,8.4555084943396,18.));
#30641=CARTESIAN_POINT('Ctrl Pts',(37.3879218093514,8.49372546467076,0.));
#30642=CARTESIAN_POINT('Ctrl Pts',(37.3879218093514,8.49372546467076,18.));
#30643=CARTESIAN_POINT('Ctrl Pts',(37.4752030152968,8.53279758643784,0.));
#30644=CARTESIAN_POINT('Ctrl Pts',(37.4752030152968,8.53279758643784,18.));
#30645=CARTESIAN_POINT('Ctrl Pts',(37.5621256752108,8.57299698459465,0.));
#30646=CARTESIAN_POINT('Ctrl Pts',(37.5621256752108,8.57299698459465,18.));
#30647=CARTESIAN_POINT('Ctrl Pts',(37.6486274754754,8.61450621749155,0.));
#30648=CARTESIAN_POINT('Ctrl Pts',(37.6486274754754,8.61450621749155,18.));
#30649=CARTESIAN_POINT('Ctrl Pts',(37.7347032383719,8.65732553894524,0.));
#30650=CARTESIAN_POINT('Ctrl Pts',(37.7347032383719,8.65732553894524,18.));
#30651=CARTESIAN_POINT('Ctrl Pts',(37.8203816669031,8.70134776631143,0.));
#30652=CARTESIAN_POINT('Ctrl Pts',(37.8203816669031,8.70134776631143,18.));
#30653=CARTESIAN_POINT('Ctrl Pts',(37.9057107230066,8.74640499479002,0.));
#30654=CARTESIAN_POINT('Ctrl Pts',(37.9057107230066,8.74640499479002,18.));
#30655=CARTESIAN_POINT('Ctrl Pts',(37.9907407304174,8.79232279131092,0.));
#30656=CARTESIAN_POINT('Ctrl Pts',(37.9907407304174,8.79232279131092,18.));
#30657=CARTESIAN_POINT('Ctrl Pts',(38.0755058326913,8.83897959763349,0.));
#30658=CARTESIAN_POINT('Ctrl Pts',(38.0755058326913,8.83897959763349,18.));
#30659=CARTESIAN_POINT('Ctrl Pts',(38.1600150482528,8.88633535238434,0.));
#30660=CARTESIAN_POINT('Ctrl Pts',(38.1600150482528,8.88633535238434,18.));
#30661=CARTESIAN_POINT('Ctrl Pts',(38.2442625706309,8.93439830996339,0.));
#30662=CARTESIAN_POINT('Ctrl Pts',(38.2442625706309,8.93439830996339,18.));
#30663=CARTESIAN_POINT('Ctrl Pts',(38.3282340281403,8.9832048378576,0.));
#30664=CARTESIAN_POINT('Ctrl Pts',(38.3282340281403,8.9832048378576,18.));
#30665=CARTESIAN_POINT('Ctrl Pts',(38.4119138099805,9.03279579360191,0.));
#30666=CARTESIAN_POINT('Ctrl Pts',(38.4119138099805,9.03279579360191,18.));
#30667=CARTESIAN_POINT('Ctrl Pts',(38.4952932486131,9.08319014288086,0.));
#30668=CARTESIAN_POINT('Ctrl Pts',(38.4952932486131,9.08319014288086,18.));
#30669=CARTESIAN_POINT('Ctrl Pts',(38.5783736628826,9.13437512010586,0.));
#30670=CARTESIAN_POINT('Ctrl Pts',(38.5783736628826,9.13437512010586,18.));
#30671=CARTESIAN_POINT('Ctrl Pts',(38.6611620045193,9.1863201939433,0.));
#30672=CARTESIAN_POINT('Ctrl Pts',(38.6611620045193,9.1863201939433,18.));
#30673=CARTESIAN_POINT('Ctrl Pts',(38.7436682576832,9.23898539199331,0.));
#30674=CARTESIAN_POINT('Ctrl Pts',(38.7436682576832,9.23898539199331,18.));
#30675=CARTESIAN_POINT('Ctrl Pts',(38.8259023794241,9.29233110570903,0.));
#30676=CARTESIAN_POINT('Ctrl Pts',(38.8259023794241,9.29233110570903,18.));
#30677=CARTESIAN_POINT('Ctrl Pts',(38.9078708427078,9.34632917154637,0.));
#30678=CARTESIAN_POINT('Ctrl Pts',(38.9078708427078,9.34632917154637,18.));
#30679=CARTESIAN_POINT('Ctrl Pts',(38.9895756526779,9.40096600877644,0.));
#30680=CARTESIAN_POINT('Ctrl Pts',(38.9895756526779,9.40096600877644,18.));
#30681=CARTESIAN_POINT('Ctrl Pts',(39.0710161994951,9.45623664577431,0.));
#30682=CARTESIAN_POINT('Ctrl Pts',(39.0710161994951,9.45623664577431,18.));
#30683=CARTESIAN_POINT('Ctrl Pts',(39.1521903958955,9.51214104535621,0.));
#30684=CARTESIAN_POINT('Ctrl Pts',(39.1521903958955,9.51214104535621,18.));
#30685=CARTESIAN_POINT('Ctrl Pts',(39.2330959982788,9.56867984233623,0.));
#30686=CARTESIAN_POINT('Ctrl Pts',(39.2330959982788,9.56867984233623,18.));
#30687=CARTESIAN_POINT('Ctrl Pts',(39.3137321153686,9.62584947846543,0.));
#30688=CARTESIAN_POINT('Ctrl Pts',(39.3137321153686,9.62584947846543,18.));
#30689=CARTESIAN_POINT('Ctrl Pts',(39.3940995760289,9.68364100883826,0.));
#30690=CARTESIAN_POINT('Ctrl Pts',(39.3940995760289,9.68364100883826,18.));
#30691=CARTESIAN_POINT('Ctrl Pts',(39.4742001555227,9.74204258152663,0.));
#30692=CARTESIAN_POINT('Ctrl Pts',(39.4742001555227,9.74204258152663,18.));
#30693=CARTESIAN_POINT('Ctrl Pts',(39.5540361022309,9.80104095251613,0.));
#30694=CARTESIAN_POINT('Ctrl Pts',(39.5540361022309,9.80104095251613,18.));
#30695=CARTESIAN_POINT('Ctrl Pts',(39.6336095893767,9.86062324242559,0.));
#30696=CARTESIAN_POINT('Ctrl Pts',(39.6336095893767,9.86062324242559,18.));
#30697=CARTESIAN_POINT('Ctrl Pts',(39.712922089547,9.92077894513191,0.));
#30698=CARTESIAN_POINT('Ctrl Pts',(39.712922089547,9.92077894513191,18.));
#30699=CARTESIAN_POINT('Ctrl Pts',(39.7919742367922,9.98150036150823,0.));
#30700=CARTESIAN_POINT('Ctrl Pts',(39.7919742367922,9.98150036150823,18.));
#30701=CARTESIAN_POINT('Ctrl Pts',(39.8707661565233,10.0427815229883,0.));
#30702=CARTESIAN_POINT('Ctrl Pts',(39.8707661565233,10.0427815229883,18.));
#30703=CARTESIAN_POINT('Ctrl Pts',(39.9492976736738,10.1046175096878,0.));
#30704=CARTESIAN_POINT('Ctrl Pts',(39.9492976736738,10.1046175096878,18.));
#30705=CARTESIAN_POINT('Ctrl Pts',(40.0275685525923,10.1670036683795,0.));
#30706=CARTESIAN_POINT('Ctrl Pts',(40.0275685525923,10.1670036683795,18.));
#30707=CARTESIAN_POINT('Ctrl Pts',(40.1055787732578,10.2299347125857,0.));
#30708=CARTESIAN_POINT('Ctrl Pts',(40.1055787732578,10.2299347125857,18.));
#30709=CARTESIAN_POINT('Ctrl Pts',(40.1833286010098,10.2934044990237,0.));
#30710=CARTESIAN_POINT('Ctrl Pts',(40.1833286010098,10.2934044990237,18.));
#30711=CARTESIAN_POINT('Ctrl Pts',(40.2608184485326,10.3574064830678,0.));
#30712=CARTESIAN_POINT('Ctrl Pts',(40.2608184485326,10.3574064830678,18.));
#30713=CARTESIAN_POINT('Ctrl Pts',(40.3380487942952,10.421933993295,0.));
#30714=CARTESIAN_POINT('Ctrl Pts',(40.3380487942952,10.421933993295,18.));
#30715=CARTESIAN_POINT('Ctrl Pts',(40.4150200869536,10.48698054978,0.));
#30716=CARTESIAN_POINT('Ctrl Pts',(40.4150200869536,10.48698054978,18.));
#30717=CARTESIAN_POINT('Ctrl Pts',(40.4917326404439,10.5525402237951,0.));
#30718=CARTESIAN_POINT('Ctrl Pts',(40.4917326404439,10.5525402237951,18.));
#30719=CARTESIAN_POINT('Ctrl Pts',(40.5681866012103,10.618607730849,0.));
#30720=CARTESIAN_POINT('Ctrl Pts',(40.5681866012103,10.618607730849,18.));
#30721=CARTESIAN_POINT('Ctrl Pts',(40.6443819999244,10.6851782157325,0.));
#30722=CARTESIAN_POINT('Ctrl Pts',(40.6443819999244,10.6851782157325,18.));
#30723=CARTESIAN_POINT('Ctrl Pts',(40.7203187831783,10.7522471109694,0.));
#30724=CARTESIAN_POINT('Ctrl Pts',(40.7203187831783,10.7522471109694,18.));
#30725=CARTESIAN_POINT('Ctrl Pts',(40.795996852756,10.8198099757795,0.));
#30726=CARTESIAN_POINT('Ctrl Pts',(40.795996852756,10.8198099757795,18.));
#30727=CARTESIAN_POINT('Ctrl Pts',(40.8714161092412,10.8878623066646,0.));
#30728=CARTESIAN_POINT('Ctrl Pts',(40.8714161092412,10.8878623066646,18.));
#30729=CARTESIAN_POINT('Ctrl Pts',(40.9465764747798,10.956399476781,0.));
#30730=CARTESIAN_POINT('Ctrl Pts',(40.9465764747798,10.956399476781,18.));
#30731=CARTESIAN_POINT('Ctrl Pts',(41.0214778832142,11.0254168609972,0.));
#30732=CARTESIAN_POINT('Ctrl Pts',(41.0214778832142,11.0254168609972,18.));
#30733=CARTESIAN_POINT('Ctrl Pts',(41.0961202807715,11.0949099155251,0.));
#30734=CARTESIAN_POINT('Ctrl Pts',(41.0961202807715,11.0949099155251,18.));
#30735=CARTESIAN_POINT('Ctrl Pts',(41.1705036228854,11.1648742640378,0.));
#30736=CARTESIAN_POINT('Ctrl Pts',(41.1705036228854,11.1648742640378,18.));
#30737=CARTESIAN_POINT('Ctrl Pts',(41.2446278781981,11.2353057980338,0.));
#30738=CARTESIAN_POINT('Ctrl Pts',(41.2446278781981,11.2353057980338,18.));
#30739=CARTESIAN_POINT('Ctrl Pts',(41.3184930194148,11.3062006993745,0.));
#30740=CARTESIAN_POINT('Ctrl Pts',(41.3184930194148,11.3062006993745,18.));
#30741=CARTESIAN_POINT('Ctrl Pts',(41.3920989905986,11.3775553120176,0.));
#30742=CARTESIAN_POINT('Ctrl Pts',(41.3920989905986,11.3775553120176,18.));
#30743=CARTESIAN_POINT('Ctrl Pts',(41.4654456796071,11.4493660393849,0.));
#30744=CARTESIAN_POINT('Ctrl Pts',(41.4654456796071,11.4493660393849,18.));
#30745=CARTESIAN_POINT('Ctrl Pts',(41.5385328935506,11.5216292382388,0.));
#30746=CARTESIAN_POINT('Ctrl Pts',(41.5385328935506,11.5216292382388,18.));
#30747=CARTESIAN_POINT('Ctrl Pts',(41.6113603270596,11.5943410868252,0.));
#30748=CARTESIAN_POINT('Ctrl Pts',(41.6113603270596,11.5943410868252,18.));
#30749=CARTESIAN_POINT('Ctrl Pts',(41.6839275596248,11.6674975352851,0.));
#30750=CARTESIAN_POINT('Ctrl Pts',(41.6839275596248,11.6674975352851,18.));
#30751=CARTESIAN_POINT('Ctrl Pts',(41.7562341395977,11.7410945211992,0.));
#30752=CARTESIAN_POINT('Ctrl Pts',(41.7562341395977,11.7410945211992,18.));
#30753=CARTESIAN_POINT('Ctrl Pts',(41.8282796562569,11.81512813804,0.));
#30754=CARTESIAN_POINT('Ctrl Pts',(41.8282796562569,11.81512813804,18.));
#30755=CARTESIAN_POINT('Ctrl Pts',(41.9000638152266,11.8895948153349,0.));
#30756=CARTESIAN_POINT('Ctrl Pts',(41.9000638152266,11.8895948153349,18.));
#30757=CARTESIAN_POINT('Ctrl Pts',(41.9715865222182,11.9644914999263,0.));
#30758=CARTESIAN_POINT('Ctrl Pts',(41.9715865222182,11.9644914999263,18.));
#30759=CARTESIAN_POINT('Ctrl Pts',(42.0428479428228,12.0398158079102,0.));
#30760=CARTESIAN_POINT('Ctrl Pts',(42.0428479428228,12.0398158079102,18.));
#30761=CARTESIAN_POINT('Ctrl Pts',(42.1138483839101,12.1155659644537,0.));
#30762=CARTESIAN_POINT('Ctrl Pts',(42.1138483839101,12.1155659644537,18.));
#30763=CARTESIAN_POINT('Ctrl Pts',(42.1704402333854,12.1765058047069,0.));
#30764=CARTESIAN_POINT('Ctrl Pts',(42.1704402333854,12.1765058047069,18.));
#30765=CARTESIAN_POINT('Ctrl Pts',(42.2127669677092,12.222401466668,0.));
#30766=CARTESIAN_POINT('Ctrl Pts',(42.2127669677092,12.222401466668,18.));
#30767=CARTESIAN_POINT('Ctrl Pts',(42.2409327400055,12.2530833383985,0.));
#30768=CARTESIAN_POINT('Ctrl Pts',(42.2409327400055,12.2530833383985,18.));
#30769=CARTESIAN_POINT('Ctrl Pts',(42.2550026135057,12.2684454652018,0.));
#30770=CARTESIAN_POINT('Ctrl Pts',(42.2550026135057,12.2684454652018,18.));
#30771=CARTESIAN_POINT('Ctrl Pts',(36.6758703925241,8.22897839625061,0.));
#30772=CARTESIAN_POINT('Ctrl Pts',(36.6943771018148,8.23313075335376,0.));
#30773=CARTESIAN_POINT('Ctrl Pts',(36.7312504697652,8.24192165947367,0.));
#30774=CARTESIAN_POINT('Ctrl Pts',(36.7861403757604,8.2565665745182,0.));
#30775=CARTESIAN_POINT('Ctrl Pts',(36.8585291300917,8.27886599440785,0.));
#30776=CARTESIAN_POINT('Ctrl Pts',(36.9479311729484,8.31052547794591,0.));
#30777=CARTESIAN_POINT('Ctrl Pts',(37.0365602155148,8.34490818952639,0.));
#30778=CARTESIAN_POINT('Ctrl Pts',(37.1247207489179,8.38096706211448,0.));
#30779=CARTESIAN_POINT('Ctrl Pts',(37.2126332013933,8.4179308831326,0.));
#30780=CARTESIAN_POINT('Ctrl Pts',(37.3003733151561,8.4555084943396,0.));
#30781=CARTESIAN_POINT('Ctrl Pts',(37.3879218093514,8.49372546467076,0.));
#30782=CARTESIAN_POINT('Ctrl Pts',(37.4752030152968,8.53279758643784,0.));
#30783=CARTESIAN_POINT('Ctrl Pts',(37.5621256752108,8.57299698459465,0.));
#30784=CARTESIAN_POINT('Ctrl Pts',(37.6486274754754,8.61450621749155,0.));
#30785=CARTESIAN_POINT('Ctrl Pts',(37.7347032383719,8.65732553894524,0.));
#30786=CARTESIAN_POINT('Ctrl Pts',(37.8203816669031,8.70134776631143,0.));
#30787=CARTESIAN_POINT('Ctrl Pts',(37.9057107230066,8.74640499479002,0.));
#30788=CARTESIAN_POINT('Ctrl Pts',(37.9907407304174,8.79232279131092,0.));
#30789=CARTESIAN_POINT('Ctrl Pts',(38.0755058326913,8.83897959763349,0.));
#30790=CARTESIAN_POINT('Ctrl Pts',(38.1600150482528,8.88633535238434,0.));
#30791=CARTESIAN_POINT('Ctrl Pts',(38.2442625706309,8.93439830996339,0.));
#30792=CARTESIAN_POINT('Ctrl Pts',(38.3282340281403,8.9832048378576,0.));
#30793=CARTESIAN_POINT('Ctrl Pts',(38.4119138099805,9.03279579360191,0.));
#30794=CARTESIAN_POINT('Ctrl Pts',(38.4952932486131,9.08319014288086,0.));
#30795=CARTESIAN_POINT('Ctrl Pts',(38.5783736628826,9.13437512010586,0.));
#30796=CARTESIAN_POINT('Ctrl Pts',(38.6611620045193,9.1863201939433,0.));
#30797=CARTESIAN_POINT('Ctrl Pts',(38.7436682576832,9.23898539199331,0.));
#30798=CARTESIAN_POINT('Ctrl Pts',(38.8259023794241,9.29233110570903,0.));
#30799=CARTESIAN_POINT('Ctrl Pts',(38.9078708427078,9.34632917154637,0.));
#30800=CARTESIAN_POINT('Ctrl Pts',(38.9895756526779,9.40096600877644,0.));
#30801=CARTESIAN_POINT('Ctrl Pts',(39.0710161994951,9.45623664577431,0.));
#30802=CARTESIAN_POINT('Ctrl Pts',(39.1521903958955,9.51214104535621,0.));
#30803=CARTESIAN_POINT('Ctrl Pts',(39.2330959982788,9.56867984233623,0.));
#30804=CARTESIAN_POINT('Ctrl Pts',(39.3137321153686,9.62584947846543,0.));
#30805=CARTESIAN_POINT('Ctrl Pts',(39.3940995760289,9.68364100883826,0.));
#30806=CARTESIAN_POINT('Ctrl Pts',(39.4742001555227,9.74204258152663,0.));
#30807=CARTESIAN_POINT('Ctrl Pts',(39.5540361022309,9.80104095251613,0.));
#30808=CARTESIAN_POINT('Ctrl Pts',(39.6336095893767,9.86062324242559,0.));
#30809=CARTESIAN_POINT('Ctrl Pts',(39.712922089547,9.92077894513191,0.));
#30810=CARTESIAN_POINT('Ctrl Pts',(39.7919742367922,9.98150036150823,0.));
#30811=CARTESIAN_POINT('Ctrl Pts',(39.8707661565233,10.0427815229883,0.));
#30812=CARTESIAN_POINT('Ctrl Pts',(39.9492976736738,10.1046175096878,0.));
#30813=CARTESIAN_POINT('Ctrl Pts',(40.0275685525923,10.1670036683795,0.));
#30814=CARTESIAN_POINT('Ctrl Pts',(40.1055787732578,10.2299347125857,0.));
#30815=CARTESIAN_POINT('Ctrl Pts',(40.1833286010098,10.2934044990237,0.));
#30816=CARTESIAN_POINT('Ctrl Pts',(40.2608184485326,10.3574064830678,0.));
#30817=CARTESIAN_POINT('Ctrl Pts',(40.3380487942952,10.421933993295,0.));
#30818=CARTESIAN_POINT('Ctrl Pts',(40.4150200869536,10.48698054978,0.));
#30819=CARTESIAN_POINT('Ctrl Pts',(40.4917326404439,10.5525402237951,0.));
#30820=CARTESIAN_POINT('Ctrl Pts',(40.5681866012103,10.618607730849,0.));
#30821=CARTESIAN_POINT('Ctrl Pts',(40.6443819999244,10.6851782157325,0.));
#30822=CARTESIAN_POINT('Ctrl Pts',(40.7203187831783,10.7522471109694,0.));
#30823=CARTESIAN_POINT('Ctrl Pts',(40.795996852756,10.8198099757795,0.));
#30824=CARTESIAN_POINT('Ctrl Pts',(40.8714161092412,10.8878623066646,0.));
#30825=CARTESIAN_POINT('Ctrl Pts',(40.9465764747798,10.956399476781,0.));
#30826=CARTESIAN_POINT('Ctrl Pts',(41.0214778832142,11.0254168609972,0.));
#30827=CARTESIAN_POINT('Ctrl Pts',(41.0961202807715,11.0949099155251,0.));
#30828=CARTESIAN_POINT('Ctrl Pts',(41.1705036228854,11.1648742640378,0.));
#30829=CARTESIAN_POINT('Ctrl Pts',(41.2446278781981,11.2353057980338,0.));
#30830=CARTESIAN_POINT('Ctrl Pts',(41.3184930194148,11.3062006993745,0.));
#30831=CARTESIAN_POINT('Ctrl Pts',(41.3920989905986,11.3775553120176,0.));
#30832=CARTESIAN_POINT('Ctrl Pts',(41.4654456796071,11.4493660393849,0.));
#30833=CARTESIAN_POINT('Ctrl Pts',(41.5385328935506,11.5216292382388,0.));
#30834=CARTESIAN_POINT('Ctrl Pts',(41.6113603270596,11.5943410868252,0.));
#30835=CARTESIAN_POINT('Ctrl Pts',(41.6839275596248,11.6674975352851,0.));
#30836=CARTESIAN_POINT('Ctrl Pts',(41.7562341395977,11.7410945211992,0.));
#30837=CARTESIAN_POINT('Ctrl Pts',(41.8282796562569,11.81512813804,0.));
#30838=CARTESIAN_POINT('Ctrl Pts',(41.9000638152266,11.8895948153349,0.));
#30839=CARTESIAN_POINT('Ctrl Pts',(41.9715865222182,11.9644914999263,0.));
#30840=CARTESIAN_POINT('Ctrl Pts',(42.0571002269437,12.054880669507,0.));
#30841=CARTESIAN_POINT('Ctrl Pts',(42.1280354231517,12.1307372881904,0.));
#30842=CARTESIAN_POINT('Ctrl Pts',(42.18457517013,12.1917619768791,0.));
#30843=CARTESIAN_POINT('Ctrl Pts',(42.2268628664988,12.2377212115625,0.));
#30844=CARTESIAN_POINT('Ctrl Pts',(42.2550026135057,12.2684454652018,0.));
#30845=CARTESIAN_POINT('Ctrl Pts',(36.6758703925241,8.22897839625061,15.));
#30846=CARTESIAN_POINT('Ctrl Pts',(36.6943771018148,8.23313075335376,15.));
#30847=CARTESIAN_POINT('Ctrl Pts',(36.7312504697652,8.24192165947367,15.));
#30848=CARTESIAN_POINT('Ctrl Pts',(36.7861403757604,8.2565665745182,15.));
#30849=CARTESIAN_POINT('Ctrl Pts',(36.8585291300917,8.27886599440785,15.));
#30850=CARTESIAN_POINT('Ctrl Pts',(36.9479311729484,8.31052547794591,15.));
#30851=CARTESIAN_POINT('Ctrl Pts',(37.0365602155148,8.34490818952639,15.));
#30852=CARTESIAN_POINT('Ctrl Pts',(37.1247207489179,8.38096706211448,15.));
#30853=CARTESIAN_POINT('Ctrl Pts',(37.2126332013933,8.4179308831326,15.));
#30854=CARTESIAN_POINT('Ctrl Pts',(37.3003733151561,8.4555084943396,15.));
#30855=CARTESIAN_POINT('Ctrl Pts',(37.3879218093514,8.49372546467076,15.));
#30856=CARTESIAN_POINT('Ctrl Pts',(37.4752030152968,8.53279758643784,15.));
#30857=CARTESIAN_POINT('Ctrl Pts',(37.5621256752108,8.57299698459465,15.));
#30858=CARTESIAN_POINT('Ctrl Pts',(37.6486274754754,8.61450621749155,15.));
#30859=CARTESIAN_POINT('Ctrl Pts',(37.7347032383719,8.65732553894524,15.));
#30860=CARTESIAN_POINT('Ctrl Pts',(37.8203816669031,8.70134776631143,15.));
#30861=CARTESIAN_POINT('Ctrl Pts',(37.9057107230066,8.74640499479002,15.));
#30862=CARTESIAN_POINT('Ctrl Pts',(37.9907407304174,8.79232279131092,15.));
#30863=CARTESIAN_POINT('Ctrl Pts',(38.0755058326913,8.83897959763349,15.));
#30864=CARTESIAN_POINT('Ctrl Pts',(38.1600150482528,8.88633535238434,15.));
#30865=CARTESIAN_POINT('Ctrl Pts',(38.2442625706309,8.93439830996339,15.));
#30866=CARTESIAN_POINT('Ctrl Pts',(38.3282340281403,8.9832048378576,15.));
#30867=CARTESIAN_POINT('Ctrl Pts',(38.4119138099805,9.03279579360191,15.));
#30868=CARTESIAN_POINT('Ctrl Pts',(38.4952932486131,9.08319014288086,15.));
#30869=CARTESIAN_POINT('Ctrl Pts',(38.5783736628826,9.13437512010586,15.));
#30870=CARTESIAN_POINT('Ctrl Pts',(38.6611620045193,9.1863201939433,15.));
#30871=CARTESIAN_POINT('Ctrl Pts',(38.7436682576832,9.23898539199331,15.));
#30872=CARTESIAN_POINT('Ctrl Pts',(38.8259023794241,9.29233110570903,15.));
#30873=CARTESIAN_POINT('Ctrl Pts',(38.9078708427078,9.34632917154637,15.));
#30874=CARTESIAN_POINT('Ctrl Pts',(38.9895756526779,9.40096600877644,15.));
#30875=CARTESIAN_POINT('Ctrl Pts',(39.0710161994951,9.45623664577431,15.));
#30876=CARTESIAN_POINT('Ctrl Pts',(39.1521903958955,9.51214104535621,15.));
#30877=CARTESIAN_POINT('Ctrl Pts',(39.2330959982788,9.56867984233623,15.));
#30878=CARTESIAN_POINT('Ctrl Pts',(39.3137321153686,9.62584947846543,15.));
#30879=CARTESIAN_POINT('Ctrl Pts',(39.3940995760289,9.68364100883826,15.));
#30880=CARTESIAN_POINT('Ctrl Pts',(39.4742001555227,9.74204258152663,15.));
#30881=CARTESIAN_POINT('Ctrl Pts',(39.5540361022309,9.80104095251613,15.));
#30882=CARTESIAN_POINT('Ctrl Pts',(39.6336095893767,9.86062324242559,15.));
#30883=CARTESIAN_POINT('Ctrl Pts',(39.712922089547,9.92077894513191,15.));
#30884=CARTESIAN_POINT('Ctrl Pts',(39.7919742367922,9.98150036150823,15.));
#30885=CARTESIAN_POINT('Ctrl Pts',(39.8707661565233,10.0427815229883,15.));
#30886=CARTESIAN_POINT('Ctrl Pts',(39.9492976736738,10.1046175096878,15.));
#30887=CARTESIAN_POINT('Ctrl Pts',(40.0275685525923,10.1670036683795,15.));
#30888=CARTESIAN_POINT('Ctrl Pts',(40.1055787732578,10.2299347125857,15.));
#30889=CARTESIAN_POINT('Ctrl Pts',(40.1833286010098,10.2934044990237,15.));
#30890=CARTESIAN_POINT('Ctrl Pts',(40.2608184485326,10.3574064830678,15.));
#30891=CARTESIAN_POINT('Ctrl Pts',(40.3380487942952,10.421933993295,15.));
#30892=CARTESIAN_POINT('Ctrl Pts',(40.4150200869536,10.48698054978,15.));
#30893=CARTESIAN_POINT('Ctrl Pts',(40.4917326404439,10.5525402237951,15.));
#30894=CARTESIAN_POINT('Ctrl Pts',(40.5681866012103,10.618607730849,15.));
#30895=CARTESIAN_POINT('Ctrl Pts',(40.6443819999244,10.6851782157325,15.));
#30896=CARTESIAN_POINT('Ctrl Pts',(40.7203187831783,10.7522471109694,15.));
#30897=CARTESIAN_POINT('Ctrl Pts',(40.795996852756,10.8198099757795,15.));
#30898=CARTESIAN_POINT('Ctrl Pts',(40.8714161092412,10.8878623066646,15.));
#30899=CARTESIAN_POINT('Ctrl Pts',(40.9465764747798,10.956399476781,15.));
#30900=CARTESIAN_POINT('Ctrl Pts',(41.0214778832142,11.0254168609972,15.));
#30901=CARTESIAN_POINT('Ctrl Pts',(41.0961202807715,11.0949099155251,15.));
#30902=CARTESIAN_POINT('Ctrl Pts',(41.1705036228854,11.1648742640378,15.));
#30903=CARTESIAN_POINT('Ctrl Pts',(41.2446278781981,11.2353057980338,15.));
#30904=CARTESIAN_POINT('Ctrl Pts',(41.3184930194148,11.3062006993745,15.));
#30905=CARTESIAN_POINT('Ctrl Pts',(41.3920989905986,11.3775553120176,15.));
#30906=CARTESIAN_POINT('Ctrl Pts',(41.4654456796071,11.4493660393849,15.));
#30907=CARTESIAN_POINT('Ctrl Pts',(41.5385328935506,11.5216292382388,15.));
#30908=CARTESIAN_POINT('Ctrl Pts',(41.6113603270596,11.5943410868252,15.));
#30909=CARTESIAN_POINT('Ctrl Pts',(41.6839275596248,11.6674975352851,15.));
#30910=CARTESIAN_POINT('Ctrl Pts',(41.7562341395977,11.7410945211992,15.));
#30911=CARTESIAN_POINT('Ctrl Pts',(41.8282796562569,11.81512813804,15.));
#30912=CARTESIAN_POINT('Ctrl Pts',(41.9000638152266,11.8895948153349,15.));
#30913=CARTESIAN_POINT('Ctrl Pts',(41.9715865222182,11.9644914999263,15.));
#30914=CARTESIAN_POINT('Ctrl Pts',(42.0571002269437,12.054880669507,15.));
#30915=CARTESIAN_POINT('Ctrl Pts',(42.1280354231517,12.1307372881904,15.));
#30916=CARTESIAN_POINT('Ctrl Pts',(42.18457517013,12.1917619768791,15.));
#30917=CARTESIAN_POINT('Ctrl Pts',(42.2268628664988,12.2377212115625,15.));
#30918=CARTESIAN_POINT('Ctrl Pts',(42.2550026135057,12.2684454652018,15.));
#30919=CARTESIAN_POINT('Origin',(0.,0.,0.));
#30920=CARTESIAN_POINT('Origin',(0.,0.,0.));
#30921=CARTESIAN_POINT('Origin',(0.,0.,0.));
#30922=CARTESIAN_POINT('Origin',(0.,0.,0.));
#30923=CARTESIAN_POINT('Origin',(0.,0.,0.));
#30924=CARTESIAN_POINT('Origin',(0.,0.,0.));
#30925=CARTESIAN_POINT('Origin',(0.,0.,0.));
#30926=CARTESIAN_POINT('Origin',(0.,0.,0.));
#30927=CARTESIAN_POINT('Origin',(0.,0.,0.));
#30928=CARTESIAN_POINT('Origin',(0.,0.,0.));
#30929=CARTESIAN_POINT('Origin',(0.,0.,0.));
#30930=CARTESIAN_POINT('Origin',(0.,0.,0.));
#30931=CARTESIAN_POINT('Origin',(0.,0.,0.));
#30932=CARTESIAN_POINT('Origin',(0.,0.,0.));
#30933=CARTESIAN_POINT('Origin',(0.,0.,0.));
#30934=CARTESIAN_POINT('Origin',(0.,0.,0.));
#30935=CARTESIAN_POINT('Origin',(0.,0.,0.));
#30936=CARTESIAN_POINT('Origin',(0.,0.,0.));
#30937=CARTESIAN_POINT('',(35.1136254352094,4.26751599830831,0.));
#30938=CARTESIAN_POINT('Origin',(0.,0.,0.));
#30939=CARTESIAN_POINT('',(36.199629211057,3.39252545782466,0.));
#30940=CARTESIAN_POINT('Origin',(36.1063209411239,4.38816272448461,0.));
#30941=CARTESIAN_POINT('',(37.4237196983922,3.50724370857673,0.));
#30942=CARTESIAN_POINT('',(35.2077250236291,3.2995670413737,0.));
#30943=CARTESIAN_POINT('',(43.9780537249529,1.38952890043929,0.));
#30944=CARTESIAN_POINT('Ctrl Pts',(37.4237196983922,3.50724370857673,0.));
#30945=CARTESIAN_POINT('Ctrl Pts',(37.4426037737699,3.50901346997657,0.));
#30946=CARTESIAN_POINT('Ctrl Pts',(37.4803889700239,3.51204731876361,0.));
#30947=CARTESIAN_POINT('Ctrl Pts',(37.5371179004295,3.5150810906521,0.));
#30948=CARTESIAN_POINT('Ctrl Pts',(37.6128545966533,3.51624243734645,0.));
#30949=CARTESIAN_POINT('Ctrl Pts',(37.7076643105286,3.51375922979957,0.));
#30950=CARTESIAN_POINT('Ctrl Pts',(37.8025803811856,3.50844720825128,0.));
#30951=CARTESIAN_POINT('Ctrl Pts',(37.8975688353863,3.50139628556084,0.));
#30952=CARTESIAN_POINT('Ctrl Pts',(37.9926009950482,3.49340804454645,0.));
#30953=CARTESIAN_POINT('Ctrl Pts',(38.0876589224537,3.48478279878233,0.));
#30954=CARTESIAN_POINT('Ctrl Pts',(38.1827321816559,3.47549027265411,0.));
#30955=CARTESIAN_POINT('Ctrl Pts',(38.2778154909527,3.46530185256872,0.));
#30956=CARTESIAN_POINT('Ctrl Pts',(38.3729061502716,3.45393053211023,0.));
#30957=CARTESIAN_POINT('Ctrl Pts',(38.4680013094732,3.44118343200303,0.));
#30958=CARTESIAN_POINT('Ctrl Pts',(38.5630961226878,3.42705871084997,0.));
#30959=CARTESIAN_POINT('Ctrl Pts',(38.6581847668347,3.41166717511901,0.));
#30960=CARTESIAN_POINT('Ctrl Pts',(38.7532609709905,3.39518333281818,0.));
#30961=CARTESIAN_POINT('Ctrl Pts',(38.8483186930884,3.37778863054482,0.));
#30962=CARTESIAN_POINT('Ctrl Pts',(38.9433528420174,3.35960922799481,0.));
#30963=CARTESIAN_POINT('Ctrl Pts',(39.0383596151636,3.34068601264472,0.));
#30964=CARTESIAN_POINT('Ctrl Pts',(39.1333360409949,3.32100933979557,0.));
#30965=CARTESIAN_POINT('Ctrl Pts',(39.2282796893977,3.30054018081687,0.));
#30966=CARTESIAN_POINT('Ctrl Pts',(39.3231883392913,3.27923485388117,0.));
#30967=CARTESIAN_POINT('Ctrl Pts',(39.4180596080755,3.25707264313388,0.));
#30968=CARTESIAN_POINT('Ctrl Pts',(39.5128908052622,3.23406609691661,0.));
#30969=CARTESIAN_POINT('Ctrl Pts',(39.607679107639,3.21024640045595,0.));
#30970=CARTESIAN_POINT('Ctrl Pts',(39.7024216585552,3.18565465503835,0.));
#30971=CARTESIAN_POINT('Ctrl Pts',(39.7971156880138,3.16033160752804,0.));
#30972=CARTESIAN_POINT('Ctrl Pts',(39.8917586491576,3.13430604330356,0.));
#30973=CARTESIAN_POINT('Ctrl Pts',(39.9863482523153,3.10759149802908,0.));
#30974=CARTESIAN_POINT('Ctrl Pts',(40.0808823811787,3.08019251155015,0.));
#30975=CARTESIAN_POINT('Ctrl Pts',(40.1753590391515,3.05210847423071,0.));
#30976=CARTESIAN_POINT('Ctrl Pts',(40.2697762886113,3.02333808901595,0.));
#30977=CARTESIAN_POINT('Ctrl Pts',(40.3641321823444,2.9938844645822,0.));
#30978=CARTESIAN_POINT('Ctrl Pts',(40.4584247445196,2.96375636417323,0.));
#30979=CARTESIAN_POINT('Ctrl Pts',(40.5526520010651,2.93296560822894,0.));
#30980=CARTESIAN_POINT('Ctrl Pts',(40.6468119976928,2.90152548734343,0.));
#30981=CARTESIAN_POINT('Ctrl Pts',(40.7409028213129,2.86944892209898,0.));
#30982=CARTESIAN_POINT('Ctrl Pts',(40.8349226258683,2.83674635946679,0.));
#30983=CARTESIAN_POINT('Ctrl Pts',(40.9288696352159,2.80342531768405,0.));
#30984=CARTESIAN_POINT('Ctrl Pts',(41.0227421242398,2.76949151194863,0.));
#30985=CARTESIAN_POINT('Ctrl Pts',(41.1165384061145,2.73494956725006,0.));
#30986=CARTESIAN_POINT('Ctrl Pts',(41.2102568187956,2.69980383625016,0.));
#30987=CARTESIAN_POINT('Ctrl Pts',(41.3038957096306,2.66405934050118,0.));
#30988=CARTESIAN_POINT('Ctrl Pts',(41.3974534325936,2.62772200460656,0.));
#30989=CARTESIAN_POINT('Ctrl Pts',(41.4909283577703,2.59079818040172,0.));
#30990=CARTESIAN_POINT('Ctrl Pts',(41.5843188786284,2.55329436064184,0.));
#30991=CARTESIAN_POINT('Ctrl Pts',(41.6776234194583,2.51521684674477,0.));
#30992=CARTESIAN_POINT('Ctrl Pts',(41.7708404467532,2.47657137427693,0.));
#30993=CARTESIAN_POINT('Ctrl Pts',(41.8639684667923,2.43736301434201,0.));
#30994=CARTESIAN_POINT('Ctrl Pts',(41.9570060084039,2.39759639399648,0.));
#30995=CARTESIAN_POINT('Ctrl Pts',(42.0499516093661,2.35727584066429,0.));
#30996=CARTESIAN_POINT('Ctrl Pts',(42.1428038039937,2.31640554742809,0.));
#30997=CARTESIAN_POINT('Ctrl Pts',(42.2355611060784,2.27498976664775,0.));
#30998=CARTESIAN_POINT('Ctrl Pts',(42.3282220118033,2.233032874655,0.));
#30999=CARTESIAN_POINT('Ctrl Pts',(42.4207850290047,2.19053924976738,0.));
#31000=CARTESIAN_POINT('Ctrl Pts',(42.5132487024335,2.14751319676745,0.));
#31001=CARTESIAN_POINT('Ctrl Pts',(42.6056116373455,2.10395886401771,0.));
#31002=CARTESIAN_POINT('Ctrl Pts',(42.6978725343209,2.05988014924519,0.));
#31003=CARTESIAN_POINT('Ctrl Pts',(42.7900301875309,2.0152806752809,0.));
#31004=CARTESIAN_POINT('Ctrl Pts',(42.8820834139973,1.97016390194216,0.));
#31005=CARTESIAN_POINT('Ctrl Pts',(42.9740309956624,1.92453321512436,0.));
#31006=CARTESIAN_POINT('Ctrl Pts',(43.065871623255,1.87839202014609,0.));
#31007=CARTESIAN_POINT('Ctrl Pts',(43.1576038253643,1.83174385734712,0.));
#31008=CARTESIAN_POINT('Ctrl Pts',(43.2492259505872,1.7845924484277,0.));
#31009=CARTESIAN_POINT('Ctrl Pts',(43.3407363140236,1.73694151741124,0.));
#31010=CARTESIAN_POINT('Ctrl Pts',(43.4321333178711,1.68879465270608,0.));
#31011=CARTESIAN_POINT('Ctrl Pts',(43.5234155788248,1.64015515906648,0.));
#31012=CARTESIAN_POINT('Ctrl Pts',(43.6145820637333,1.59102591108104,0.));
#31013=CARTESIAN_POINT('Ctrl Pts',(43.7238422193529,1.53148589036097,0.));
#31014=CARTESIAN_POINT('Ctrl Pts',(43.8147465842502,1.48126213998559,0.));
#31015=CARTESIAN_POINT('Ctrl Pts',(43.8873767449248,1.44069595482723,0.));
#31016=CARTESIAN_POINT('Ctrl Pts',(43.9417969186811,1.41005374202872,0.));
#31017=CARTESIAN_POINT('Ctrl Pts',(43.9780537249529,1.38952890043916,0.));
#31018=CARTESIAN_POINT('',(43.9780537249529,-1.38952890043916,0.));
#31019=CARTESIAN_POINT('Origin',(1.13331566353736E-11,0.,0.));
#31020=CARTESIAN_POINT('',(37.4237196983922,-3.50724370857673,0.));
#31021=CARTESIAN_POINT('Ctrl Pts',(37.4237196983922,-3.50724370857673,0.));
#31022=CARTESIAN_POINT('Ctrl Pts',(37.4426037737699,-3.50901346997657,0.));
#31023=CARTESIAN_POINT('Ctrl Pts',(37.4803889700239,-3.51204731876361,0.));
#31024=CARTESIAN_POINT('Ctrl Pts',(37.5371179004295,-3.5150810906521,0.));
#31025=CARTESIAN_POINT('Ctrl Pts',(37.6128545966533,-3.51624243734645,0.));
#31026=CARTESIAN_POINT('Ctrl Pts',(37.7076643105286,-3.51375922979957,0.));
#31027=CARTESIAN_POINT('Ctrl Pts',(37.8025803811856,-3.50844720825128,0.));
#31028=CARTESIAN_POINT('Ctrl Pts',(37.8975688353863,-3.50139628556084,0.));
#31029=CARTESIAN_POINT('Ctrl Pts',(37.9926009950482,-3.49340804454645,0.));
#31030=CARTESIAN_POINT('Ctrl Pts',(38.0876589224537,-3.48478279878233,0.));
#31031=CARTESIAN_POINT('Ctrl Pts',(38.1827321816559,-3.47549027265411,0.));
#31032=CARTESIAN_POINT('Ctrl Pts',(38.2778154909527,-3.46530185256872,0.));
#31033=CARTESIAN_POINT('Ctrl Pts',(38.3729061502716,-3.45393053211023,0.));
#31034=CARTESIAN_POINT('Ctrl Pts',(38.4680013094732,-3.44118343200303,0.));
#31035=CARTESIAN_POINT('Ctrl Pts',(38.5630961226878,-3.42705871084997,0.));
#31036=CARTESIAN_POINT('Ctrl Pts',(38.6581847668347,-3.41166717511901,0.));
#31037=CARTESIAN_POINT('Ctrl Pts',(38.7532609709905,-3.39518333281818,0.));
#31038=CARTESIAN_POINT('Ctrl Pts',(38.8483186930884,-3.37778863054482,0.));
#31039=CARTESIAN_POINT('Ctrl Pts',(38.9433528420174,-3.35960922799481,0.));
#31040=CARTESIAN_POINT('Ctrl Pts',(39.0383596151636,-3.34068601264472,0.));
#31041=CARTESIAN_POINT('Ctrl Pts',(39.1333360409949,-3.32100933979557,0.));
#31042=CARTESIAN_POINT('Ctrl Pts',(39.2282796893977,-3.30054018081687,0.));
#31043=CARTESIAN_POINT('Ctrl Pts',(39.3231883392913,-3.27923485388117,0.));
#31044=CARTESIAN_POINT('Ctrl Pts',(39.4180596080755,-3.25707264313388,0.));
#31045=CARTESIAN_POINT('Ctrl Pts',(39.5128908052622,-3.23406609691661,0.));
#31046=CARTESIAN_POINT('Ctrl Pts',(39.607679107639,-3.21024640045595,0.));
#31047=CARTESIAN_POINT('Ctrl Pts',(39.7024216585552,-3.18565465503835,0.));
#31048=CARTESIAN_POINT('Ctrl Pts',(39.7971156880138,-3.16033160752804,0.));
#31049=CARTESIAN_POINT('Ctrl Pts',(39.8917586491576,-3.13430604330356,0.));
#31050=CARTESIAN_POINT('Ctrl Pts',(39.9863482523153,-3.10759149802908,0.));
#31051=CARTESIAN_POINT('Ctrl Pts',(40.0808823811787,-3.08019251155015,0.));
#31052=CARTESIAN_POINT('Ctrl Pts',(40.1753590391515,-3.05210847423071,0.));
#31053=CARTESIAN_POINT('Ctrl Pts',(40.2697762886113,-3.02333808901595,0.));
#31054=CARTESIAN_POINT('Ctrl Pts',(40.3641321823444,-2.9938844645822,0.));
#31055=CARTESIAN_POINT('Ctrl Pts',(40.4584247445196,-2.96375636417323,0.));
#31056=CARTESIAN_POINT('Ctrl Pts',(40.5526520010651,-2.93296560822894,0.));
#31057=CARTESIAN_POINT('Ctrl Pts',(40.6468119976928,-2.90152548734343,0.));
#31058=CARTESIAN_POINT('Ctrl Pts',(40.7409028213129,-2.86944892209898,0.));
#31059=CARTESIAN_POINT('Ctrl Pts',(40.8349226258683,-2.83674635946679,0.));
#31060=CARTESIAN_POINT('Ctrl Pts',(40.9288696352159,-2.80342531768405,0.));
#31061=CARTESIAN_POINT('Ctrl Pts',(41.0227421242398,-2.76949151194863,0.));
#31062=CARTESIAN_POINT('Ctrl Pts',(41.1165384061145,-2.73494956725006,0.));
#31063=CARTESIAN_POINT('Ctrl Pts',(41.2102568187956,-2.69980383625016,0.));
#31064=CARTESIAN_POINT('Ctrl Pts',(41.3038957096306,-2.66405934050118,0.));
#31065=CARTESIAN_POINT('Ctrl Pts',(41.3974534325936,-2.62772200460656,0.));
#31066=CARTESIAN_POINT('Ctrl Pts',(41.4909283577703,-2.59079818040172,0.));
#31067=CARTESIAN_POINT('Ctrl Pts',(41.5843188786284,-2.55329436064184,0.));
#31068=CARTESIAN_POINT('Ctrl Pts',(41.6776234194583,-2.51521684674477,0.));
#31069=CARTESIAN_POINT('Ctrl Pts',(41.7708404467532,-2.47657137427693,0.));
#31070=CARTESIAN_POINT('Ctrl Pts',(41.8639684667923,-2.43736301434201,0.));
#31071=CARTESIAN_POINT('Ctrl Pts',(41.9570060084039,-2.39759639399648,0.));
#31072=CARTESIAN_POINT('Ctrl Pts',(42.0499516093661,-2.35727584066429,0.));
#31073=CARTESIAN_POINT('Ctrl Pts',(42.1428038039937,-2.31640554742809,0.));
#31074=CARTESIAN_POINT('Ctrl Pts',(42.2355611060784,-2.27498976664775,0.));
#31075=CARTESIAN_POINT('Ctrl Pts',(42.3282220118033,-2.233032874655,0.));
#31076=CARTESIAN_POINT('Ctrl Pts',(42.4207850290047,-2.19053924976738,0.));
#31077=CARTESIAN_POINT('Ctrl Pts',(42.5132487024335,-2.14751319676745,0.));
#31078=CARTESIAN_POINT('Ctrl Pts',(42.6056116373455,-2.10395886401771,0.));
#31079=CARTESIAN_POINT('Ctrl Pts',(42.6978725343209,-2.05988014924519,0.));
#31080=CARTESIAN_POINT('Ctrl Pts',(42.7900301875309,-2.0152806752809,0.));
#31081=CARTESIAN_POINT('Ctrl Pts',(42.8820834139973,-1.97016390194216,0.));
#31082=CARTESIAN_POINT('Ctrl Pts',(42.9740309956624,-1.92453321512436,0.));
#31083=CARTESIAN_POINT('Ctrl Pts',(43.065871623255,-1.87839202014609,0.));
#31084=CARTESIAN_POINT('Ctrl Pts',(43.1576038253643,-1.83174385734712,0.));
#31085=CARTESIAN_POINT('Ctrl Pts',(43.2492259505872,-1.7845924484277,0.));
#31086=CARTESIAN_POINT('Ctrl Pts',(43.3407363140236,-1.73694151741124,0.));
#31087=CARTESIAN_POINT('Ctrl Pts',(43.4321333178711,-1.68879465270608,0.));
#31088=CARTESIAN_POINT('Ctrl Pts',(43.5234155788248,-1.64015515906648,0.));
#31089=CARTESIAN_POINT('Ctrl Pts',(43.6145820637333,-1.59102591108104,0.));
#31090=CARTESIAN_POINT('Ctrl Pts',(43.7238422193529,-1.53148589036097,0.));
#31091=CARTESIAN_POINT('Ctrl Pts',(43.8147465842502,-1.48126213998559,0.));
#31092=CARTESIAN_POINT('Ctrl Pts',(43.8873767449248,-1.44069595482723,0.));
#31093=CARTESIAN_POINT('Ctrl Pts',(43.9417969186811,-1.41005374202872,0.));
#31094=CARTESIAN_POINT('Ctrl Pts',(43.9780537249529,-1.38952890043916,0.));
#31095=CARTESIAN_POINT('',(36.199629211057,-3.39252545782466,0.));
#31096=CARTESIAN_POINT('',(35.2077250236291,-3.2995670413737,0.));
#31097=CARTESIAN_POINT('',(35.1136254352094,-4.26751599830831,0.));
#31098=CARTESIAN_POINT('Origin',(36.1063209411239,-4.38816272448461,0.));
#31099=CARTESIAN_POINT('Origin',(0.,0.,0.));
#31100=CARTESIAN_POINT('Origin',(0.,0.,0.));
#31101=CARTESIAN_POINT('Origin',(0.,0.,15.));
#31102=CARTESIAN_POINT('',(35.1136254352094,-4.26751599830831,15.));
#31103=CARTESIAN_POINT('Origin',(0.,0.,15.));
#31104=CARTESIAN_POINT('',(36.199629211057,-3.39252545782466,15.));
#31105=CARTESIAN_POINT('Origin',(36.1063209411239,-4.38816272448461,15.));
#31106=CARTESIAN_POINT('',(37.4237196983922,-3.50724370857673,15.));
#31107=CARTESIAN_POINT('',(35.2077250236291,-3.2995670413737,15.));
#31108=CARTESIAN_POINT('',(43.9780537249529,-1.38952890043916,15.));
#31109=CARTESIAN_POINT('Ctrl Pts',(37.4237196983922,-3.50724370857673,15.));
#31110=CARTESIAN_POINT('Ctrl Pts',(37.4426037737699,-3.50901346997657,15.));
#31111=CARTESIAN_POINT('Ctrl Pts',(37.4803889700239,-3.51204731876361,15.));
#31112=CARTESIAN_POINT('Ctrl Pts',(37.5371179004295,-3.5150810906521,15.));
#31113=CARTESIAN_POINT('Ctrl Pts',(37.6128545966533,-3.51624243734645,15.));
#31114=CARTESIAN_POINT('Ctrl Pts',(37.7076643105286,-3.51375922979957,15.));
#31115=CARTESIAN_POINT('Ctrl Pts',(37.8025803811856,-3.50844720825128,15.));
#31116=CARTESIAN_POINT('Ctrl Pts',(37.8975688353863,-3.50139628556084,15.));
#31117=CARTESIAN_POINT('Ctrl Pts',(37.9926009950482,-3.49340804454645,15.));
#31118=CARTESIAN_POINT('Ctrl Pts',(38.0876589224537,-3.48478279878233,15.));
#31119=CARTESIAN_POINT('Ctrl Pts',(38.1827321816559,-3.47549027265411,15.));
#31120=CARTESIAN_POINT('Ctrl Pts',(38.2778154909527,-3.46530185256872,15.));
#31121=CARTESIAN_POINT('Ctrl Pts',(38.3729061502716,-3.45393053211023,15.));
#31122=CARTESIAN_POINT('Ctrl Pts',(38.4680013094732,-3.44118343200303,15.));
#31123=CARTESIAN_POINT('Ctrl Pts',(38.5630961226878,-3.42705871084997,15.));
#31124=CARTESIAN_POINT('Ctrl Pts',(38.6581847668347,-3.41166717511901,15.));
#31125=CARTESIAN_POINT('Ctrl Pts',(38.7532609709905,-3.39518333281818,15.));
#31126=CARTESIAN_POINT('Ctrl Pts',(38.8483186930884,-3.37778863054482,15.));
#31127=CARTESIAN_POINT('Ctrl Pts',(38.9433528420174,-3.35960922799481,15.));
#31128=CARTESIAN_POINT('Ctrl Pts',(39.0383596151636,-3.34068601264472,15.));
#31129=CARTESIAN_POINT('Ctrl Pts',(39.1333360409949,-3.32100933979557,15.));
#31130=CARTESIAN_POINT('Ctrl Pts',(39.2282796893977,-3.30054018081687,15.));
#31131=CARTESIAN_POINT('Ctrl Pts',(39.3231883392913,-3.27923485388117,15.));
#31132=CARTESIAN_POINT('Ctrl Pts',(39.4180596080755,-3.25707264313388,15.));
#31133=CARTESIAN_POINT('Ctrl Pts',(39.5128908052622,-3.23406609691661,15.));
#31134=CARTESIAN_POINT('Ctrl Pts',(39.607679107639,-3.21024640045595,15.));
#31135=CARTESIAN_POINT('Ctrl Pts',(39.7024216585552,-3.18565465503835,15.));
#31136=CARTESIAN_POINT('Ctrl Pts',(39.7971156880138,-3.16033160752804,15.));
#31137=CARTESIAN_POINT('Ctrl Pts',(39.8917586491576,-3.13430604330356,15.));
#31138=CARTESIAN_POINT('Ctrl Pts',(39.9863482523153,-3.10759149802908,15.));
#31139=CARTESIAN_POINT('Ctrl Pts',(40.0808823811787,-3.08019251155015,15.));
#31140=CARTESIAN_POINT('Ctrl Pts',(40.1753590391515,-3.05210847423071,15.));
#31141=CARTESIAN_POINT('Ctrl Pts',(40.2697762886113,-3.02333808901595,15.));
#31142=CARTESIAN_POINT('Ctrl Pts',(40.3641321823444,-2.9938844645822,15.));
#31143=CARTESIAN_POINT('Ctrl Pts',(40.4584247445196,-2.96375636417323,15.));
#31144=CARTESIAN_POINT('Ctrl Pts',(40.5526520010651,-2.93296560822894,15.));
#31145=CARTESIAN_POINT('Ctrl Pts',(40.6468119976928,-2.90152548734343,15.));
#31146=CARTESIAN_POINT('Ctrl Pts',(40.7409028213129,-2.86944892209898,15.));
#31147=CARTESIAN_POINT('Ctrl Pts',(40.8349226258683,-2.83674635946679,15.));
#31148=CARTESIAN_POINT('Ctrl Pts',(40.9288696352159,-2.80342531768405,15.));
#31149=CARTESIAN_POINT('Ctrl Pts',(41.0227421242398,-2.76949151194863,15.));
#31150=CARTESIAN_POINT('Ctrl Pts',(41.1165384061145,-2.73494956725006,15.));
#31151=CARTESIAN_POINT('Ctrl Pts',(41.2102568187956,-2.69980383625016,15.));
#31152=CARTESIAN_POINT('Ctrl Pts',(41.3038957096306,-2.66405934050118,15.));
#31153=CARTESIAN_POINT('Ctrl Pts',(41.3974534325936,-2.62772200460656,15.));
#31154=CARTESIAN_POINT('Ctrl Pts',(41.4909283577703,-2.59079818040172,15.));
#31155=CARTESIAN_POINT('Ctrl Pts',(41.5843188786284,-2.55329436064184,15.));
#31156=CARTESIAN_POINT('Ctrl Pts',(41.6776234194583,-2.51521684674477,15.));
#31157=CARTESIAN_POINT('Ctrl Pts',(41.7708404467532,-2.47657137427693,15.));
#31158=CARTESIAN_POINT('Ctrl Pts',(41.8639684667923,-2.43736301434201,15.));
#31159=CARTESIAN_POINT('Ctrl Pts',(41.9570060084039,-2.39759639399648,15.));
#31160=CARTESIAN_POINT('Ctrl Pts',(42.0499516093661,-2.35727584066429,15.));
#31161=CARTESIAN_POINT('Ctrl Pts',(42.1428038039937,-2.31640554742809,15.));
#31162=CARTESIAN_POINT('Ctrl Pts',(42.2355611060784,-2.27498976664775,15.));
#31163=CARTESIAN_POINT('Ctrl Pts',(42.3282220118033,-2.233032874655,15.));
#31164=CARTESIAN_POINT('Ctrl Pts',(42.4207850290047,-2.19053924976738,15.));
#31165=CARTESIAN_POINT('Ctrl Pts',(42.5132487024335,-2.14751319676745,15.));
#31166=CARTESIAN_POINT('Ctrl Pts',(42.6056116373455,-2.10395886401771,15.));
#31167=CARTESIAN_POINT('Ctrl Pts',(42.6978725343209,-2.05988014924519,15.));
#31168=CARTESIAN_POINT('Ctrl Pts',(42.7900301875309,-2.0152806752809,15.));
#31169=CARTESIAN_POINT('Ctrl Pts',(42.8820834139973,-1.97016390194216,15.));
#31170=CARTESIAN_POINT('Ctrl Pts',(42.9740309956624,-1.92453321512436,15.));
#31171=CARTESIAN_POINT('Ctrl Pts',(43.065871623255,-1.87839202014609,15.));
#31172=CARTESIAN_POINT('Ctrl Pts',(43.1576038253643,-1.83174385734712,15.));
#31173=CARTESIAN_POINT('Ctrl Pts',(43.2492259505872,-1.7845924484277,15.));
#31174=CARTESIAN_POINT('Ctrl Pts',(43.3407363140236,-1.73694151741124,15.));
#31175=CARTESIAN_POINT('Ctrl Pts',(43.4321333178711,-1.68879465270608,15.));
#31176=CARTESIAN_POINT('Ctrl Pts',(43.5234155788248,-1.64015515906648,15.));
#31177=CARTESIAN_POINT('Ctrl Pts',(43.6145820637333,-1.59102591108104,15.));
#31178=CARTESIAN_POINT('Ctrl Pts',(43.7238422193529,-1.53148589036097,15.));
#31179=CARTESIAN_POINT('Ctrl Pts',(43.8147465842502,-1.48126213998559,15.));
#31180=CARTESIAN_POINT('Ctrl Pts',(43.8873767449248,-1.44069595482723,15.));
#31181=CARTESIAN_POINT('Ctrl Pts',(43.9417969186811,-1.41005374202872,15.));
#31182=CARTESIAN_POINT('Ctrl Pts',(43.9780537249529,-1.38952890043916,15.));
#31183=CARTESIAN_POINT('',(43.9780537249529,1.38952890043929,15.));
#31184=CARTESIAN_POINT('Origin',(1.13331566353736E-11,0.,15.));
#31185=CARTESIAN_POINT('',(37.4237196983922,3.50724370857673,15.));
#31186=CARTESIAN_POINT('Ctrl Pts',(43.9780537249529,1.38952890043916,15.));
#31187=CARTESIAN_POINT('Ctrl Pts',(43.9599253218251,1.39979132121931,15.));
#31188=CARTESIAN_POINT('Ctrl Pts',(43.9236568607623,1.42026781296156,15.));
#31189=CARTESIAN_POINT('Ctrl Pts',(43.8692192047561,1.45083750111682,15.));
#31190=CARTESIAN_POINT('Ctrl Pts',(43.7965657112707,1.49130689006067,15.));
#31191=CARTESIAN_POINT('Ctrl Pts',(43.7056321934163,1.54140922714765,15.));
#31192=CARTESIAN_POINT('Ctrl Pts',(43.6145820637333,1.59102591108104,15.));
#31193=CARTESIAN_POINT('Ctrl Pts',(43.5234155788248,1.64015515906648,15.));
#31194=CARTESIAN_POINT('Ctrl Pts',(43.4321333178711,1.68879465270608,15.));
#31195=CARTESIAN_POINT('Ctrl Pts',(43.3407363140236,1.73694151741124,15.));
#31196=CARTESIAN_POINT('Ctrl Pts',(43.2492259505872,1.7845924484277,15.));
#31197=CARTESIAN_POINT('Ctrl Pts',(43.1576038253643,1.83174385734712,15.));
#31198=CARTESIAN_POINT('Ctrl Pts',(43.065871623255,1.87839202014609,15.));
#31199=CARTESIAN_POINT('Ctrl Pts',(42.9740309956624,1.92453321512436,15.));
#31200=CARTESIAN_POINT('Ctrl Pts',(42.8820834139973,1.97016390194216,15.));
#31201=CARTESIAN_POINT('Ctrl Pts',(42.7900301875309,2.0152806752809,15.));
#31202=CARTESIAN_POINT('Ctrl Pts',(42.6978725343209,2.05988014924519,15.));
#31203=CARTESIAN_POINT('Ctrl Pts',(42.6056116373455,2.10395886401771,15.));
#31204=CARTESIAN_POINT('Ctrl Pts',(42.5132487024335,2.14751319676745,15.));
#31205=CARTESIAN_POINT('Ctrl Pts',(42.4207850290047,2.19053924976738,15.));
#31206=CARTESIAN_POINT('Ctrl Pts',(42.3282220118033,2.233032874655,15.));
#31207=CARTESIAN_POINT('Ctrl Pts',(42.2355611060784,2.27498976664775,15.));
#31208=CARTESIAN_POINT('Ctrl Pts',(42.1428038039937,2.31640554742809,15.));
#31209=CARTESIAN_POINT('Ctrl Pts',(42.0499516093661,2.35727584066429,15.));
#31210=CARTESIAN_POINT('Ctrl Pts',(41.9570060084039,2.39759639399648,15.));
#31211=CARTESIAN_POINT('Ctrl Pts',(41.8639684667923,2.43736301434201,15.));
#31212=CARTESIAN_POINT('Ctrl Pts',(41.7708404467532,2.47657137427693,15.));
#31213=CARTESIAN_POINT('Ctrl Pts',(41.6776234194583,2.51521684674477,15.));
#31214=CARTESIAN_POINT('Ctrl Pts',(41.5843188786284,2.55329436064184,15.));
#31215=CARTESIAN_POINT('Ctrl Pts',(41.4909283577703,2.59079818040172,15.));
#31216=CARTESIAN_POINT('Ctrl Pts',(41.3974534325936,2.62772200460656,15.));
#31217=CARTESIAN_POINT('Ctrl Pts',(41.3038957096306,2.66405934050118,15.));
#31218=CARTESIAN_POINT('Ctrl Pts',(41.2102568187956,2.69980383625016,15.));
#31219=CARTESIAN_POINT('Ctrl Pts',(41.1165384061145,2.73494956725006,15.));
#31220=CARTESIAN_POINT('Ctrl Pts',(41.0227421242398,2.76949151194863,15.));
#31221=CARTESIAN_POINT('Ctrl Pts',(40.9288696352159,2.80342531768405,15.));
#31222=CARTESIAN_POINT('Ctrl Pts',(40.8349226258683,2.83674635946679,15.));
#31223=CARTESIAN_POINT('Ctrl Pts',(40.7409028213129,2.86944892209898,15.));
#31224=CARTESIAN_POINT('Ctrl Pts',(40.6468119976928,2.90152548734343,15.));
#31225=CARTESIAN_POINT('Ctrl Pts',(40.5526520010651,2.93296560822894,15.));
#31226=CARTESIAN_POINT('Ctrl Pts',(40.4584247445196,2.96375636417323,15.));
#31227=CARTESIAN_POINT('Ctrl Pts',(40.3641321823444,2.9938844645822,15.));
#31228=CARTESIAN_POINT('Ctrl Pts',(40.2697762886113,3.02333808901595,15.));
#31229=CARTESIAN_POINT('Ctrl Pts',(40.1753590391515,3.05210847423071,15.));
#31230=CARTESIAN_POINT('Ctrl Pts',(40.0808823811787,3.08019251155015,15.));
#31231=CARTESIAN_POINT('Ctrl Pts',(39.9863482523153,3.10759149802908,15.));
#31232=CARTESIAN_POINT('Ctrl Pts',(39.8917586491576,3.13430604330356,15.));
#31233=CARTESIAN_POINT('Ctrl Pts',(39.7971156880138,3.16033160752804,15.));
#31234=CARTESIAN_POINT('Ctrl Pts',(39.7024216585552,3.18565465503835,15.));
#31235=CARTESIAN_POINT('Ctrl Pts',(39.607679107639,3.21024640045595,15.));
#31236=CARTESIAN_POINT('Ctrl Pts',(39.5128908052622,3.23406609691661,15.));
#31237=CARTESIAN_POINT('Ctrl Pts',(39.4180596080755,3.25707264313388,15.));
#31238=CARTESIAN_POINT('Ctrl Pts',(39.3231883392913,3.27923485388117,15.));
#31239=CARTESIAN_POINT('Ctrl Pts',(39.2282796893977,3.30054018081687,15.));
#31240=CARTESIAN_POINT('Ctrl Pts',(39.1333360409949,3.32100933979557,15.));
#31241=CARTESIAN_POINT('Ctrl Pts',(39.0383596151636,3.34068601264472,15.));
#31242=CARTESIAN_POINT('Ctrl Pts',(38.9433528420174,3.35960922799481,15.));
#31243=CARTESIAN_POINT('Ctrl Pts',(38.8483186930884,3.37778863054482,15.));
#31244=CARTESIAN_POINT('Ctrl Pts',(38.7532609709905,3.39518333281818,15.));
#31245=CARTESIAN_POINT('Ctrl Pts',(38.6581847668347,3.41166717511901,15.));
#31246=CARTESIAN_POINT('Ctrl Pts',(38.5630961226878,3.42705871084997,15.));
#31247=CARTESIAN_POINT('Ctrl Pts',(38.4680013094732,3.44118343200303,15.));
#31248=CARTESIAN_POINT('Ctrl Pts',(38.3729061502716,3.45393053211023,15.));
#31249=CARTESIAN_POINT('Ctrl Pts',(38.2778154909527,3.46530185256872,15.));
#31250=CARTESIAN_POINT('Ctrl Pts',(38.1827321816559,3.47549027265411,15.));
#31251=CARTESIAN_POINT('Ctrl Pts',(38.0876589224537,3.48478279878233,15.));
#31252=CARTESIAN_POINT('Ctrl Pts',(37.9926009950482,3.49340804454645,15.));
#31253=CARTESIAN_POINT('Ctrl Pts',(37.8975688353863,3.50139628556084,15.));
#31254=CARTESIAN_POINT('Ctrl Pts',(37.8025803811856,3.50844720825128,15.));
#31255=CARTESIAN_POINT('Ctrl Pts',(37.7076643105286,3.51375922979957,15.));
#31256=CARTESIAN_POINT('Ctrl Pts',(37.6128545966533,3.51624243734645,15.));
#31257=CARTESIAN_POINT('Ctrl Pts',(37.5371179004295,3.5150810906521,15.));
#31258=CARTESIAN_POINT('Ctrl Pts',(37.4803889700239,3.51204731876361,15.));
#31259=CARTESIAN_POINT('Ctrl Pts',(37.4426037737699,3.50901346997657,15.));
#31260=CARTESIAN_POINT('Ctrl Pts',(37.4237196983922,3.50724370857673,15.));
#31261=CARTESIAN_POINT('',(36.199629211057,3.39252545782466,15.));
#31262=CARTESIAN_POINT('',(35.2077250236291,3.2995670413737,15.));
#31263=CARTESIAN_POINT('',(35.1136254352094,4.26751599830831,15.));
#31264=CARTESIAN_POINT('Origin',(36.1063209411239,4.38816272448461,15.));
#31265=CARTESIAN_POINT('Origin',(0.,0.,15.));
#31266=CARTESIAN_POINT('Origin',(0.,0.,15.));
#31267=CARTESIAN_POINT('Origin',(0.,0.,15.));
#31268=CARTESIAN_POINT('Origin',(0.,0.,15.));
#31269=CARTESIAN_POINT('Origin',(0.,0.,15.));
#31270=CARTESIAN_POINT('Origin',(0.,0.,15.));
#31271=CARTESIAN_POINT('Origin',(0.,0.,15.));
#31272=CARTESIAN_POINT('Origin',(0.,0.,15.));
#31273=CARTESIAN_POINT('Origin',(0.,0.,15.));
#31274=CARTESIAN_POINT('Origin',(0.,0.,15.));
#31275=CARTESIAN_POINT('Origin',(0.,0.,15.));
#31276=CARTESIAN_POINT('Origin',(0.,0.,15.));
#31277=CARTESIAN_POINT('Origin',(0.,0.,15.));
#31278=CARTESIAN_POINT('Origin',(0.,0.,15.));
#31279=CARTESIAN_POINT('Origin',(0.,0.,15.));
#31280=CARTESIAN_POINT('Origin',(0.,0.,15.));
#31281=CARTESIAN_POINT('Origin',(0.,0.,15.));
#31282=CARTESIAN_POINT('Origin',(0.,0.,15.));
#31283=CARTESIAN_POINT('Origin',(0.,0.,15.));
#31284=CARTESIAN_POINT('Origin',(0.,0.,0.));
#31285=CARTESIAN_POINT('',(35.1136254352094,4.26751599830831,0.));
#31286=CARTESIAN_POINT('Origin',(0.,0.,0.));
#31287=CARTESIAN_POINT('Origin',(0.,0.,0.));
#31288=CARTESIAN_POINT('Origin',(0.,0.,0.));
#31289=CARTESIAN_POINT('Origin',(0.,0.,0.));
#31290=CARTESIAN_POINT('Origin',(0.,0.,0.));
#31291=CARTESIAN_POINT('Origin',(0.,0.,0.));
#31292=CARTESIAN_POINT('Origin',(0.,0.,0.));
#31293=CARTESIAN_POINT('Origin',(0.,0.,0.));
#31294=CARTESIAN_POINT('Origin',(0.,0.,0.));
#31295=CARTESIAN_POINT('Origin',(0.,0.,0.));
#31296=CARTESIAN_POINT('Origin',(0.,0.,0.));
#31297=CARTESIAN_POINT('Origin',(0.,0.,0.));
#31298=CARTESIAN_POINT('Origin',(0.,0.,0.));
#31299=CARTESIAN_POINT('Origin',(0.,0.,0.));
#31300=CARTESIAN_POINT('Origin',(0.,0.,0.));
#31301=CARTESIAN_POINT('Origin',(0.,0.,0.));
#31302=CARTESIAN_POINT('Origin',(0.,0.,0.));
#31303=CARTESIAN_POINT('Origin',(0.,0.,0.));
#31304=CARTESIAN_POINT('Origin',(36.1063209411239,4.38816272448461,0.));
#31305=CARTESIAN_POINT('',(36.199629211057,3.39252545782466,0.));
#31306=CARTESIAN_POINT('Origin',(37.4237196983922,3.50724370857673,0.));
#31307=CARTESIAN_POINT('',(37.4237196983922,3.50724370857673,0.));
#31308=CARTESIAN_POINT('Origin',(36.1063209411239,-4.38816272448461,0.));
#31309=CARTESIAN_POINT('',(36.199629211057,-3.39252545782466,0.));
#31310=CARTESIAN_POINT('',(35.1136254352094,-4.26751599830831,0.));
#31311=CARTESIAN_POINT('Origin',(35.2077250236291,-3.2995670413737,0.));
#31312=CARTESIAN_POINT('',(37.4237196983922,-3.50724370857673,0.));
#31313=CARTESIAN_POINT('Ctrl Pts',(43.9780537249529,1.38952890043916,0.));
#31314=CARTESIAN_POINT('Ctrl Pts',(43.9780537249529,1.38952890043916,18.));
#31315=CARTESIAN_POINT('Ctrl Pts',(43.9599253218251,1.39979132121931,0.));
#31316=CARTESIAN_POINT('Ctrl Pts',(43.9599253218251,1.39979132121931,18.));
#31317=CARTESIAN_POINT('Ctrl Pts',(43.9236568607623,1.42026781296156,0.));
#31318=CARTESIAN_POINT('Ctrl Pts',(43.9236568607623,1.42026781296156,18.));
#31319=CARTESIAN_POINT('Ctrl Pts',(43.8692192047561,1.45083750111682,0.));
#31320=CARTESIAN_POINT('Ctrl Pts',(43.8692192047561,1.45083750111682,18.));
#31321=CARTESIAN_POINT('Ctrl Pts',(43.7965657112707,1.49130689006067,0.));
#31322=CARTESIAN_POINT('Ctrl Pts',(43.7965657112707,1.49130689006067,18.));
#31323=CARTESIAN_POINT('Ctrl Pts',(43.7056321934163,1.54140922714765,0.));
#31324=CARTESIAN_POINT('Ctrl Pts',(43.7056321934163,1.54140922714765,18.));
#31325=CARTESIAN_POINT('Ctrl Pts',(43.6145820637333,1.59102591108104,0.));
#31326=CARTESIAN_POINT('Ctrl Pts',(43.6145820637333,1.59102591108104,18.));
#31327=CARTESIAN_POINT('Ctrl Pts',(43.5234155788248,1.64015515906648,0.));
#31328=CARTESIAN_POINT('Ctrl Pts',(43.5234155788248,1.64015515906648,18.));
#31329=CARTESIAN_POINT('Ctrl Pts',(43.4321333178711,1.68879465270608,0.));
#31330=CARTESIAN_POINT('Ctrl Pts',(43.4321333178711,1.68879465270608,18.));
#31331=CARTESIAN_POINT('Ctrl Pts',(43.3407363140236,1.73694151741124,0.));
#31332=CARTESIAN_POINT('Ctrl Pts',(43.3407363140236,1.73694151741124,18.));
#31333=CARTESIAN_POINT('Ctrl Pts',(43.2492259505872,1.7845924484277,0.));
#31334=CARTESIAN_POINT('Ctrl Pts',(43.2492259505872,1.7845924484277,18.));
#31335=CARTESIAN_POINT('Ctrl Pts',(43.1576038253643,1.83174385734712,0.));
#31336=CARTESIAN_POINT('Ctrl Pts',(43.1576038253643,1.83174385734712,18.));
#31337=CARTESIAN_POINT('Ctrl Pts',(43.065871623255,1.87839202014609,0.));
#31338=CARTESIAN_POINT('Ctrl Pts',(43.065871623255,1.87839202014609,18.));
#31339=CARTESIAN_POINT('Ctrl Pts',(42.9740309956624,1.92453321512436,0.));
#31340=CARTESIAN_POINT('Ctrl Pts',(42.9740309956624,1.92453321512436,18.));
#31341=CARTESIAN_POINT('Ctrl Pts',(42.8820834139973,1.97016390194216,0.));
#31342=CARTESIAN_POINT('Ctrl Pts',(42.8820834139973,1.97016390194216,18.));
#31343=CARTESIAN_POINT('Ctrl Pts',(42.7900301875309,2.0152806752809,0.));
#31344=CARTESIAN_POINT('Ctrl Pts',(42.7900301875309,2.0152806752809,18.));
#31345=CARTESIAN_POINT('Ctrl Pts',(42.6978725343209,2.05988014924519,0.));
#31346=CARTESIAN_POINT('Ctrl Pts',(42.6978725343209,2.05988014924519,18.));
#31347=CARTESIAN_POINT('Ctrl Pts',(42.6056116373455,2.10395886401771,0.));
#31348=CARTESIAN_POINT('Ctrl Pts',(42.6056116373455,2.10395886401771,18.));
#31349=CARTESIAN_POINT('Ctrl Pts',(42.5132487024335,2.14751319676745,0.));
#31350=CARTESIAN_POINT('Ctrl Pts',(42.5132487024335,2.14751319676745,18.));
#31351=CARTESIAN_POINT('Ctrl Pts',(42.4207850290047,2.19053924976738,0.));
#31352=CARTESIAN_POINT('Ctrl Pts',(42.4207850290047,2.19053924976738,18.));
#31353=CARTESIAN_POINT('Ctrl Pts',(42.3282220118033,2.233032874655,0.));
#31354=CARTESIAN_POINT('Ctrl Pts',(42.3282220118033,2.233032874655,18.));
#31355=CARTESIAN_POINT('Ctrl Pts',(42.2355611060784,2.27498976664775,0.));
#31356=CARTESIAN_POINT('Ctrl Pts',(42.2355611060784,2.27498976664775,18.));
#31357=CARTESIAN_POINT('Ctrl Pts',(42.1428038039937,2.31640554742809,0.));
#31358=CARTESIAN_POINT('Ctrl Pts',(42.1428038039937,2.31640554742809,18.));
#31359=CARTESIAN_POINT('Ctrl Pts',(42.0499516093661,2.35727584066429,0.));
#31360=CARTESIAN_POINT('Ctrl Pts',(42.0499516093661,2.35727584066429,18.));
#31361=CARTESIAN_POINT('Ctrl Pts',(41.9570060084039,2.39759639399648,0.));
#31362=CARTESIAN_POINT('Ctrl Pts',(41.9570060084039,2.39759639399648,18.));
#31363=CARTESIAN_POINT('Ctrl Pts',(41.8639684667923,2.43736301434201,0.));
#31364=CARTESIAN_POINT('Ctrl Pts',(41.8639684667923,2.43736301434201,18.));
#31365=CARTESIAN_POINT('Ctrl Pts',(41.7708404467532,2.47657137427693,0.));
#31366=CARTESIAN_POINT('Ctrl Pts',(41.7708404467532,2.47657137427693,18.));
#31367=CARTESIAN_POINT('Ctrl Pts',(41.6776234194583,2.51521684674477,0.));
#31368=CARTESIAN_POINT('Ctrl Pts',(41.6776234194583,2.51521684674477,18.));
#31369=CARTESIAN_POINT('Ctrl Pts',(41.5843188786284,2.55329436064184,0.));
#31370=CARTESIAN_POINT('Ctrl Pts',(41.5843188786284,2.55329436064184,18.));
#31371=CARTESIAN_POINT('Ctrl Pts',(41.4909283577703,2.59079818040172,0.));
#31372=CARTESIAN_POINT('Ctrl Pts',(41.4909283577703,2.59079818040172,18.));
#31373=CARTESIAN_POINT('Ctrl Pts',(41.3974534325936,2.62772200460656,0.));
#31374=CARTESIAN_POINT('Ctrl Pts',(41.3974534325936,2.62772200460656,18.));
#31375=CARTESIAN_POINT('Ctrl Pts',(41.3038957096306,2.66405934050118,0.));
#31376=CARTESIAN_POINT('Ctrl Pts',(41.3038957096306,2.66405934050118,18.));
#31377=CARTESIAN_POINT('Ctrl Pts',(41.2102568187956,2.69980383625016,0.));
#31378=CARTESIAN_POINT('Ctrl Pts',(41.2102568187956,2.69980383625016,18.));
#31379=CARTESIAN_POINT('Ctrl Pts',(41.1165384061145,2.73494956725006,0.));
#31380=CARTESIAN_POINT('Ctrl Pts',(41.1165384061145,2.73494956725006,18.));
#31381=CARTESIAN_POINT('Ctrl Pts',(41.0227421242398,2.76949151194863,0.));
#31382=CARTESIAN_POINT('Ctrl Pts',(41.0227421242398,2.76949151194863,18.));
#31383=CARTESIAN_POINT('Ctrl Pts',(40.9288696352159,2.80342531768405,0.));
#31384=CARTESIAN_POINT('Ctrl Pts',(40.9288696352159,2.80342531768405,18.));
#31385=CARTESIAN_POINT('Ctrl Pts',(40.8349226258683,2.83674635946679,0.));
#31386=CARTESIAN_POINT('Ctrl Pts',(40.8349226258683,2.83674635946679,18.));
#31387=CARTESIAN_POINT('Ctrl Pts',(40.7409028213129,2.86944892209898,0.));
#31388=CARTESIAN_POINT('Ctrl Pts',(40.7409028213129,2.86944892209898,18.));
#31389=CARTESIAN_POINT('Ctrl Pts',(40.6468119976928,2.90152548734343,0.));
#31390=CARTESIAN_POINT('Ctrl Pts',(40.6468119976928,2.90152548734343,18.));
#31391=CARTESIAN_POINT('Ctrl Pts',(40.5526520010651,2.93296560822894,0.));
#31392=CARTESIAN_POINT('Ctrl Pts',(40.5526520010651,2.93296560822894,18.));
#31393=CARTESIAN_POINT('Ctrl Pts',(40.4584247445196,2.96375636417323,0.));
#31394=CARTESIAN_POINT('Ctrl Pts',(40.4584247445196,2.96375636417323,18.));
#31395=CARTESIAN_POINT('Ctrl Pts',(40.3641321823444,2.9938844645822,0.));
#31396=CARTESIAN_POINT('Ctrl Pts',(40.3641321823444,2.9938844645822,18.));
#31397=CARTESIAN_POINT('Ctrl Pts',(40.2697762886113,3.02333808901595,0.));
#31398=CARTESIAN_POINT('Ctrl Pts',(40.2697762886113,3.02333808901595,18.));
#31399=CARTESIAN_POINT('Ctrl Pts',(40.1753590391515,3.05210847423071,0.));
#31400=CARTESIAN_POINT('Ctrl Pts',(40.1753590391515,3.05210847423071,18.));
#31401=CARTESIAN_POINT('Ctrl Pts',(40.0808823811787,3.08019251155015,0.));
#31402=CARTESIAN_POINT('Ctrl Pts',(40.0808823811787,3.08019251155015,18.));
#31403=CARTESIAN_POINT('Ctrl Pts',(39.9863482523153,3.10759149802908,0.));
#31404=CARTESIAN_POINT('Ctrl Pts',(39.9863482523153,3.10759149802908,18.));
#31405=CARTESIAN_POINT('Ctrl Pts',(39.8917586491576,3.13430604330356,0.));
#31406=CARTESIAN_POINT('Ctrl Pts',(39.8917586491576,3.13430604330356,18.));
#31407=CARTESIAN_POINT('Ctrl Pts',(39.7971156880138,3.16033160752804,0.));
#31408=CARTESIAN_POINT('Ctrl Pts',(39.7971156880138,3.16033160752804,18.));
#31409=CARTESIAN_POINT('Ctrl Pts',(39.7024216585552,3.18565465503835,0.));
#31410=CARTESIAN_POINT('Ctrl Pts',(39.7024216585552,3.18565465503835,18.));
#31411=CARTESIAN_POINT('Ctrl Pts',(39.607679107639,3.21024640045595,0.));
#31412=CARTESIAN_POINT('Ctrl Pts',(39.607679107639,3.21024640045595,18.));
#31413=CARTESIAN_POINT('Ctrl Pts',(39.5128908052622,3.23406609691661,0.));
#31414=CARTESIAN_POINT('Ctrl Pts',(39.5128908052622,3.23406609691661,18.));
#31415=CARTESIAN_POINT('Ctrl Pts',(39.4180596080755,3.25707264313388,0.));
#31416=CARTESIAN_POINT('Ctrl Pts',(39.4180596080755,3.25707264313388,18.));
#31417=CARTESIAN_POINT('Ctrl Pts',(39.3231883392913,3.27923485388117,0.));
#31418=CARTESIAN_POINT('Ctrl Pts',(39.3231883392913,3.27923485388117,18.));
#31419=CARTESIAN_POINT('Ctrl Pts',(39.2282796893977,3.30054018081687,0.));
#31420=CARTESIAN_POINT('Ctrl Pts',(39.2282796893977,3.30054018081687,18.));
#31421=CARTESIAN_POINT('Ctrl Pts',(39.1333360409949,3.32100933979557,0.));
#31422=CARTESIAN_POINT('Ctrl Pts',(39.1333360409949,3.32100933979557,18.));
#31423=CARTESIAN_POINT('Ctrl Pts',(39.0383596151636,3.34068601264472,0.));
#31424=CARTESIAN_POINT('Ctrl Pts',(39.0383596151636,3.34068601264472,18.));
#31425=CARTESIAN_POINT('Ctrl Pts',(38.9433528420174,3.35960922799481,0.));
#31426=CARTESIAN_POINT('Ctrl Pts',(38.9433528420174,3.35960922799481,18.));
#31427=CARTESIAN_POINT('Ctrl Pts',(38.8483186930884,3.37778863054482,0.));
#31428=CARTESIAN_POINT('Ctrl Pts',(38.8483186930884,3.37778863054482,18.));
#31429=CARTESIAN_POINT('Ctrl Pts',(38.7532609709905,3.39518333281818,0.));
#31430=CARTESIAN_POINT('Ctrl Pts',(38.7532609709905,3.39518333281818,18.));
#31431=CARTESIAN_POINT('Ctrl Pts',(38.6581847668347,3.41166717511901,0.));
#31432=CARTESIAN_POINT('Ctrl Pts',(38.6581847668347,3.41166717511901,18.));
#31433=CARTESIAN_POINT('Ctrl Pts',(38.5630961226878,3.42705871084997,0.));
#31434=CARTESIAN_POINT('Ctrl Pts',(38.5630961226878,3.42705871084997,18.));
#31435=CARTESIAN_POINT('Ctrl Pts',(38.4680013094732,3.44118343200303,0.));
#31436=CARTESIAN_POINT('Ctrl Pts',(38.4680013094732,3.44118343200303,18.));
#31437=CARTESIAN_POINT('Ctrl Pts',(38.3729061502716,3.45393053211023,0.));
#31438=CARTESIAN_POINT('Ctrl Pts',(38.3729061502716,3.45393053211023,18.));
#31439=CARTESIAN_POINT('Ctrl Pts',(38.2778154909527,3.46530185256872,0.));
#31440=CARTESIAN_POINT('Ctrl Pts',(38.2778154909527,3.46530185256872,18.));
#31441=CARTESIAN_POINT('Ctrl Pts',(38.1827321816559,3.47549027265411,0.));
#31442=CARTESIAN_POINT('Ctrl Pts',(38.1827321816559,3.47549027265411,18.));
#31443=CARTESIAN_POINT('Ctrl Pts',(38.0876589224537,3.48478279878233,0.));
#31444=CARTESIAN_POINT('Ctrl Pts',(38.0876589224537,3.48478279878233,18.));
#31445=CARTESIAN_POINT('Ctrl Pts',(37.9926009950482,3.49340804454645,0.));
#31446=CARTESIAN_POINT('Ctrl Pts',(37.9926009950482,3.49340804454645,18.));
#31447=CARTESIAN_POINT('Ctrl Pts',(37.8975688353863,3.50139628556084,0.));
#31448=CARTESIAN_POINT('Ctrl Pts',(37.8975688353863,3.50139628556084,18.));
#31449=CARTESIAN_POINT('Ctrl Pts',(37.8025803811856,3.50844720825128,0.));
#31450=CARTESIAN_POINT('Ctrl Pts',(37.8025803811856,3.50844720825128,18.));
#31451=CARTESIAN_POINT('Ctrl Pts',(37.7076643105286,3.51375922979957,0.));
#31452=CARTESIAN_POINT('Ctrl Pts',(37.7076643105286,3.51375922979957,18.));
#31453=CARTESIAN_POINT('Ctrl Pts',(37.6128545966533,3.51624243734645,0.));
#31454=CARTESIAN_POINT('Ctrl Pts',(37.6128545966533,3.51624243734645,18.));
#31455=CARTESIAN_POINT('Ctrl Pts',(37.5371179004295,3.5150810906521,0.));
#31456=CARTESIAN_POINT('Ctrl Pts',(37.5371179004295,3.5150810906521,18.));
#31457=CARTESIAN_POINT('Ctrl Pts',(37.4803889700239,3.51204731876361,0.));
#31458=CARTESIAN_POINT('Ctrl Pts',(37.4803889700239,3.51204731876361,18.));
#31459=CARTESIAN_POINT('Ctrl Pts',(37.4426037737699,3.50901346997657,0.));
#31460=CARTESIAN_POINT('Ctrl Pts',(37.4426037737699,3.50901346997657,18.));
#31461=CARTESIAN_POINT('Ctrl Pts',(37.4237196983922,3.50724370857673,0.));
#31462=CARTESIAN_POINT('Ctrl Pts',(37.4237196983922,3.50724370857673,18.));
#31463=CARTESIAN_POINT('',(43.9780537249529,1.38952890043929,0.));
#31464=CARTESIAN_POINT('Origin',(1.13331566353736E-11,0.,0.));
#31465=CARTESIAN_POINT('',(43.9780537249529,-1.38952890043916,0.));
#31466=CARTESIAN_POINT('Ctrl Pts',(37.4237196983922,-3.50724370857673,0.));
#31467=CARTESIAN_POINT('Ctrl Pts',(37.4237196983922,-3.50724370857673,18.));
#31468=CARTESIAN_POINT('Ctrl Pts',(37.4426037737699,-3.50901346997657,0.));
#31469=CARTESIAN_POINT('Ctrl Pts',(37.4426037737699,-3.50901346997657,18.));
#31470=CARTESIAN_POINT('Ctrl Pts',(37.4803889700239,-3.51204731876361,0.));
#31471=CARTESIAN_POINT('Ctrl Pts',(37.4803889700239,-3.51204731876361,18.));
#31472=CARTESIAN_POINT('Ctrl Pts',(37.5371179004295,-3.5150810906521,0.));
#31473=CARTESIAN_POINT('Ctrl Pts',(37.5371179004295,-3.5150810906521,18.));
#31474=CARTESIAN_POINT('Ctrl Pts',(37.6128545966533,-3.51624243734645,0.));
#31475=CARTESIAN_POINT('Ctrl Pts',(37.6128545966533,-3.51624243734645,18.));
#31476=CARTESIAN_POINT('Ctrl Pts',(37.7076643105286,-3.51375922979957,0.));
#31477=CARTESIAN_POINT('Ctrl Pts',(37.7076643105286,-3.51375922979957,18.));
#31478=CARTESIAN_POINT('Ctrl Pts',(37.8025803811856,-3.50844720825128,0.));
#31479=CARTESIAN_POINT('Ctrl Pts',(37.8025803811856,-3.50844720825128,18.));
#31480=CARTESIAN_POINT('Ctrl Pts',(37.8975688353863,-3.50139628556084,0.));
#31481=CARTESIAN_POINT('Ctrl Pts',(37.8975688353863,-3.50139628556084,18.));
#31482=CARTESIAN_POINT('Ctrl Pts',(37.9926009950482,-3.49340804454645,0.));
#31483=CARTESIAN_POINT('Ctrl Pts',(37.9926009950482,-3.49340804454645,18.));
#31484=CARTESIAN_POINT('Ctrl Pts',(38.0876589224537,-3.48478279878233,0.));
#31485=CARTESIAN_POINT('Ctrl Pts',(38.0876589224537,-3.48478279878233,18.));
#31486=CARTESIAN_POINT('Ctrl Pts',(38.1827321816559,-3.47549027265411,0.));
#31487=CARTESIAN_POINT('Ctrl Pts',(38.1827321816559,-3.47549027265411,18.));
#31488=CARTESIAN_POINT('Ctrl Pts',(38.2778154909527,-3.46530185256872,0.));
#31489=CARTESIAN_POINT('Ctrl Pts',(38.2778154909527,-3.46530185256872,18.));
#31490=CARTESIAN_POINT('Ctrl Pts',(38.3729061502716,-3.45393053211023,0.));
#31491=CARTESIAN_POINT('Ctrl Pts',(38.3729061502716,-3.45393053211023,18.));
#31492=CARTESIAN_POINT('Ctrl Pts',(38.4680013094732,-3.44118343200303,0.));
#31493=CARTESIAN_POINT('Ctrl Pts',(38.4680013094732,-3.44118343200303,18.));
#31494=CARTESIAN_POINT('Ctrl Pts',(38.5630961226878,-3.42705871084997,0.));
#31495=CARTESIAN_POINT('Ctrl Pts',(38.5630961226878,-3.42705871084997,18.));
#31496=CARTESIAN_POINT('Ctrl Pts',(38.6581847668347,-3.41166717511901,0.));
#31497=CARTESIAN_POINT('Ctrl Pts',(38.6581847668347,-3.41166717511901,18.));
#31498=CARTESIAN_POINT('Ctrl Pts',(38.7532609709905,-3.39518333281818,0.));
#31499=CARTESIAN_POINT('Ctrl Pts',(38.7532609709905,-3.39518333281818,18.));
#31500=CARTESIAN_POINT('Ctrl Pts',(38.8483186930884,-3.37778863054482,0.));
#31501=CARTESIAN_POINT('Ctrl Pts',(38.8483186930884,-3.37778863054482,18.));
#31502=CARTESIAN_POINT('Ctrl Pts',(38.9433528420174,-3.35960922799481,0.));
#31503=CARTESIAN_POINT('Ctrl Pts',(38.9433528420174,-3.35960922799481,18.));
#31504=CARTESIAN_POINT('Ctrl Pts',(39.0383596151636,-3.34068601264472,0.));
#31505=CARTESIAN_POINT('Ctrl Pts',(39.0383596151636,-3.34068601264472,18.));
#31506=CARTESIAN_POINT('Ctrl Pts',(39.1333360409949,-3.32100933979557,0.));
#31507=CARTESIAN_POINT('Ctrl Pts',(39.1333360409949,-3.32100933979557,18.));
#31508=CARTESIAN_POINT('Ctrl Pts',(39.2282796893977,-3.30054018081687,0.));
#31509=CARTESIAN_POINT('Ctrl Pts',(39.2282796893977,-3.30054018081687,18.));
#31510=CARTESIAN_POINT('Ctrl Pts',(39.3231883392913,-3.27923485388117,0.));
#31511=CARTESIAN_POINT('Ctrl Pts',(39.3231883392913,-3.27923485388117,18.));
#31512=CARTESIAN_POINT('Ctrl Pts',(39.4180596080755,-3.25707264313388,0.));
#31513=CARTESIAN_POINT('Ctrl Pts',(39.4180596080755,-3.25707264313388,18.));
#31514=CARTESIAN_POINT('Ctrl Pts',(39.5128908052622,-3.23406609691661,0.));
#31515=CARTESIAN_POINT('Ctrl Pts',(39.5128908052622,-3.23406609691661,18.));
#31516=CARTESIAN_POINT('Ctrl Pts',(39.607679107639,-3.21024640045595,0.));
#31517=CARTESIAN_POINT('Ctrl Pts',(39.607679107639,-3.21024640045595,18.));
#31518=CARTESIAN_POINT('Ctrl Pts',(39.7024216585552,-3.18565465503835,0.));
#31519=CARTESIAN_POINT('Ctrl Pts',(39.7024216585552,-3.18565465503835,18.));
#31520=CARTESIAN_POINT('Ctrl Pts',(39.7971156880138,-3.16033160752804,0.));
#31521=CARTESIAN_POINT('Ctrl Pts',(39.7971156880138,-3.16033160752804,18.));
#31522=CARTESIAN_POINT('Ctrl Pts',(39.8917586491576,-3.13430604330356,0.));
#31523=CARTESIAN_POINT('Ctrl Pts',(39.8917586491576,-3.13430604330356,18.));
#31524=CARTESIAN_POINT('Ctrl Pts',(39.9863482523153,-3.10759149802908,0.));
#31525=CARTESIAN_POINT('Ctrl Pts',(39.9863482523153,-3.10759149802908,18.));
#31526=CARTESIAN_POINT('Ctrl Pts',(40.0808823811787,-3.08019251155015,0.));
#31527=CARTESIAN_POINT('Ctrl Pts',(40.0808823811787,-3.08019251155015,18.));
#31528=CARTESIAN_POINT('Ctrl Pts',(40.1753590391515,-3.05210847423071,0.));
#31529=CARTESIAN_POINT('Ctrl Pts',(40.1753590391515,-3.05210847423071,18.));
#31530=CARTESIAN_POINT('Ctrl Pts',(40.2697762886113,-3.02333808901595,0.));
#31531=CARTESIAN_POINT('Ctrl Pts',(40.2697762886113,-3.02333808901595,18.));
#31532=CARTESIAN_POINT('Ctrl Pts',(40.3641321823444,-2.9938844645822,0.));
#31533=CARTESIAN_POINT('Ctrl Pts',(40.3641321823444,-2.9938844645822,18.));
#31534=CARTESIAN_POINT('Ctrl Pts',(40.4584247445196,-2.96375636417323,0.));
#31535=CARTESIAN_POINT('Ctrl Pts',(40.4584247445196,-2.96375636417323,18.));
#31536=CARTESIAN_POINT('Ctrl Pts',(40.5526520010651,-2.93296560822894,0.));
#31537=CARTESIAN_POINT('Ctrl Pts',(40.5526520010651,-2.93296560822894,18.));
#31538=CARTESIAN_POINT('Ctrl Pts',(40.6468119976928,-2.90152548734343,0.));
#31539=CARTESIAN_POINT('Ctrl Pts',(40.6468119976928,-2.90152548734343,18.));
#31540=CARTESIAN_POINT('Ctrl Pts',(40.7409028213129,-2.86944892209898,0.));
#31541=CARTESIAN_POINT('Ctrl Pts',(40.7409028213129,-2.86944892209898,18.));
#31542=CARTESIAN_POINT('Ctrl Pts',(40.8349226258683,-2.83674635946679,0.));
#31543=CARTESIAN_POINT('Ctrl Pts',(40.8349226258683,-2.83674635946679,18.));
#31544=CARTESIAN_POINT('Ctrl Pts',(40.9288696352159,-2.80342531768405,0.));
#31545=CARTESIAN_POINT('Ctrl Pts',(40.9288696352159,-2.80342531768405,18.));
#31546=CARTESIAN_POINT('Ctrl Pts',(41.0227421242398,-2.76949151194863,0.));
#31547=CARTESIAN_POINT('Ctrl Pts',(41.0227421242398,-2.76949151194863,18.));
#31548=CARTESIAN_POINT('Ctrl Pts',(41.1165384061145,-2.73494956725006,0.));
#31549=CARTESIAN_POINT('Ctrl Pts',(41.1165384061145,-2.73494956725006,18.));
#31550=CARTESIAN_POINT('Ctrl Pts',(41.2102568187956,-2.69980383625016,0.));
#31551=CARTESIAN_POINT('Ctrl Pts',(41.2102568187956,-2.69980383625016,18.));
#31552=CARTESIAN_POINT('Ctrl Pts',(41.3038957096306,-2.66405934050118,0.));
#31553=CARTESIAN_POINT('Ctrl Pts',(41.3038957096306,-2.66405934050118,18.));
#31554=CARTESIAN_POINT('Ctrl Pts',(41.3974534325936,-2.62772200460656,0.));
#31555=CARTESIAN_POINT('Ctrl Pts',(41.3974534325936,-2.62772200460656,18.));
#31556=CARTESIAN_POINT('Ctrl Pts',(41.4909283577703,-2.59079818040172,0.));
#31557=CARTESIAN_POINT('Ctrl Pts',(41.4909283577703,-2.59079818040172,18.));
#31558=CARTESIAN_POINT('Ctrl Pts',(41.5843188786284,-2.55329436064184,0.));
#31559=CARTESIAN_POINT('Ctrl Pts',(41.5843188786284,-2.55329436064184,18.));
#31560=CARTESIAN_POINT('Ctrl Pts',(41.6776234194583,-2.51521684674477,0.));
#31561=CARTESIAN_POINT('Ctrl Pts',(41.6776234194583,-2.51521684674477,18.));
#31562=CARTESIAN_POINT('Ctrl Pts',(41.7708404467532,-2.47657137427693,0.));
#31563=CARTESIAN_POINT('Ctrl Pts',(41.7708404467532,-2.47657137427693,18.));
#31564=CARTESIAN_POINT('Ctrl Pts',(41.8639684667923,-2.43736301434201,0.));
#31565=CARTESIAN_POINT('Ctrl Pts',(41.8639684667923,-2.43736301434201,18.));
#31566=CARTESIAN_POINT('Ctrl Pts',(41.9570060084039,-2.39759639399648,0.));
#31567=CARTESIAN_POINT('Ctrl Pts',(41.9570060084039,-2.39759639399648,18.));
#31568=CARTESIAN_POINT('Ctrl Pts',(42.0499516093661,-2.35727584066429,0.));
#31569=CARTESIAN_POINT('Ctrl Pts',(42.0499516093661,-2.35727584066429,18.));
#31570=CARTESIAN_POINT('Ctrl Pts',(42.1428038039937,-2.31640554742809,0.));
#31571=CARTESIAN_POINT('Ctrl Pts',(42.1428038039937,-2.31640554742809,18.));
#31572=CARTESIAN_POINT('Ctrl Pts',(42.2355611060784,-2.27498976664775,0.));
#31573=CARTESIAN_POINT('Ctrl Pts',(42.2355611060784,-2.27498976664775,18.));
#31574=CARTESIAN_POINT('Ctrl Pts',(42.3282220118033,-2.233032874655,0.));
#31575=CARTESIAN_POINT('Ctrl Pts',(42.3282220118033,-2.233032874655,18.));
#31576=CARTESIAN_POINT('Ctrl Pts',(42.4207850290047,-2.19053924976738,0.));
#31577=CARTESIAN_POINT('Ctrl Pts',(42.4207850290047,-2.19053924976738,18.));
#31578=CARTESIAN_POINT('Ctrl Pts',(42.5132487024335,-2.14751319676745,0.));
#31579=CARTESIAN_POINT('Ctrl Pts',(42.5132487024335,-2.14751319676745,18.));
#31580=CARTESIAN_POINT('Ctrl Pts',(42.6056116373455,-2.10395886401771,0.));
#31581=CARTESIAN_POINT('Ctrl Pts',(42.6056116373455,-2.10395886401771,18.));
#31582=CARTESIAN_POINT('Ctrl Pts',(42.6978725343209,-2.05988014924519,0.));
#31583=CARTESIAN_POINT('Ctrl Pts',(42.6978725343209,-2.05988014924519,18.));
#31584=CARTESIAN_POINT('Ctrl Pts',(42.7900301875309,-2.0152806752809,0.));
#31585=CARTESIAN_POINT('Ctrl Pts',(42.7900301875309,-2.0152806752809,18.));
#31586=CARTESIAN_POINT('Ctrl Pts',(42.8820834139973,-1.97016390194216,0.));
#31587=CARTESIAN_POINT('Ctrl Pts',(42.8820834139973,-1.97016390194216,18.));
#31588=CARTESIAN_POINT('Ctrl Pts',(42.9740309956624,-1.92453321512436,0.));
#31589=CARTESIAN_POINT('Ctrl Pts',(42.9740309956624,-1.92453321512436,18.));
#31590=CARTESIAN_POINT('Ctrl Pts',(43.065871623255,-1.87839202014609,0.));
#31591=CARTESIAN_POINT('Ctrl Pts',(43.065871623255,-1.87839202014609,18.));
#31592=CARTESIAN_POINT('Ctrl Pts',(43.1576038253643,-1.83174385734712,0.));
#31593=CARTESIAN_POINT('Ctrl Pts',(43.1576038253643,-1.83174385734712,18.));
#31594=CARTESIAN_POINT('Ctrl Pts',(43.2492259505872,-1.7845924484277,0.));
#31595=CARTESIAN_POINT('Ctrl Pts',(43.2492259505872,-1.7845924484277,18.));
#31596=CARTESIAN_POINT('Ctrl Pts',(43.3407363140236,-1.73694151741124,0.));
#31597=CARTESIAN_POINT('Ctrl Pts',(43.3407363140236,-1.73694151741124,18.));
#31598=CARTESIAN_POINT('Ctrl Pts',(43.4321333178711,-1.68879465270608,0.));
#31599=CARTESIAN_POINT('Ctrl Pts',(43.4321333178711,-1.68879465270608,18.));
#31600=CARTESIAN_POINT('Ctrl Pts',(43.5234155788248,-1.64015515906648,0.));
#31601=CARTESIAN_POINT('Ctrl Pts',(43.5234155788248,-1.64015515906648,18.));
#31602=CARTESIAN_POINT('Ctrl Pts',(43.6145820637333,-1.59102591108104,0.));
#31603=CARTESIAN_POINT('Ctrl Pts',(43.6145820637333,-1.59102591108104,18.));
#31604=CARTESIAN_POINT('Ctrl Pts',(43.7056321934163,-1.54140922714765,0.));
#31605=CARTESIAN_POINT('Ctrl Pts',(43.7056321934163,-1.54140922714765,18.));
#31606=CARTESIAN_POINT('Ctrl Pts',(43.7965657112707,-1.49130689006067,0.));
#31607=CARTESIAN_POINT('Ctrl Pts',(43.7965657112707,-1.49130689006067,18.));
#31608=CARTESIAN_POINT('Ctrl Pts',(43.8692192047561,-1.45083750111682,0.));
#31609=CARTESIAN_POINT('Ctrl Pts',(43.8692192047561,-1.45083750111682,18.));
#31610=CARTESIAN_POINT('Ctrl Pts',(43.9236568607623,-1.42026781296156,0.));
#31611=CARTESIAN_POINT('Ctrl Pts',(43.9236568607623,-1.42026781296156,18.));
#31612=CARTESIAN_POINT('Ctrl Pts',(43.9599253218251,-1.39979132121931,0.));
#31613=CARTESIAN_POINT('Ctrl Pts',(43.9599253218251,-1.39979132121931,18.));
#31614=CARTESIAN_POINT('Ctrl Pts',(43.9780537249529,-1.38952890043916,0.));
#31615=CARTESIAN_POINT('Ctrl Pts',(43.9780537249529,-1.38952890043916,18.));
#31616=CARTESIAN_POINT('Origin',(0.,0.,0.));
#31617=CARTESIAN_POINT('',(0.,0.,0.));
#31618=CARTESIAN_POINT('Origin',(3.70814490224802E-12,-1.04805053524615E-12,
7.49999782838924));
#31619=CARTESIAN_POINT('',(-7.49999999999629,-1.12798659301916E-12,14.9999978283892));
#31620=CARTESIAN_POINT('Origin',(3.70814490224802E-12,-1.12798659301916E-12,
14.9999978283892));
#31621=CARTESIAN_POINT('',(-7.4999999999963,-1.09223486052218E-12,57.4999978283893));
#31622=CARTESIAN_POINT('',(-7.4999999999963,-1.04713205014679E-12,7.49999782838924));
#31623=CARTESIAN_POINT('Origin',(3.70814490224802E-12,-1.09315334562154E-12,
57.4999978283893));
#31624=CARTESIAN_POINT('Origin',(3.70814490224802E-12,-1.04805053524615E-12,
7.49999782838924));
#31625=CARTESIAN_POINT('',(-7.4999999999963,-1.00112718356388E-12,-43.5000021716108));
#31626=CARTESIAN_POINT('Origin',(3.70814490224802E-12,-1.00204566866324E-12,
-43.5000021716108));
#31627=CARTESIAN_POINT('',(-7.49999999999629,-1.11022302462516E-12,-2.17161075816152E-6));
#31628=CARTESIAN_POINT('',(-7.4999999999963,-1.04713205014679E-12,7.49999782838924));
#31629=CARTESIAN_POINT('Origin',(3.70814490224802E-12,-1.11022302462516E-12,
-2.17161075816152E-6));
#31630=CARTESIAN_POINT('Origin',(3.70814490224802E-12,-1.09232067835308E-12,
57.4999978283893));
#31631=CARTESIAN_POINT('Origin',(3.70814490224802E-12,-1.00290609150733E-12,
-43.5000021716108));
#31632=CARTESIAN_POINT('Origin',(15.1099349338646,-6.30335230606528,0.));
#31633=CARTESIAN_POINT('',(14.1870217324314,-5.91834422482504,15.));
#31634=CARTESIAN_POINT('',(14.6692742696684,-7.20102606586345,15.));
#31635=CARTESIAN_POINT('Origin',(15.1099349338646,-6.30335230606528,15.));
#31636=CARTESIAN_POINT('',(14.6692742696684,-7.20102606586345,0.));
#31637=CARTESIAN_POINT('',(14.6692742696684,-7.20102606586345,0.));
#31638=CARTESIAN_POINT('',(14.1870217324314,-5.91834422482504,0.));
#31639=CARTESIAN_POINT('Origin',(15.1099349338646,-6.30335230606528,0.));
#31640=CARTESIAN_POINT('',(14.1870217324314,-5.91834422482504,0.));
#31641=CARTESIAN_POINT('Origin',(16.8707481591095,-8.28171148831561,0.));
#31642=CARTESIAN_POINT('',(16.8707481591095,-8.28171148831561,15.));
#31643=CARTESIAN_POINT('',(13.7900642980194,-6.76942912338193,15.));
#31644=CARTESIAN_POINT('',(16.8707481591095,-8.28171148831561,0.));
#31645=CARTESIAN_POINT('',(16.8707481591095,-8.28171148831561,0.));
#31646=CARTESIAN_POINT('',(13.7900642980194,-6.76942912338193,0.));
#31647=CARTESIAN_POINT('Origin',(10.6640709636513,-12.422559095541,0.));
#31648=CARTESIAN_POINT('',(10.0127106555856,-11.6637905214181,0.));
#31649=CARTESIAN_POINT('',(11.3816378084254,-11.7260694522002,0.));
#31650=CARTESIAN_POINT('Origin',(10.6640709636513,-12.422559095541,0.));
#31651=CARTESIAN_POINT('',(11.3816378084254,-11.7260694522002,15.));
#31652=CARTESIAN_POINT('',(11.3816378084254,-11.7260694522002,0.));
#31653=CARTESIAN_POINT('',(10.0127106555856,-11.6637905214181,15.));
#31654=CARTESIAN_POINT('Origin',(10.6640709636513,-12.422559095541,15.));
#31655=CARTESIAN_POINT('',(10.0127106555856,-11.6637905214181,0.));
#31656=CARTESIAN_POINT('Origin',(10.6994739010018,-11.0232618694188,0.));
#31657=CARTESIAN_POINT('',(13.0897235660237,-13.4858453790958,0.));
#31658=CARTESIAN_POINT('',(10.6994739010018,-11.0232618694188,0.));
#31659=CARTESIAN_POINT('',(13.0897235660237,-13.4858453790958,15.));
#31660=CARTESIAN_POINT('',(13.0897235660237,-13.4858453790958,0.));
#31661=CARTESIAN_POINT('',(10.6994739010018,-11.0232618694188,15.));
#31662=CARTESIAN_POINT('Origin',(8.51917661988723,-13.9809160543638,0.));
#31663=CARTESIAN_POINT('',(7.9988262277612,-13.1269632047203,15.));
#31664=CARTESIAN_POINT('',(7.63503525642066,-14.448135541765,15.));
#31665=CARTESIAN_POINT('Origin',(8.51917661988723,-13.9809160543638,15.));
#31666=CARTESIAN_POINT('',(7.63503525642066,-14.448135541765,0.));
#31667=CARTESIAN_POINT('',(7.63503525642066,-14.448135541765,0.));
#31668=CARTESIAN_POINT('',(7.9988262277612,-13.1269632047203,0.));
#31669=CARTESIAN_POINT('Origin',(8.51917661988723,-13.9809160543638,0.));
#31670=CARTESIAN_POINT('',(7.9988262277612,-13.1269632047203,0.));
#31671=CARTESIAN_POINT('Origin',(8.78085409196639,-16.6164222996225,0.));
#31672=CARTESIAN_POINT('',(8.78085409196639,-16.6164222996225,15.));
#31673=CARTESIAN_POINT('',(7.17742576545784,-13.5821796255734,15.));
#31674=CARTESIAN_POINT('',(8.78085409196639,-16.6164222996225,0.));
#31675=CARTESIAN_POINT('',(8.78085409196639,-16.6164222996225,0.));
#31676=CARTESIAN_POINT('',(7.17742576545784,-13.5821796255734,0.));
#31677=CARTESIAN_POINT('Origin',(1.32561760672361,-16.3182450637544,0.));
#31678=CARTESIAN_POINT('',(1.24464902580963,-15.3215284094816,0.));
#31679=CARTESIAN_POINT('',(2.315527719476,-16.1765483147777,0.));
#31680=CARTESIAN_POINT('Origin',(1.32561760672361,-16.3182450637544,0.));
#31681=CARTESIAN_POINT('',(2.315527719476,-16.1765483147777,15.));
#31682=CARTESIAN_POINT('',(2.315527719476,-16.1765483147777,0.));
#31683=CARTESIAN_POINT('',(1.24464902580963,-15.3215284094816,15.));
#31684=CARTESIAN_POINT('Origin',(1.32561760672361,-16.3182450637544,15.));
#31685=CARTESIAN_POINT('',(1.24464902580963,-15.3215284094816,0.));
#31686=CARTESIAN_POINT('Origin',(2.17674545777935,-15.2069991521022,0.));
#31687=CARTESIAN_POINT('',(2.66302778805429,-18.6042245638953,0.));
#31688=CARTESIAN_POINT('',(2.17674545777935,-15.2069991521022,0.));
#31689=CARTESIAN_POINT('',(2.66302778805429,-18.6042245638953,15.));
#31690=CARTESIAN_POINT('',(2.66302778805429,-18.6042245638953,0.));
#31691=CARTESIAN_POINT('',(2.17674545777935,-15.2069991521022,15.));
#31692=CARTESIAN_POINT('Origin',(-1.32561760672361,-16.3182450637544,0.));
#31693=CARTESIAN_POINT('',(-1.24464902580964,-15.3215284094816,15.));
#31694=CARTESIAN_POINT('',(-2.315527719476,-16.1765483147777,15.));
#31695=CARTESIAN_POINT('Origin',(-1.32561760672361,-16.3182450637544,15.));
#31696=CARTESIAN_POINT('',(-2.315527719476,-16.1765483147777,0.));
#31697=CARTESIAN_POINT('',(-2.315527719476,-16.1765483147777,0.));
#31698=CARTESIAN_POINT('',(-1.24464902580964,-15.3215284094816,0.));
#31699=CARTESIAN_POINT('Origin',(-1.32561760672361,-16.3182450637544,0.));
#31700=CARTESIAN_POINT('',(-1.24464902580964,-15.3215284094816,0.));
#31701=CARTESIAN_POINT('Origin',(-2.6630277880543,-18.6042245638953,0.));
#31702=CARTESIAN_POINT('',(-2.6630277880543,-18.6042245638953,15.));
#31703=CARTESIAN_POINT('',(-2.17674545777936,-15.2069991521022,15.));
#31704=CARTESIAN_POINT('',(-2.6630277880543,-18.6042245638953,0.));
#31705=CARTESIAN_POINT('',(-2.6630277880543,-18.6042245638953,0.));
#31706=CARTESIAN_POINT('',(-2.17674545777936,-15.2069991521022,0.));
#31707=CARTESIAN_POINT('Origin',(-8.51917661988722,-13.9809160543638,0.));
#31708=CARTESIAN_POINT('',(-7.9988262277612,-13.1269632047203,0.));
#31709=CARTESIAN_POINT('',(-7.63503525642066,-14.448135541765,0.));
#31710=CARTESIAN_POINT('Origin',(-8.51917661988722,-13.9809160543638,0.));
#31711=CARTESIAN_POINT('',(-7.63503525642066,-14.448135541765,15.));
#31712=CARTESIAN_POINT('',(-7.63503525642066,-14.448135541765,0.));
#31713=CARTESIAN_POINT('',(-7.9988262277612,-13.1269632047203,15.));
#31714=CARTESIAN_POINT('Origin',(-8.51917661988722,-13.9809160543638,15.));
#31715=CARTESIAN_POINT('',(-7.9988262277612,-13.1269632047203,0.));
#31716=CARTESIAN_POINT('Origin',(-7.17742576545785,-13.5821796255734,0.));
#31717=CARTESIAN_POINT('',(-8.7808540919664,-16.6164222996225,0.));
#31718=CARTESIAN_POINT('',(-7.17742576545785,-13.5821796255734,0.));
#31719=CARTESIAN_POINT('',(-8.7808540919664,-16.6164222996225,15.));
#31720=CARTESIAN_POINT('',(-8.7808540919664,-16.6164222996225,0.));
#31721=CARTESIAN_POINT('',(-7.17742576545785,-13.5821796255734,15.));
#31722=CARTESIAN_POINT('Origin',(-10.6640709636513,-12.422559095541,0.));
#31723=CARTESIAN_POINT('',(-10.0127106555856,-11.6637905214181,15.));
#31724=CARTESIAN_POINT('',(-11.3816378084254,-11.7260694522002,15.));
#31725=CARTESIAN_POINT('Origin',(-10.6640709636513,-12.422559095541,15.));
#31726=CARTESIAN_POINT('',(-11.3816378084254,-11.7260694522002,0.));
#31727=CARTESIAN_POINT('',(-11.3816378084254,-11.7260694522002,0.));
#31728=CARTESIAN_POINT('',(-10.0127106555856,-11.6637905214181,0.));
#31729=CARTESIAN_POINT('Origin',(-10.6640709636513,-12.422559095541,0.));
#31730=CARTESIAN_POINT('',(-10.0127106555856,-11.6637905214181,0.));
#31731=CARTESIAN_POINT('Origin',(-13.0897235660237,-13.4858453790958,0.));
#31732=CARTESIAN_POINT('',(-13.0897235660237,-13.4858453790958,15.));
#31733=CARTESIAN_POINT('',(-10.6994739010018,-11.0232618694188,15.));
#31734=CARTESIAN_POINT('',(-13.0897235660237,-13.4858453790958,0.));
#31735=CARTESIAN_POINT('',(-13.0897235660237,-13.4858453790958,0.));
#31736=CARTESIAN_POINT('',(-10.6994739010018,-11.0232618694188,0.));
#31737=CARTESIAN_POINT('Origin',(-15.1099349338646,-6.30335230606528,0.));
#31738=CARTESIAN_POINT('',(-14.1870217324314,-5.91834422482503,0.));
#31739=CARTESIAN_POINT('',(-14.6692742696684,-7.20102606586344,0.));
#31740=CARTESIAN_POINT('Origin',(-15.1099349338646,-6.30335230606528,0.));
#31741=CARTESIAN_POINT('',(-14.6692742696684,-7.20102606586344,15.));
#31742=CARTESIAN_POINT('',(-14.6692742696684,-7.20102606586344,0.));
#31743=CARTESIAN_POINT('',(-14.1870217324314,-5.91834422482503,15.));
#31744=CARTESIAN_POINT('Origin',(-15.1099349338646,-6.30335230606528,15.));
#31745=CARTESIAN_POINT('',(-14.1870217324314,-5.91834422482503,0.));
#31746=CARTESIAN_POINT('Origin',(-13.7900642980194,-6.76942912338193,0.));
#31747=CARTESIAN_POINT('',(-16.8707481591095,-8.28171148831561,0.));
#31748=CARTESIAN_POINT('',(-13.7900642980194,-6.76942912338193,0.));
#31749=CARTESIAN_POINT('',(-16.8707481591095,-8.28171148831561,15.));
#31750=CARTESIAN_POINT('',(-16.8707481591095,-8.28171148831561,0.));
#31751=CARTESIAN_POINT('',(-13.7900642980194,-6.76942912338193,15.));
#31752=CARTESIAN_POINT('Origin',(-15.9292116709051,-3.78187778008512,0.));
#31753=CARTESIAN_POINT('',(-14.9562571344462,-3.5508810918317,15.));
#31754=CARTESIAN_POINT('',(-16.1003491021971,-2.79663061332402,15.));
#31755=CARTESIAN_POINT('Origin',(-15.9292116709051,-3.78187778008512,15.));
#31756=CARTESIAN_POINT('',(-16.1003491021971,-2.79663061332402,0.));
#31757=CARTESIAN_POINT('',(-16.1003491021971,-2.79663061332403,0.));
#31758=CARTESIAN_POINT('',(-14.9562571344462,-3.5508810918317,0.));
#31759=CARTESIAN_POINT('Origin',(-15.9292116709051,-3.78187778008512,0.));
#31760=CARTESIAN_POINT('',(-14.9562571344462,-3.5508810918317,0.));
#31761=CARTESIAN_POINT('Origin',(-18.5165898451125,-3.21633162650739,0.));
#31762=CARTESIAN_POINT('',(-18.5165898451125,-3.21633162650739,15.));
#31763=CARTESIAN_POINT('',(-15.135366975784,-2.62901321950806,15.));
#31764=CARTESIAN_POINT('',(-18.5165898451125,-3.21633162650739,0.));
#31765=CARTESIAN_POINT('',(-18.5165898451125,-3.21633162650739,0.));
#31766=CARTESIAN_POINT('',(-15.135366975784,-2.62901321950806,0.));
#31767=CARTESIAN_POINT('Origin',(-15.9292116709051,3.78187778008512,0.));
#31768=CARTESIAN_POINT('',(-14.9562571344462,3.5508810918317,0.));
#31769=CARTESIAN_POINT('',(-16.1003491021971,2.79663061332403,0.));
#31770=CARTESIAN_POINT('Origin',(-15.9292116709051,3.78187778008512,0.));
#31771=CARTESIAN_POINT('',(-16.1003491021971,2.79663061332403,15.));
#31772=CARTESIAN_POINT('',(-16.1003491021971,2.79663061332403,0.));
#31773=CARTESIAN_POINT('',(-14.9562571344462,3.5508810918317,15.));
#31774=CARTESIAN_POINT('Origin',(-15.9292116709051,3.78187778008512,15.));
#31775=CARTESIAN_POINT('',(-14.9562571344462,3.5508810918317,0.));
#31776=CARTESIAN_POINT('Origin',(-15.135366975784,2.62901321950807,0.));
#31777=CARTESIAN_POINT('',(-18.5165898451125,3.2163316265074,0.));
#31778=CARTESIAN_POINT('',(-15.135366975784,2.62901321950807,0.));
#31779=CARTESIAN_POINT('',(-18.5165898451125,3.2163316265074,15.));
#31780=CARTESIAN_POINT('',(-18.5165898451125,3.2163316265074,0.));
#31781=CARTESIAN_POINT('',(-15.135366975784,2.62901321950807,15.));
#31782=CARTESIAN_POINT('Origin',(-15.1099349338646,6.30335230606528,0.));
#31783=CARTESIAN_POINT('',(-14.1870217324314,5.91834422482504,15.));
#31784=CARTESIAN_POINT('',(-14.6692742696684,7.20102606586345,15.));
#31785=CARTESIAN_POINT('Origin',(-15.1099349338646,6.30335230606528,15.));
#31786=CARTESIAN_POINT('',(-14.6692742696684,7.20102606586345,0.));
#31787=CARTESIAN_POINT('',(-14.6692742696684,7.20102606586345,0.));
#31788=CARTESIAN_POINT('',(-14.1870217324314,5.91834422482504,0.));
#31789=CARTESIAN_POINT('Origin',(-15.1099349338646,6.30335230606528,0.));
#31790=CARTESIAN_POINT('',(-14.1870217324314,5.91834422482504,0.));
#31791=CARTESIAN_POINT('Origin',(-16.8707481591095,8.28171148831561,0.));
#31792=CARTESIAN_POINT('',(-16.8707481591095,8.28171148831561,15.));
#31793=CARTESIAN_POINT('',(-13.7900642980194,6.76942912338193,15.));
#31794=CARTESIAN_POINT('',(-16.8707481591095,8.28171148831561,0.));
#31795=CARTESIAN_POINT('',(-16.8707481591095,8.28171148831561,0.));
#31796=CARTESIAN_POINT('',(-13.7900642980194,6.76942912338193,0.));
#31797=CARTESIAN_POINT('Origin',(-10.6640709636513,12.422559095541,0.));
#31798=CARTESIAN_POINT('',(-10.0127106555856,11.6637905214181,0.));
#31799=CARTESIAN_POINT('',(-11.3816378084254,11.7260694522002,0.));
#31800=CARTESIAN_POINT('Origin',(-10.6640709636513,12.422559095541,0.));
#31801=CARTESIAN_POINT('',(-11.3816378084254,11.7260694522002,15.));
#31802=CARTESIAN_POINT('',(-11.3816378084254,11.7260694522002,0.));
#31803=CARTESIAN_POINT('',(-10.0127106555856,11.6637905214181,15.));
#31804=CARTESIAN_POINT('Origin',(-10.6640709636513,12.422559095541,15.));
#31805=CARTESIAN_POINT('',(-10.0127106555856,11.6637905214181,0.));
#31806=CARTESIAN_POINT('Origin',(-10.6994739010018,11.0232618694188,0.));
#31807=CARTESIAN_POINT('',(-13.0897235660237,13.4858453790958,0.));
#31808=CARTESIAN_POINT('',(-10.6994739010018,11.0232618694188,0.));
#31809=CARTESIAN_POINT('',(-13.0897235660237,13.4858453790958,15.));
#31810=CARTESIAN_POINT('',(-13.0897235660237,13.4858453790958,0.));
#31811=CARTESIAN_POINT('',(-10.6994739010018,11.0232618694188,15.));
#31812=CARTESIAN_POINT('Origin',(-8.51917661988722,13.9809160543638,0.));
#31813=CARTESIAN_POINT('',(-7.9988262277612,13.1269632047203,15.));
#31814=CARTESIAN_POINT('',(-7.63503525642066,14.448135541765,15.));
#31815=CARTESIAN_POINT('Origin',(-8.51917661988722,13.9809160543638,15.));
#31816=CARTESIAN_POINT('',(-7.63503525642066,14.448135541765,0.));
#31817=CARTESIAN_POINT('',(-7.63503525642066,14.448135541765,0.));
#31818=CARTESIAN_POINT('',(-7.9988262277612,13.1269632047203,0.));
#31819=CARTESIAN_POINT('Origin',(-8.51917661988722,13.9809160543638,0.));
#31820=CARTESIAN_POINT('',(-7.9988262277612,13.1269632047203,0.));
#31821=CARTESIAN_POINT('Origin',(-8.78085409196639,16.6164222996225,0.));
#31822=CARTESIAN_POINT('',(-8.78085409196639,16.6164222996225,15.));
#31823=CARTESIAN_POINT('',(-7.17742576545784,13.5821796255734,15.));
#31824=CARTESIAN_POINT('',(-8.78085409196639,16.6164222996225,0.));
#31825=CARTESIAN_POINT('',(-8.78085409196639,16.6164222996225,0.));
#31826=CARTESIAN_POINT('',(-7.17742576545784,13.5821796255734,0.));
#31827=CARTESIAN_POINT('Origin',(-1.32561760672361,16.3182450637544,0.));
#31828=CARTESIAN_POINT('',(-1.24464902580963,15.3215284094816,0.));
#31829=CARTESIAN_POINT('',(-2.315527719476,16.1765483147777,0.));
#31830=CARTESIAN_POINT('Origin',(-1.32561760672361,16.3182450637544,0.));
#31831=CARTESIAN_POINT('',(-2.315527719476,16.1765483147777,15.));
#31832=CARTESIAN_POINT('',(-2.315527719476,16.1765483147777,0.));
#31833=CARTESIAN_POINT('',(-1.24464902580963,15.3215284094816,15.));
#31834=CARTESIAN_POINT('Origin',(-1.32561760672361,16.3182450637544,15.));
#31835=CARTESIAN_POINT('',(-1.24464902580963,15.3215284094816,0.));
#31836=CARTESIAN_POINT('Origin',(-2.17674545777935,15.2069991521022,0.));
#31837=CARTESIAN_POINT('',(-2.66302778805429,18.6042245638953,0.));
#31838=CARTESIAN_POINT('',(-2.17674545777935,15.2069991521022,0.));
#31839=CARTESIAN_POINT('',(-2.66302778805429,18.6042245638953,15.));
#31840=CARTESIAN_POINT('',(-2.66302778805429,18.6042245638953,0.));
#31841=CARTESIAN_POINT('',(-2.17674545777935,15.2069991521022,15.));
#31842=CARTESIAN_POINT('Origin',(1.32561760672361,16.3182450637544,0.));
#31843=CARTESIAN_POINT('',(1.24464902580964,15.3215284094816,15.));
#31844=CARTESIAN_POINT('',(2.315527719476,16.1765483147777,15.));
#31845=CARTESIAN_POINT('Origin',(1.32561760672361,16.3182450637544,15.));
#31846=CARTESIAN_POINT('',(2.315527719476,16.1765483147777,0.));
#31847=CARTESIAN_POINT('',(2.315527719476,16.1765483147777,0.));
#31848=CARTESIAN_POINT('',(1.24464902580964,15.3215284094816,0.));
#31849=CARTESIAN_POINT('Origin',(1.32561760672361,16.3182450637544,0.));
#31850=CARTESIAN_POINT('',(1.24464902580964,15.3215284094816,0.));
#31851=CARTESIAN_POINT('Origin',(2.66302778805429,18.6042245638953,0.));
#31852=CARTESIAN_POINT('',(2.66302778805429,18.6042245638953,15.));
#31853=CARTESIAN_POINT('',(2.17674545777935,15.2069991521022,15.));
#31854=CARTESIAN_POINT('',(2.66302778805429,18.6042245638953,0.));
#31855=CARTESIAN_POINT('',(2.66302778805429,18.6042245638953,0.));
#31856=CARTESIAN_POINT('',(2.17674545777935,15.2069991521022,0.));
#31857=CARTESIAN_POINT('Origin',(8.51917661988723,13.9809160543638,0.));
#31858=CARTESIAN_POINT('',(7.9988262277612,13.1269632047203,0.));
#31859=CARTESIAN_POINT('',(7.63503525642066,14.448135541765,0.));
#31860=CARTESIAN_POINT('Origin',(8.51917661988723,13.9809160543638,0.));
#31861=CARTESIAN_POINT('',(7.63503525642066,14.448135541765,15.));
#31862=CARTESIAN_POINT('',(7.63503525642066,14.448135541765,0.));
#31863=CARTESIAN_POINT('',(7.9988262277612,13.1269632047203,15.));
#31864=CARTESIAN_POINT('Origin',(8.51917661988723,13.9809160543638,15.));
#31865=CARTESIAN_POINT('',(7.9988262277612,13.1269632047203,0.));
#31866=CARTESIAN_POINT('Origin',(7.17742576545784,13.5821796255734,0.));
#31867=CARTESIAN_POINT('',(8.78085409196639,16.6164222996225,0.));
#31868=CARTESIAN_POINT('',(7.17742576545784,13.5821796255734,0.));
#31869=CARTESIAN_POINT('',(8.78085409196639,16.6164222996225,15.));
#31870=CARTESIAN_POINT('',(8.78085409196639,16.6164222996225,0.));
#31871=CARTESIAN_POINT('',(7.17742576545784,13.5821796255734,15.));
#31872=CARTESIAN_POINT('Origin',(10.6640709636513,12.422559095541,0.));
#31873=CARTESIAN_POINT('',(10.0127106555856,11.6637905214181,15.));
#31874=CARTESIAN_POINT('',(11.3816378084254,11.7260694522002,15.));
#31875=CARTESIAN_POINT('Origin',(10.6640709636513,12.422559095541,15.));
#31876=CARTESIAN_POINT('',(11.3816378084254,11.7260694522002,0.));
#31877=CARTESIAN_POINT('',(11.3816378084254,11.7260694522002,0.));
#31878=CARTESIAN_POINT('',(10.0127106555856,11.6637905214181,0.));
#31879=CARTESIAN_POINT('Origin',(10.6640709636513,12.422559095541,0.));
#31880=CARTESIAN_POINT('',(10.0127106555856,11.6637905214181,0.));
#31881=CARTESIAN_POINT('Origin',(13.0897235660237,13.4858453790958,0.));
#31882=CARTESIAN_POINT('',(13.0897235660237,13.4858453790958,15.));
#31883=CARTESIAN_POINT('',(10.6994739010018,11.0232618694188,15.));
#31884=CARTESIAN_POINT('',(13.0897235660237,13.4858453790958,0.));
#31885=CARTESIAN_POINT('',(13.0897235660237,13.4858453790958,0.));
#31886=CARTESIAN_POINT('',(10.6994739010018,11.0232618694188,0.));
#31887=CARTESIAN_POINT('Origin',(15.1099349338646,6.30335230606528,0.));
#31888=CARTESIAN_POINT('',(14.1870217324314,5.91834422482504,0.));
#31889=CARTESIAN_POINT('',(14.6692742696684,7.20102606586344,0.));
#31890=CARTESIAN_POINT('Origin',(15.1099349338646,6.30335230606528,0.));
#31891=CARTESIAN_POINT('',(14.6692742696684,7.20102606586344,15.));
#31892=CARTESIAN_POINT('',(14.6692742696684,7.20102606586344,0.));
#31893=CARTESIAN_POINT('',(14.1870217324314,5.91834422482504,15.));
#31894=CARTESIAN_POINT('Origin',(15.1099349338646,6.30335230606528,15.));
#31895=CARTESIAN_POINT('',(14.1870217324314,5.91834422482504,0.));
#31896=CARTESIAN_POINT('Origin',(13.7900642980194,6.76942912338193,0.));
#31897=CARTESIAN_POINT('',(16.8707481591095,8.28171148831561,0.));
#31898=CARTESIAN_POINT('',(13.7900642980194,6.76942912338193,0.));
#31899=CARTESIAN_POINT('',(16.8707481591095,8.28171148831561,15.));
#31900=CARTESIAN_POINT('',(16.8707481591095,8.28171148831561,0.));
#31901=CARTESIAN_POINT('',(13.7900642980194,6.76942912338193,15.));
#31902=CARTESIAN_POINT('Ctrl Pts',(20.0837475345526,-13.1393715591102,0.));
#31903=CARTESIAN_POINT('Ctrl Pts',(20.0837475345526,-13.1393715591102,18.));
#31904=CARTESIAN_POINT('Ctrl Pts',(20.0780177478283,-13.1220955868173,0.));
#31905=CARTESIAN_POINT('Ctrl Pts',(20.0780177478283,-13.1220955868173,18.));
#31906=CARTESIAN_POINT('Ctrl Pts',(20.0665110891946,-13.0875783330728,0.));
#31907=CARTESIAN_POINT('Ctrl Pts',(20.0665110891946,-13.0875783330728,18.));
#31908=CARTESIAN_POINT('Ctrl Pts',(20.0491098457044,-13.0359065249991,0.));
#31909=CARTESIAN_POINT('Ctrl Pts',(20.0491098457044,-13.0359065249991,18.));
#31910=CARTESIAN_POINT('Ctrl Pts',(20.0256255826397,-12.9672189949731,0.));
#31911=CARTESIAN_POINT('Ctrl Pts',(20.0256255826397,-12.9672189949731,18.));
#31912=CARTESIAN_POINT('Ctrl Pts',(19.9957986945787,-12.8817072534696,0.));
#31913=CARTESIAN_POINT('Ctrl Pts',(19.9957986945787,-12.8817072534696,18.));
#31914=CARTESIAN_POINT('Ctrl Pts',(19.9654995335894,-12.7965444294443,0.));
#31915=CARTESIAN_POINT('Ctrl Pts',(19.9654995335894,-12.7965444294443,18.));
#31916=CARTESIAN_POINT('Ctrl Pts',(19.9347273847264,-12.7117325003719,0.));
#31917=CARTESIAN_POINT('Ctrl Pts',(19.9347273847264,-12.7117325003719,18.));
#31918=CARTESIAN_POINT('Ctrl Pts',(19.9034816813503,-12.6272742843372,0.));
#31919=CARTESIAN_POINT('Ctrl Pts',(19.9034816813503,-12.6272742843372,18.));
#31920=CARTESIAN_POINT('Ctrl Pts',(19.8717621942733,-12.5431736030596,0.));
#31921=CARTESIAN_POINT('Ctrl Pts',(19.8717621942733,-12.5431736030596,18.));
#31922=CARTESIAN_POINT('Ctrl Pts',(19.839568972011,-12.4594350764989,0.));
#31923=CARTESIAN_POINT('Ctrl Pts',(19.839568972011,-12.4594350764989,18.));
#31924=CARTESIAN_POINT('Ctrl Pts',(19.8069022248387,-12.3760638341708,0.));
#31925=CARTESIAN_POINT('Ctrl Pts',(19.8069022248387,-12.3760638341708,18.));
#31926=CARTESIAN_POINT('Ctrl Pts',(19.7737622285562,-12.2930652417987,0.));
#31927=CARTESIAN_POINT('Ctrl Pts',(19.7737622285562,-12.2930652417987,18.));
#31928=CARTESIAN_POINT('Ctrl Pts',(19.7401492304335,-12.2104446447874,0.));
#31929=CARTESIAN_POINT('Ctrl Pts',(19.7401492304335,-12.2104446447874,18.));
#31930=CARTESIAN_POINT('Ctrl Pts',(19.7060633406705,-12.1282070378972,0.));
#31931=CARTESIAN_POINT('Ctrl Pts',(19.7060633406705,-12.1282070378972,18.));
#31932=CARTESIAN_POINT('Ctrl Pts',(19.6715045149944,-12.0463570680309,0.));
#31933=CARTESIAN_POINT('Ctrl Pts',(19.6715045149944,-12.0463570680309,18.));
#31934=CARTESIAN_POINT('Ctrl Pts',(19.6364725931695,-11.9648992312094,0.));
#31935=CARTESIAN_POINT('Ctrl Pts',(19.6364725931695,-11.9648992312094,18.));
#31936=CARTESIAN_POINT('Ctrl Pts',(19.6009673241771,-11.8838380136222,0.));
#31937=CARTESIAN_POINT('Ctrl Pts',(19.6009673241771,-11.8838380136222,18.));
#31938=CARTESIAN_POINT('Ctrl Pts',(19.5649883985826,-11.8031780389346,0.));
#31939=CARTESIAN_POINT('Ctrl Pts',(19.5649883985826,-11.8031780389346,18.));
#31940=CARTESIAN_POINT('Ctrl Pts',(19.5285354853626,-11.722924244195,0.));
#31941=CARTESIAN_POINT('Ctrl Pts',(19.5285354853626,-11.722924244195,18.));
#31942=CARTESIAN_POINT('Ctrl Pts',(19.4916082541529,-11.6430819099846,0.));
#31943=CARTESIAN_POINT('Ctrl Pts',(19.4916082541529,-11.6430819099846,18.));
#31944=CARTESIAN_POINT('Ctrl Pts',(19.4542063779876,-11.5636565297382,0.));
#31945=CARTESIAN_POINT('Ctrl Pts',(19.4542063779876,-11.5636565297382,18.));
#31946=CARTESIAN_POINT('Ctrl Pts',(19.4163295466324,-11.4846537135043,0.));
#31947=CARTESIAN_POINT('Ctrl Pts',(19.4163295466324,-11.4846537135043,18.));
#31948=CARTESIAN_POINT('Ctrl Pts',(19.3779774742875,-11.4060790880015,0.));
#31949=CARTESIAN_POINT('Ctrl Pts',(19.3779774742875,-11.4060790880015,18.));
#31950=CARTESIAN_POINT('Ctrl Pts',(19.3391499248083,-11.3279381634523,0.));
#31951=CARTESIAN_POINT('Ctrl Pts',(19.3391499248083,-11.3279381634523,18.));
#31952=CARTESIAN_POINT('Ctrl Pts',(19.2998466936739,-11.2502363198588,0.));
#31953=CARTESIAN_POINT('Ctrl Pts',(19.2998466936739,-11.2502363198588,18.));
#31954=CARTESIAN_POINT('Ctrl Pts',(19.2600675167206,-11.1729790050543,0.));
#31955=CARTESIAN_POINT('Ctrl Pts',(19.2600675167206,-11.1729790050543,18.));
#31956=CARTESIAN_POINT('Ctrl Pts',(19.2198119937835,-11.0961718903994,0.));
#31957=CARTESIAN_POINT('Ctrl Pts',(19.2198119937835,-11.0961718903994,18.));
#31958=CARTESIAN_POINT('Ctrl Pts',(19.1790795192393,-11.0198210228993,0.));
#31959=CARTESIAN_POINT('Ctrl Pts',(19.1790795192393,-11.0198210228993,18.));
#31960=CARTESIAN_POINT('Ctrl Pts',(19.1378691901023,-10.9439330179206,0.));
#31961=CARTESIAN_POINT('Ctrl Pts',(19.1378691901023,-10.9439330179206,18.));
#31962=CARTESIAN_POINT('Ctrl Pts',(19.0961797996403,-10.868515097783,0.));
#31963=CARTESIAN_POINT('Ctrl Pts',(19.0961797996403,-10.868515097783,18.));
#31964=CARTESIAN_POINT('Ctrl Pts',(19.0540100416943,-10.7935747414879,0.));
#31965=CARTESIAN_POINT('Ctrl Pts',(19.0540100416943,-10.7935747414879,18.));
#31966=CARTESIAN_POINT('Ctrl Pts',(19.0113586878152,-10.7191193896586,0.));
#31967=CARTESIAN_POINT('Ctrl Pts',(19.0113586878152,-10.7191193896586,18.));
#31968=CARTESIAN_POINT('Ctrl Pts',(18.9682247574834,-10.6451561585969,0.));
#31969=CARTESIAN_POINT('Ctrl Pts',(18.9682247574834,-10.6451561585969,18.));
#31970=CARTESIAN_POINT('Ctrl Pts',(18.9246077453188,-10.5716914651544,0.));
#31971=CARTESIAN_POINT('Ctrl Pts',(18.9246077453188,-10.5716914651544,18.));
#31972=CARTESIAN_POINT('Ctrl Pts',(18.8805076729356,-10.4987309368494,0.));
#31973=CARTESIAN_POINT('Ctrl Pts',(18.8805076729356,-10.4987309368494,18.));
#31974=CARTESIAN_POINT('Ctrl Pts',(18.8359245594214,-10.4262802670211,0.));
#31975=CARTESIAN_POINT('Ctrl Pts',(18.8359245594214,-10.4262802670211,18.));
#31976=CARTESIAN_POINT('Ctrl Pts',(18.7908579693851,-10.3543459451258,0.));
#31977=CARTESIAN_POINT('Ctrl Pts',(18.7908579693851,-10.3543459451258,18.));
#31978=CARTESIAN_POINT('Ctrl Pts',(18.7453065790062,-10.2829359603685,0.));
#31979=CARTESIAN_POINT('Ctrl Pts',(18.7453065790062,-10.2829359603685,18.));
#31980=CARTESIAN_POINT('Ctrl Pts',(18.699267629819,-10.2120606864872,0.));
#31981=CARTESIAN_POINT('Ctrl Pts',(18.699267629819,-10.2120606864872,18.));
#31982=CARTESIAN_POINT('Ctrl Pts',(18.6527367592664,-10.1417331637795,0.));
#31983=CARTESIAN_POINT('Ctrl Pts',(18.6527367592664,-10.1417331637795,18.));
#31984=CARTESIAN_POINT('Ctrl Pts',(18.605709190442,-10.0719672018851,0.));
#31985=CARTESIAN_POINT('Ctrl Pts',(18.605709190442,-10.0719672018851,18.));
#31986=CARTESIAN_POINT('Ctrl Pts',(18.5581807679204,-10.0027757313807,0.));
#31987=CARTESIAN_POINT('Ctrl Pts',(18.5581807679204,-10.0027757313807,18.));
#31988=CARTESIAN_POINT('Ctrl Pts',(18.5101489409161,-9.93416923996829,0.));
#31989=CARTESIAN_POINT('Ctrl Pts',(18.5101489409161,-9.93416923996829,18.));
#31990=CARTESIAN_POINT('Ctrl Pts',(18.461614050347,-9.86615372541685,0.));
#31991=CARTESIAN_POINT('Ctrl Pts',(18.461614050347,-9.86615372541685,18.));
#31992=CARTESIAN_POINT('Ctrl Pts',(18.4125796444662,-9.79873019947434,0.));
#31993=CARTESIAN_POINT('Ctrl Pts',(18.4125796444662,-9.79873019947434,18.));
#31994=CARTESIAN_POINT('Ctrl Pts',(18.3630495772677,-9.73189932619939,0.));
#31995=CARTESIAN_POINT('Ctrl Pts',(18.3630495772677,-9.73189932619939,18.));
#31996=CARTESIAN_POINT('Ctrl Pts',(18.3130254811852,-9.6656654640326,0.));
#31997=CARTESIAN_POINT('Ctrl Pts',(18.3130254811852,-9.6656654640326,18.));
#31998=CARTESIAN_POINT('Ctrl Pts',(18.2625044208165,-9.60004042085347,0.));
#31999=CARTESIAN_POINT('Ctrl Pts',(18.2625044208165,-9.60004042085347,18.));
#32000=CARTESIAN_POINT('Ctrl Pts',(18.2114756946126,-9.53504856811686,0.));
#32001=CARTESIAN_POINT('Ctrl Pts',(18.2114756946126,-9.53504856811686,18.));
#32002=CARTESIAN_POINT('Ctrl Pts',(18.1599204445014,-9.47072748065832,0.));
#32003=CARTESIAN_POINT('Ctrl Pts',(18.1599204445014,-9.47072748065832,18.));
#32004=CARTESIAN_POINT('Ctrl Pts',(18.1078184146735,-9.40711718355464,0.));
#32005=CARTESIAN_POINT('Ctrl Pts',(18.1078184146735,-9.40711718355464,18.));
#32006=CARTESIAN_POINT('Ctrl Pts',(18.0551538338035,-9.34425079614396,0.));
#32007=CARTESIAN_POINT('Ctrl Pts',(18.0551538338035,-9.34425079614396,18.));
#32008=CARTESIAN_POINT('Ctrl Pts',(18.0019206847747,-9.28214615574471,0.));
#32009=CARTESIAN_POINT('Ctrl Pts',(18.0019206847747,-9.28214615574471,18.));
#32010=CARTESIAN_POINT('Ctrl Pts',(17.9481305624284,-9.22079331175917,0.));
#32011=CARTESIAN_POINT('Ctrl Pts',(17.9481305624284,-9.22079331175917,18.));
#32012=CARTESIAN_POINT('Ctrl Pts',(17.8938116696237,-9.1601561636161,0.));
#32013=CARTESIAN_POINT('Ctrl Pts',(17.8938116696237,-9.1601561636161,18.));
#32014=CARTESIAN_POINT('Ctrl Pts',(17.8389924349283,-9.10019864472208,0.));
#32015=CARTESIAN_POINT('Ctrl Pts',(17.8389924349283,-9.10019864472208,18.));
#32016=CARTESIAN_POINT('Ctrl Pts',(17.7836872744016,-9.04090748239097,0.));
#32017=CARTESIAN_POINT('Ctrl Pts',(17.7836872744016,-9.04090748239097,18.));
#32018=CARTESIAN_POINT('Ctrl Pts',(17.7278841963319,-8.98231202490686,0.));
#32019=CARTESIAN_POINT('Ctrl Pts',(17.7278841963319,-8.98231202490686,18.));
#32020=CARTESIAN_POINT('Ctrl Pts',(17.6715250120654,-8.92451585185175,0.));
#32021=CARTESIAN_POINT('Ctrl Pts',(17.6715250120654,-8.92451585185175,18.));
#32022=CARTESIAN_POINT('Ctrl Pts',(17.614513388992,-8.86768402115344,0.));
#32023=CARTESIAN_POINT('Ctrl Pts',(17.614513388992,-8.86768402115344,18.));
#32024=CARTESIAN_POINT('Ctrl Pts',(17.5567525798882,-8.81198307239551,0.));
#32025=CARTESIAN_POINT('Ctrl Pts',(17.5567525798882,-8.81198307239551,18.));
#32026=CARTESIAN_POINT('Ctrl Pts',(17.4981785296199,-8.75752832625955,0.));
#32027=CARTESIAN_POINT('Ctrl Pts',(17.4981785296199,-8.75752832625955,18.));
#32028=CARTESIAN_POINT('Ctrl Pts',(17.438788019753,-8.70433925112174,0.));
#32029=CARTESIAN_POINT('Ctrl Pts',(17.438788019753,-8.70433925112174,18.));
#32030=CARTESIAN_POINT('Ctrl Pts',(17.3786861166843,-8.65226368112816,0.));
#32031=CARTESIAN_POINT('Ctrl Pts',(17.3786861166843,-8.65226368112816,18.));
#32032=CARTESIAN_POINT('Ctrl Pts',(17.3180459442745,-8.60104338529165,0.));
#32033=CARTESIAN_POINT('Ctrl Pts',(17.3180459442745,-8.60104338529165,18.));
#32034=CARTESIAN_POINT('Ctrl Pts',(17.2570167183611,-8.55046295192434,0.));
#32035=CARTESIAN_POINT('Ctrl Pts',(17.2570167183611,-8.55046295192434,18.));
#32036=CARTESIAN_POINT('Ctrl Pts',(17.1956428575086,-8.50048099003883,0.));
#32037=CARTESIAN_POINT('Ctrl Pts',(17.1956428575086,-8.50048099003883,18.));
#32038=CARTESIAN_POINT('Ctrl Pts',(17.1337886602855,-8.45135198307877,0.));
#32039=CARTESIAN_POINT('Ctrl Pts',(17.1337886602855,-8.45135198307877,18.));
#32040=CARTESIAN_POINT('Ctrl Pts',(17.071033847921,-8.40379607744266,0.));
#32041=CARTESIAN_POINT('Ctrl Pts',(17.071033847921,-8.40379607744266,18.));
#32042=CARTESIAN_POINT('Ctrl Pts',(17.0067806259695,-8.35882146841244,0.));
#32043=CARTESIAN_POINT('Ctrl Pts',(17.0067806259695,-8.35882146841244,18.));
#32044=CARTESIAN_POINT('Ctrl Pts',(16.9536879065132,-8.32573081382563,0.));
#32045=CARTESIAN_POINT('Ctrl Pts',(16.9536879065132,-8.32573081382563,18.));
#32046=CARTESIAN_POINT('Ctrl Pts',(16.9126979078877,-8.30290517019115,0.));
#32047=CARTESIAN_POINT('Ctrl Pts',(16.9126979078877,-8.30290517019115,18.));
#32048=CARTESIAN_POINT('Ctrl Pts',(16.8848228151885,-8.28862062120315,0.));
#32049=CARTESIAN_POINT('Ctrl Pts',(16.8848228151885,-8.28862062120315,18.));
#32050=CARTESIAN_POINT('Ctrl Pts',(16.8707481591095,-8.28171148831561,0.));
#32051=CARTESIAN_POINT('Ctrl Pts',(16.8707481591095,-8.28171148831561,18.));
#32052=CARTESIAN_POINT('',(20.0837475345525,-13.1393715591102,0.));
#32053=CARTESIAN_POINT('Ctrl Pts',(16.8707481591095,-8.28171148831561,0.));
#32054=CARTESIAN_POINT('Ctrl Pts',(16.8848228151885,-8.28862062120315,0.));
#32055=CARTESIAN_POINT('Ctrl Pts',(16.9126979078877,-8.30290517019115,0.));
#32056=CARTESIAN_POINT('Ctrl Pts',(16.9536879065132,-8.32573081382563,0.));
#32057=CARTESIAN_POINT('Ctrl Pts',(17.0067806259695,-8.35882146841244,0.));
#32058=CARTESIAN_POINT('Ctrl Pts',(17.071033847921,-8.40379607744266,0.));
#32059=CARTESIAN_POINT('Ctrl Pts',(17.1337886602855,-8.45135198307877,0.));
#32060=CARTESIAN_POINT('Ctrl Pts',(17.1956428575086,-8.50048099003883,0.));
#32061=CARTESIAN_POINT('Ctrl Pts',(17.2570167183611,-8.55046295192434,0.));
#32062=CARTESIAN_POINT('Ctrl Pts',(17.3180459442745,-8.60104338529165,0.));
#32063=CARTESIAN_POINT('Ctrl Pts',(17.3786861166843,-8.65226368112816,0.));
#32064=CARTESIAN_POINT('Ctrl Pts',(17.438788019753,-8.70433925112174,0.));
#32065=CARTESIAN_POINT('Ctrl Pts',(17.4981785296199,-8.75752832625955,0.));
#32066=CARTESIAN_POINT('Ctrl Pts',(17.5567525798882,-8.81198307239551,0.));
#32067=CARTESIAN_POINT('Ctrl Pts',(17.614513388992,-8.86768402115344,0.));
#32068=CARTESIAN_POINT('Ctrl Pts',(17.6715250120654,-8.92451585185175,0.));
#32069=CARTESIAN_POINT('Ctrl Pts',(17.7278841963319,-8.98231202490686,0.));
#32070=CARTESIAN_POINT('Ctrl Pts',(17.7836872744016,-9.04090748239097,0.));
#32071=CARTESIAN_POINT('Ctrl Pts',(17.8389924349283,-9.10019864472208,0.));
#32072=CARTESIAN_POINT('Ctrl Pts',(17.8938116696237,-9.1601561636161,0.));
#32073=CARTESIAN_POINT('Ctrl Pts',(17.9481305624284,-9.22079331175917,0.));
#32074=CARTESIAN_POINT('Ctrl Pts',(18.0019206847747,-9.28214615574471,0.));
#32075=CARTESIAN_POINT('Ctrl Pts',(18.0551538338035,-9.34425079614396,0.));
#32076=CARTESIAN_POINT('Ctrl Pts',(18.1078184146735,-9.40711718355464,0.));
#32077=CARTESIAN_POINT('Ctrl Pts',(18.1599204445014,-9.47072748065832,0.));
#32078=CARTESIAN_POINT('Ctrl Pts',(18.2114756946126,-9.53504856811686,0.));
#32079=CARTESIAN_POINT('Ctrl Pts',(18.2625044208165,-9.60004042085347,0.));
#32080=CARTESIAN_POINT('Ctrl Pts',(18.3130254811852,-9.6656654640326,0.));
#32081=CARTESIAN_POINT('Ctrl Pts',(18.3630495772677,-9.73189932619939,0.));
#32082=CARTESIAN_POINT('Ctrl Pts',(18.4125796444662,-9.79873019947434,0.));
#32083=CARTESIAN_POINT('Ctrl Pts',(18.461614050347,-9.86615372541685,0.));
#32084=CARTESIAN_POINT('Ctrl Pts',(18.5101489409161,-9.93416923996829,0.));
#32085=CARTESIAN_POINT('Ctrl Pts',(18.5581807679204,-10.0027757313807,0.));
#32086=CARTESIAN_POINT('Ctrl Pts',(18.605709190442,-10.0719672018851,0.));
#32087=CARTESIAN_POINT('Ctrl Pts',(18.6527367592664,-10.1417331637795,0.));
#32088=CARTESIAN_POINT('Ctrl Pts',(18.699267629819,-10.2120606864872,0.));
#32089=CARTESIAN_POINT('Ctrl Pts',(18.7453065790062,-10.2829359603685,0.));
#32090=CARTESIAN_POINT('Ctrl Pts',(18.7908579693851,-10.3543459451258,0.));
#32091=CARTESIAN_POINT('Ctrl Pts',(18.8359245594214,-10.4262802670211,0.));
#32092=CARTESIAN_POINT('Ctrl Pts',(18.8805076729356,-10.4987309368494,0.));
#32093=CARTESIAN_POINT('Ctrl Pts',(18.9246077453188,-10.5716914651544,0.));
#32094=CARTESIAN_POINT('Ctrl Pts',(18.9682247574834,-10.6451561585969,0.));
#32095=CARTESIAN_POINT('Ctrl Pts',(19.0113586878152,-10.7191193896586,0.));
#32096=CARTESIAN_POINT('Ctrl Pts',(19.0540100416943,-10.7935747414879,0.));
#32097=CARTESIAN_POINT('Ctrl Pts',(19.0961797996403,-10.868515097783,0.));
#32098=CARTESIAN_POINT('Ctrl Pts',(19.1378691901023,-10.9439330179206,0.));
#32099=CARTESIAN_POINT('Ctrl Pts',(19.1790795192393,-11.0198210228993,0.));
#32100=CARTESIAN_POINT('Ctrl Pts',(19.2198119937835,-11.0961718903994,0.));
#32101=CARTESIAN_POINT('Ctrl Pts',(19.2600675167206,-11.1729790050543,0.));
#32102=CARTESIAN_POINT('Ctrl Pts',(19.2998466936739,-11.2502363198588,0.));
#32103=CARTESIAN_POINT('Ctrl Pts',(19.3391499248083,-11.3279381634523,0.));
#32104=CARTESIAN_POINT('Ctrl Pts',(19.3779774742875,-11.4060790880015,0.));
#32105=CARTESIAN_POINT('Ctrl Pts',(19.4163295466324,-11.4846537135043,0.));
#32106=CARTESIAN_POINT('Ctrl Pts',(19.4542063779876,-11.5636565297382,0.));
#32107=CARTESIAN_POINT('Ctrl Pts',(19.4916082541529,-11.6430819099846,0.));
#32108=CARTESIAN_POINT('Ctrl Pts',(19.5285354853626,-11.722924244195,0.));
#32109=CARTESIAN_POINT('Ctrl Pts',(19.5649883985826,-11.8031780389346,0.));
#32110=CARTESIAN_POINT('Ctrl Pts',(19.6009673241771,-11.8838380136222,0.));
#32111=CARTESIAN_POINT('Ctrl Pts',(19.6364725931695,-11.9648992312094,0.));
#32112=CARTESIAN_POINT('Ctrl Pts',(19.6715045149944,-12.0463570680309,0.));
#32113=CARTESIAN_POINT('Ctrl Pts',(19.7060633406705,-12.1282070378972,0.));
#32114=CARTESIAN_POINT('Ctrl Pts',(19.7401492304335,-12.2104446447874,0.));
#32115=CARTESIAN_POINT('Ctrl Pts',(19.7737622285562,-12.2930652417987,0.));
#32116=CARTESIAN_POINT('Ctrl Pts',(19.8069022248387,-12.3760638341708,0.));
#32117=CARTESIAN_POINT('Ctrl Pts',(19.839568972011,-12.4594350764989,0.));
#32118=CARTESIAN_POINT('Ctrl Pts',(19.8717621942733,-12.5431736030596,0.));
#32119=CARTESIAN_POINT('Ctrl Pts',(19.9034816813503,-12.6272742843372,0.));
#32120=CARTESIAN_POINT('Ctrl Pts',(19.9347273847264,-12.7117325003719,0.));
#32121=CARTESIAN_POINT('Ctrl Pts',(19.9654995335894,-12.7965444294443,0.));
#32122=CARTESIAN_POINT('Ctrl Pts',(20.0018585267766,-12.8987398182747,0.));
#32123=CARTESIAN_POINT('Ctrl Pts',(20.0315673466055,-12.9843387891477,0.));
#32124=CARTESIAN_POINT('Ctrl Pts',(20.054957345404,-13.0530957702829,0.));
#32125=CARTESIAN_POINT('Ctrl Pts',(20.0722879610899,-13.1048196144678,0.));
#32126=CARTESIAN_POINT('Ctrl Pts',(20.0837475345526,-13.1393715591102,0.));
#32127=CARTESIAN_POINT('',(20.0837475345525,-13.1393715591102,15.));
#32128=CARTESIAN_POINT('Ctrl Pts',(20.0837475345526,-13.1393715591102,15.));
#32129=CARTESIAN_POINT('Ctrl Pts',(20.0780177478283,-13.1220955868173,15.));
#32130=CARTESIAN_POINT('Ctrl Pts',(20.0665110891946,-13.0875783330728,15.));
#32131=CARTESIAN_POINT('Ctrl Pts',(20.0491098457044,-13.0359065249991,15.));
#32132=CARTESIAN_POINT('Ctrl Pts',(20.0256255826397,-12.9672189949731,15.));
#32133=CARTESIAN_POINT('Ctrl Pts',(19.9957986945787,-12.8817072534696,15.));
#32134=CARTESIAN_POINT('Ctrl Pts',(19.9654995335894,-12.7965444294443,15.));
#32135=CARTESIAN_POINT('Ctrl Pts',(19.9347273847264,-12.7117325003719,15.));
#32136=CARTESIAN_POINT('Ctrl Pts',(19.9034816813503,-12.6272742843372,15.));
#32137=CARTESIAN_POINT('Ctrl Pts',(19.8717621942733,-12.5431736030596,15.));
#32138=CARTESIAN_POINT('Ctrl Pts',(19.839568972011,-12.4594350764989,15.));
#32139=CARTESIAN_POINT('Ctrl Pts',(19.8069022248387,-12.3760638341708,15.));
#32140=CARTESIAN_POINT('Ctrl Pts',(19.7737622285562,-12.2930652417987,15.));
#32141=CARTESIAN_POINT('Ctrl Pts',(19.7401492304335,-12.2104446447874,15.));
#32142=CARTESIAN_POINT('Ctrl Pts',(19.7060633406705,-12.1282070378972,15.));
#32143=CARTESIAN_POINT('Ctrl Pts',(19.6715045149944,-12.0463570680309,15.));
#32144=CARTESIAN_POINT('Ctrl Pts',(19.6364725931695,-11.9648992312094,15.));
#32145=CARTESIAN_POINT('Ctrl Pts',(19.6009673241771,-11.8838380136222,15.));
#32146=CARTESIAN_POINT('Ctrl Pts',(19.5649883985826,-11.8031780389346,15.));
#32147=CARTESIAN_POINT('Ctrl Pts',(19.5285354853626,-11.722924244195,15.));
#32148=CARTESIAN_POINT('Ctrl Pts',(19.4916082541529,-11.6430819099846,15.));
#32149=CARTESIAN_POINT('Ctrl Pts',(19.4542063779876,-11.5636565297382,15.));
#32150=CARTESIAN_POINT('Ctrl Pts',(19.4163295466324,-11.4846537135043,15.));
#32151=CARTESIAN_POINT('Ctrl Pts',(19.3779774742875,-11.4060790880015,15.));
#32152=CARTESIAN_POINT('Ctrl Pts',(19.3391499248083,-11.3279381634523,15.));
#32153=CARTESIAN_POINT('Ctrl Pts',(19.2998466936739,-11.2502363198588,15.));
#32154=CARTESIAN_POINT('Ctrl Pts',(19.2600675167206,-11.1729790050543,15.));
#32155=CARTESIAN_POINT('Ctrl Pts',(19.2198119937835,-11.0961718903994,15.));
#32156=CARTESIAN_POINT('Ctrl Pts',(19.1790795192393,-11.0198210228993,15.));
#32157=CARTESIAN_POINT('Ctrl Pts',(19.1378691901023,-10.9439330179206,15.));
#32158=CARTESIAN_POINT('Ctrl Pts',(19.0961797996403,-10.868515097783,15.));
#32159=CARTESIAN_POINT('Ctrl Pts',(19.0540100416943,-10.7935747414879,15.));
#32160=CARTESIAN_POINT('Ctrl Pts',(19.0113586878152,-10.7191193896586,15.));
#32161=CARTESIAN_POINT('Ctrl Pts',(18.9682247574834,-10.6451561585969,15.));
#32162=CARTESIAN_POINT('Ctrl Pts',(18.9246077453188,-10.5716914651544,15.));
#32163=CARTESIAN_POINT('Ctrl Pts',(18.8805076729356,-10.4987309368494,15.));
#32164=CARTESIAN_POINT('Ctrl Pts',(18.8359245594214,-10.4262802670211,15.));
#32165=CARTESIAN_POINT('Ctrl Pts',(18.7908579693851,-10.3543459451258,15.));
#32166=CARTESIAN_POINT('Ctrl Pts',(18.7453065790062,-10.2829359603685,15.));
#32167=CARTESIAN_POINT('Ctrl Pts',(18.699267629819,-10.2120606864872,15.));
#32168=CARTESIAN_POINT('Ctrl Pts',(18.6527367592664,-10.1417331637795,15.));
#32169=CARTESIAN_POINT('Ctrl Pts',(18.605709190442,-10.0719672018851,15.));
#32170=CARTESIAN_POINT('Ctrl Pts',(18.5581807679204,-10.0027757313807,15.));
#32171=CARTESIAN_POINT('Ctrl Pts',(18.5101489409161,-9.93416923996829,15.));
#32172=CARTESIAN_POINT('Ctrl Pts',(18.461614050347,-9.86615372541685,15.));
#32173=CARTESIAN_POINT('Ctrl Pts',(18.4125796444662,-9.79873019947434,15.));
#32174=CARTESIAN_POINT('Ctrl Pts',(18.3630495772677,-9.73189932619939,15.));
#32175=CARTESIAN_POINT('Ctrl Pts',(18.3130254811852,-9.6656654640326,15.));
#32176=CARTESIAN_POINT('Ctrl Pts',(18.2625044208165,-9.60004042085347,15.));
#32177=CARTESIAN_POINT('Ctrl Pts',(18.2114756946126,-9.53504856811686,15.));
#32178=CARTESIAN_POINT('Ctrl Pts',(18.1599204445014,-9.47072748065832,15.));
#32179=CARTESIAN_POINT('Ctrl Pts',(18.1078184146735,-9.40711718355464,15.));
#32180=CARTESIAN_POINT('Ctrl Pts',(18.0551538338035,-9.34425079614396,15.));
#32181=CARTESIAN_POINT('Ctrl Pts',(18.0019206847747,-9.28214615574471,15.));
#32182=CARTESIAN_POINT('Ctrl Pts',(17.9481305624284,-9.22079331175917,15.));
#32183=CARTESIAN_POINT('Ctrl Pts',(17.8938116696237,-9.1601561636161,15.));
#32184=CARTESIAN_POINT('Ctrl Pts',(17.8389924349283,-9.10019864472208,15.));
#32185=CARTESIAN_POINT('Ctrl Pts',(17.7836872744016,-9.04090748239097,15.));
#32186=CARTESIAN_POINT('Ctrl Pts',(17.7278841963319,-8.98231202490686,15.));
#32187=CARTESIAN_POINT('Ctrl Pts',(17.6715250120654,-8.92451585185175,15.));
#32188=CARTESIAN_POINT('Ctrl Pts',(17.614513388992,-8.86768402115344,15.));
#32189=CARTESIAN_POINT('Ctrl Pts',(17.5567525798882,-8.81198307239551,15.));
#32190=CARTESIAN_POINT('Ctrl Pts',(17.4981785296199,-8.75752832625955,15.));
#32191=CARTESIAN_POINT('Ctrl Pts',(17.438788019753,-8.70433925112174,15.));
#32192=CARTESIAN_POINT('Ctrl Pts',(17.3786861166843,-8.65226368112816,15.));
#32193=CARTESIAN_POINT('Ctrl Pts',(17.3180459442745,-8.60104338529165,15.));
#32194=CARTESIAN_POINT('Ctrl Pts',(17.2570167183611,-8.55046295192434,15.));
#32195=CARTESIAN_POINT('Ctrl Pts',(17.1956428575086,-8.50048099003883,15.));
#32196=CARTESIAN_POINT('Ctrl Pts',(17.1337886602855,-8.45135198307877,15.));
#32197=CARTESIAN_POINT('Ctrl Pts',(17.071033847921,-8.40379607744266,15.));
#32198=CARTESIAN_POINT('Ctrl Pts',(17.0067806259695,-8.35882146841244,15.));
#32199=CARTESIAN_POINT('Ctrl Pts',(16.9536879065132,-8.32573081382563,15.));
#32200=CARTESIAN_POINT('Ctrl Pts',(16.9126979078877,-8.30290517019115,15.));
#32201=CARTESIAN_POINT('Ctrl Pts',(16.8848228151885,-8.28862062120315,15.));
#32202=CARTESIAN_POINT('Ctrl Pts',(16.8707481591095,-8.28171148831561,15.));
#32203=CARTESIAN_POINT('',(20.0837475345525,-13.1393715591102,0.));
#32204=CARTESIAN_POINT('Origin',(9.33709008296438E-14,-6.79236997764462E-14,
0.));
#32205=CARTESIAN_POINT('',(18.7025042402277,-15.0404898571911,0.));
#32206=CARTESIAN_POINT('Origin',(9.33709008296438E-14,-6.79236997764462E-14,
0.));
#32207=CARTESIAN_POINT('',(18.7025042402277,-15.0404898571911,15.));
#32208=CARTESIAN_POINT('Origin',(9.33709008296438E-14,-6.79236997764462E-14,
15.));
#32209=CARTESIAN_POINT('',(18.7025042402277,-15.0404898571911,0.));
#32210=CARTESIAN_POINT('Ctrl Pts',(13.0897235660237,-13.4858453790958,0.));
#32211=CARTESIAN_POINT('Ctrl Pts',(13.0897235660237,-13.4858453790958,18.));
#32212=CARTESIAN_POINT('Ctrl Pts',(13.1006438497967,-13.4970961329957,0.));
#32213=CARTESIAN_POINT('Ctrl Pts',(13.1006438497967,-13.4970961329957,18.));
#32214=CARTESIAN_POINT('Ctrl Pts',(13.1228431405579,-13.5191927531554,0.));
#32215=CARTESIAN_POINT('Ctrl Pts',(13.1228431405579,-13.5191927531554,18.));
#32216=CARTESIAN_POINT('Ctrl Pts',(13.1572182238498,-13.5511230466604,0.));
#32217=CARTESIAN_POINT('Ctrl Pts',(13.1572182238498,-13.5511230466604,18.));
#32218=CARTESIAN_POINT('Ctrl Pts',(13.2050958591127,-13.5913916488449,0.));
#32219=CARTESIAN_POINT('Ctrl Pts',(13.2050958591127,-13.5913916488449,18.));
#32220=CARTESIAN_POINT('Ctrl Pts',(13.267724591625,-13.6386021757691,0.));
#32221=CARTESIAN_POINT('Ctrl Pts',(13.267724591625,-13.6386021757691,18.));
#32222=CARTESIAN_POINT('Ctrl Pts',(13.332345249068,-13.6835899659728,0.));
#32223=CARTESIAN_POINT('Ctrl Pts',(13.332345249068,-13.6835899659728,18.));
#32224=CARTESIAN_POINT('Ctrl Pts',(13.3981837093918,-13.7272351052346,0.));
#32225=CARTESIAN_POINT('Ctrl Pts',(13.3981837093918,-13.7272351052346,18.));
#32226=CARTESIAN_POINT('Ctrl Pts',(13.4646849459541,-13.7701598398937,0.));
#32227=CARTESIAN_POINT('Ctrl Pts',(13.4646849459541,-13.7701598398937,18.));
#32228=CARTESIAN_POINT('Ctrl Pts',(13.5316488646659,-13.8125718693898,0.));
#32229=CARTESIAN_POINT('Ctrl Pts',(13.5316488646659,-13.8125718693898,18.));
#32230=CARTESIAN_POINT('Ctrl Pts',(13.5991011046042,-13.854416158639,0.));
#32231=CARTESIAN_POINT('Ctrl Pts',(13.5991011046042,-13.854416158639,18.));
#32232=CARTESIAN_POINT('Ctrl Pts',(13.6672004242289,-13.8954842290745,0.));
#32233=CARTESIAN_POINT('Ctrl Pts',(13.6672004242289,-13.8954842290745,18.));
#32234=CARTESIAN_POINT('Ctrl Pts',(13.7361389175879,-13.9355316323567,0.));
#32235=CARTESIAN_POINT('Ctrl Pts',(13.7361389175879,-13.9355316323567,18.));
#32236=CARTESIAN_POINT('Ctrl Pts',(13.806028835706,-13.9744114225699,0.));
#32237=CARTESIAN_POINT('Ctrl Pts',(13.806028835706,-13.9744114225699,18.));
#32238=CARTESIAN_POINT('Ctrl Pts',(13.876852657608,-14.0121326766855,0.));
#32239=CARTESIAN_POINT('Ctrl Pts',(13.876852657608,-14.0121326766855,18.));
#32240=CARTESIAN_POINT('Ctrl Pts',(13.9485205009332,-14.0487919508068,0.));
#32241=CARTESIAN_POINT('Ctrl Pts',(13.9485205009332,-14.0487919508068,18.));
#32242=CARTESIAN_POINT('Ctrl Pts',(14.0209038736616,-14.0845327205726,0.));
#32243=CARTESIAN_POINT('Ctrl Pts',(14.0209038736616,-14.0845327205726,18.));
#32244=CARTESIAN_POINT('Ctrl Pts',(14.0938755647891,-14.1194976094444,0.));
#32245=CARTESIAN_POINT('Ctrl Pts',(14.0938755647891,-14.1194976094444,18.));
#32246=CARTESIAN_POINT('Ctrl Pts',(14.1673550455622,-14.1537739659715,0.));
#32247=CARTESIAN_POINT('Ctrl Pts',(14.1673550455622,-14.1537739659715,18.));
#32248=CARTESIAN_POINT('Ctrl Pts',(14.2413181097468,-14.1873822640681,0.));
#32249=CARTESIAN_POINT('Ctrl Pts',(14.2413181097468,-14.1873822640681,18.));
#32250=CARTESIAN_POINT('Ctrl Pts',(14.3157729256101,-14.2203046917613,0.));
#32251=CARTESIAN_POINT('Ctrl Pts',(14.3157729256101,-14.2203046917613,18.));
#32252=CARTESIAN_POINT('Ctrl Pts',(14.3907450096103,-14.2525030666863,0.));
#32253=CARTESIAN_POINT('Ctrl Pts',(14.3907450096103,-14.2525030666863,18.));
#32254=CARTESIAN_POINT('Ctrl Pts',(14.4662599802681,-14.2839394106401,0.));
#32255=CARTESIAN_POINT('Ctrl Pts',(14.4662599802681,-14.2839394106401,18.));
#32256=CARTESIAN_POINT('Ctrl Pts',(14.5423237181615,-14.3145996213697,0.));
#32257=CARTESIAN_POINT('Ctrl Pts',(14.5423237181615,-14.3145996213697,18.));
#32258=CARTESIAN_POINT('Ctrl Pts',(14.6189211183837,-14.3444949335274,0.));
#32259=CARTESIAN_POINT('Ctrl Pts',(14.6189211183837,-14.3444949335274,18.));
#32260=CARTESIAN_POINT('Ctrl Pts',(14.6960255561799,-14.3736505809735,0.));
#32261=CARTESIAN_POINT('Ctrl Pts',(14.6960255561799,-14.3736505809735,18.));
#32262=CARTESIAN_POINT('Ctrl Pts',(14.7736052248294,-14.4020981965564,0.));
#32263=CARTESIAN_POINT('Ctrl Pts',(14.7736052248294,-14.4020981965564,18.));
#32264=CARTESIAN_POINT('Ctrl Pts',(14.8516302160049,-14.4298673266313,0.));
#32265=CARTESIAN_POINT('Ctrl Pts',(14.8516302160049,-14.4298673266313,18.));
#32266=CARTESIAN_POINT('Ctrl Pts',(14.9300806580357,-14.4569756801697,0.));
#32267=CARTESIAN_POINT('Ctrl Pts',(14.9300806580357,-14.4569756801697,18.));
#32268=CARTESIAN_POINT('Ctrl Pts',(15.0089462280504,-14.4834296977405,0.));
#32269=CARTESIAN_POINT('Ctrl Pts',(15.0089462280504,-14.4834296977405,18.));
#32270=CARTESIAN_POINT('Ctrl Pts',(15.0882222764759,-14.5092291736391,0.));
#32271=CARTESIAN_POINT('Ctrl Pts',(15.0882222764759,-14.5092291736391,18.));
#32272=CARTESIAN_POINT('Ctrl Pts',(15.1679069808052,-14.5343706477051,0.));
#32273=CARTESIAN_POINT('Ctrl Pts',(15.1679069808052,-14.5343706477051,18.));
#32274=CARTESIAN_POINT('Ctrl Pts',(15.2479982823383,-14.5588510579962,0.));
#32275=CARTESIAN_POINT('Ctrl Pts',(15.2479982823383,-14.5588510579962,18.));
#32276=CARTESIAN_POINT('Ctrl Pts',(15.3284903715086,-14.5826719336929,0.));
#32277=CARTESIAN_POINT('Ctrl Pts',(15.3284903715086,-14.5826719336929,18.));
#32278=CARTESIAN_POINT('Ctrl Pts',(15.4093740621547,-14.6058389416146,0.));
#32279=CARTESIAN_POINT('Ctrl Pts',(15.4093740621547,-14.6058389416146,18.));
#32280=CARTESIAN_POINT('Ctrl Pts',(15.4906383406647,-14.6283600295736,0.));
#32281=CARTESIAN_POINT('Ctrl Pts',(15.4906383406647,-14.6283600295736,18.));
#32282=CARTESIAN_POINT('Ctrl Pts',(15.5722715494357,-14.6502440080912,0.));
#32283=CARTESIAN_POINT('Ctrl Pts',(15.5722715494357,-14.6502440080912,18.));
#32284=CARTESIAN_POINT('Ctrl Pts',(15.6542626345121,-14.6714990558793,0.));
#32285=CARTESIAN_POINT('Ctrl Pts',(15.6542626345121,-14.6714990558793,18.));
#32286=CARTESIAN_POINT('Ctrl Pts',(15.7366025822956,-14.692131002056,0.));
#32287=CARTESIAN_POINT('Ctrl Pts',(15.7366025822956,-14.692131002056,18.));
#32288=CARTESIAN_POINT('Ctrl Pts',(15.8192842036838,-14.7121435744495,0.));
#32289=CARTESIAN_POINT('Ctrl Pts',(15.8192842036838,-14.7121435744495,18.));
#32290=CARTESIAN_POINT('Ctrl Pts',(15.9023014613802,-14.7315391924939,0.));
#32291=CARTESIAN_POINT('Ctrl Pts',(15.9023014613802,-14.7315391924939,18.));
#32292=CARTESIAN_POINT('Ctrl Pts',(15.9856489347991,-14.7503195973741,0.));
#32293=CARTESIAN_POINT('Ctrl Pts',(15.9856489347991,-14.7503195973741,18.));
#32294=CARTESIAN_POINT('Ctrl Pts',(16.0693212651732,-14.7684865075326,0.));
#32295=CARTESIAN_POINT('Ctrl Pts',(16.0693212651732,-14.7684865075326,18.));
#32296=CARTESIAN_POINT('Ctrl Pts',(16.1533125058853,-14.7860423865308,0.));
#32297=CARTESIAN_POINT('Ctrl Pts',(16.1533125058853,-14.7860423865308,18.));
#32298=CARTESIAN_POINT('Ctrl Pts',(16.2376161919272,-14.8029903659562,0.));
#32299=CARTESIAN_POINT('Ctrl Pts',(16.2376161919272,-14.8029903659562,18.));
#32300=CARTESIAN_POINT('Ctrl Pts',(16.3222256264574,-14.8193339134125,0.));
#32301=CARTESIAN_POINT('Ctrl Pts',(16.3222256264574,-14.8193339134125,18.));
#32302=CARTESIAN_POINT('Ctrl Pts',(16.4071341001481,-14.8350765822692,0.));
#32303=CARTESIAN_POINT('Ctrl Pts',(16.4071341001481,-14.8350765822692,18.));
#32304=CARTESIAN_POINT('Ctrl Pts',(16.492335117066,-14.8502217520165,0.));
#32305=CARTESIAN_POINT('Ctrl Pts',(16.492335117066,-14.8502217520165,18.));
#32306=CARTESIAN_POINT('Ctrl Pts',(16.5778226646614,-14.8647723257055,0.));
#32307=CARTESIAN_POINT('Ctrl Pts',(16.5778226646614,-14.8647723257055,18.));
#32308=CARTESIAN_POINT('Ctrl Pts',(16.6635911790385,-14.8787307479454,0.));
#32309=CARTESIAN_POINT('Ctrl Pts',(16.6635911790385,-14.8787307479454,18.));
#32310=CARTESIAN_POINT('Ctrl Pts',(16.7496353900706,-14.8920991518626,0.));
#32311=CARTESIAN_POINT('Ctrl Pts',(16.7496353900706,-14.8920991518626,18.));
#32312=CARTESIAN_POINT('Ctrl Pts',(16.8359501981915,-14.9048794721647,0.));
#32313=CARTESIAN_POINT('Ctrl Pts',(16.8359501981915,-14.9048794721647,18.));
#32314=CARTESIAN_POINT('Ctrl Pts',(16.9225305499155,-14.9170735658747,0.));
#32315=CARTESIAN_POINT('Ctrl Pts',(16.9225305499155,-14.9170735658747,18.));
#32316=CARTESIAN_POINT('Ctrl Pts',(17.0093712776822,-14.9286833603319,0.));
#32317=CARTESIAN_POINT('Ctrl Pts',(17.0093712776822,-14.9286833603319,18.));
#32318=CARTESIAN_POINT('Ctrl Pts',(17.0964671184813,-14.9397108660998,0.));
#32319=CARTESIAN_POINT('Ctrl Pts',(17.0964671184813,-14.9397108660998,18.));
#32320=CARTESIAN_POINT('Ctrl Pts',(17.1838128327073,-14.9501581118289,0.));
#32321=CARTESIAN_POINT('Ctrl Pts',(17.1838128327073,-14.9501581118289,18.));
#32322=CARTESIAN_POINT('Ctrl Pts',(17.2714032968314,-14.9600271060471,0.));
#32323=CARTESIAN_POINT('Ctrl Pts',(17.2714032968314,-14.9600271060471,18.));
#32324=CARTESIAN_POINT('Ctrl Pts',(17.3592335908102,-14.9693197947387,0.));
#32325=CARTESIAN_POINT('Ctrl Pts',(17.3592335908102,-14.9693197947387,18.));
#32326=CARTESIAN_POINT('Ctrl Pts',(17.4472991215239,-14.9780380183576,0.));
#32327=CARTESIAN_POINT('Ctrl Pts',(17.4472991215239,-14.9780380183576,18.));
#32328=CARTESIAN_POINT('Ctrl Pts',(17.5355955872257,-14.9861834999847,0.));
#32329=CARTESIAN_POINT('Ctrl Pts',(17.5355955872257,-14.9861834999847,18.));
#32330=CARTESIAN_POINT('Ctrl Pts',(17.6241187988652,-14.9937578646616,0.));
#32331=CARTESIAN_POINT('Ctrl Pts',(17.6241187988652,-14.9937578646616,18.));
#32332=CARTESIAN_POINT('Ctrl Pts',(17.7128645299878,-15.0007626541287,0.));
#32333=CARTESIAN_POINT('Ctrl Pts',(17.7128645299878,-15.0007626541287,18.));
#32334=CARTESIAN_POINT('Ctrl Pts',(17.8018283748074,-15.0071993464636,0.));
#32335=CARTESIAN_POINT('Ctrl Pts',(17.8018283748074,-15.0071993464636,18.));
#32336=CARTESIAN_POINT('Ctrl Pts',(17.891005548971,-15.0130693803259,0.));
#32337=CARTESIAN_POINT('Ctrl Pts',(17.891005548971,-15.0130693803259,18.));
#32338=CARTESIAN_POINT('Ctrl Pts',(17.980390892286,-15.0183741723687,0.));
#32339=CARTESIAN_POINT('Ctrl Pts',(17.980390892286,-15.0183741723687,18.));
#32340=CARTESIAN_POINT('Ctrl Pts',(18.0699792164192,-15.0231151183906,0.));
#32341=CARTESIAN_POINT('Ctrl Pts',(18.0699792164192,-15.0231151183906,18.));
#32342=CARTESIAN_POINT('Ctrl Pts',(18.1597655779328,-15.0272936035154,0.));
#32343=CARTESIAN_POINT('Ctrl Pts',(18.1597655779328,-15.0272936035154,18.));
#32344=CARTESIAN_POINT('Ctrl Pts',(18.2497455679917,-15.0309110092482,0.));
#32345=CARTESIAN_POINT('Ctrl Pts',(18.2497455679917,-15.0309110092482,18.));
#32346=CARTESIAN_POINT('Ctrl Pts',(18.3399156227477,-15.0339687345357,0.));
#32347=CARTESIAN_POINT('Ctrl Pts',(18.3399156227477,-15.0339687345357,18.));
#32348=CARTESIAN_POINT('Ctrl Pts',(18.430273237144,-15.0364681891201,0.));
#32349=CARTESIAN_POINT('Ctrl Pts',(18.430273237144,-15.0364681891201,18.));
#32350=CARTESIAN_POINT('Ctrl Pts',(18.5208167514208,-15.0384106640282,0.));
#32351=CARTESIAN_POINT('Ctrl Pts',(18.5208167514208,-15.0384106640282,18.));
#32352=CARTESIAN_POINT('Ctrl Pts',(18.5933995108277,-15.0395199113665,0.));
#32353=CARTESIAN_POINT('Ctrl Pts',(18.5933995108277,-15.0395199113665,18.));
#32354=CARTESIAN_POINT('Ctrl Pts',(18.6479196005666,-15.0401020105546,0.));
#32355=CARTESIAN_POINT('Ctrl Pts',(18.6479196005666,-15.0401020105546,18.));
#32356=CARTESIAN_POINT('Ctrl Pts',(18.6843032127312,-15.0403790752228,0.));
#32357=CARTESIAN_POINT('Ctrl Pts',(18.6843032127312,-15.0403790752228,18.));
#32358=CARTESIAN_POINT('Ctrl Pts',(18.7025042402277,-15.0404898571911,0.));
#32359=CARTESIAN_POINT('Ctrl Pts',(18.7025042402277,-15.0404898571911,18.));
#32360=CARTESIAN_POINT('Ctrl Pts',(13.0897235660237,-13.4858453790958,0.));
#32361=CARTESIAN_POINT('Ctrl Pts',(13.1006438497967,-13.4970961329957,0.));
#32362=CARTESIAN_POINT('Ctrl Pts',(13.1228431405579,-13.5191927531554,0.));
#32363=CARTESIAN_POINT('Ctrl Pts',(13.1572182238498,-13.5511230466604,0.));
#32364=CARTESIAN_POINT('Ctrl Pts',(13.2050958591127,-13.5913916488449,0.));
#32365=CARTESIAN_POINT('Ctrl Pts',(13.267724591625,-13.6386021757691,0.));
#32366=CARTESIAN_POINT('Ctrl Pts',(13.332345249068,-13.6835899659728,0.));
#32367=CARTESIAN_POINT('Ctrl Pts',(13.3981837093918,-13.7272351052346,0.));
#32368=CARTESIAN_POINT('Ctrl Pts',(13.4646849459541,-13.7701598398937,0.));
#32369=CARTESIAN_POINT('Ctrl Pts',(13.5316488646659,-13.8125718693898,0.));
#32370=CARTESIAN_POINT('Ctrl Pts',(13.5991011046042,-13.854416158639,0.));
#32371=CARTESIAN_POINT('Ctrl Pts',(13.6672004242289,-13.8954842290745,0.));
#32372=CARTESIAN_POINT('Ctrl Pts',(13.7361389175879,-13.9355316323567,0.));
#32373=CARTESIAN_POINT('Ctrl Pts',(13.806028835706,-13.9744114225699,0.));
#32374=CARTESIAN_POINT('Ctrl Pts',(13.876852657608,-14.0121326766855,0.));
#32375=CARTESIAN_POINT('Ctrl Pts',(13.9485205009332,-14.0487919508068,0.));
#32376=CARTESIAN_POINT('Ctrl Pts',(14.0209038736616,-14.0845327205726,0.));
#32377=CARTESIAN_POINT('Ctrl Pts',(14.0938755647891,-14.1194976094444,0.));
#32378=CARTESIAN_POINT('Ctrl Pts',(14.1673550455622,-14.1537739659715,0.));
#32379=CARTESIAN_POINT('Ctrl Pts',(14.2413181097468,-14.1873822640681,0.));
#32380=CARTESIAN_POINT('Ctrl Pts',(14.3157729256101,-14.2203046917613,0.));
#32381=CARTESIAN_POINT('Ctrl Pts',(14.3907450096103,-14.2525030666863,0.));
#32382=CARTESIAN_POINT('Ctrl Pts',(14.4662599802681,-14.2839394106401,0.));
#32383=CARTESIAN_POINT('Ctrl Pts',(14.5423237181615,-14.3145996213697,0.));
#32384=CARTESIAN_POINT('Ctrl Pts',(14.6189211183837,-14.3444949335274,0.));
#32385=CARTESIAN_POINT('Ctrl Pts',(14.6960255561799,-14.3736505809735,0.));
#32386=CARTESIAN_POINT('Ctrl Pts',(14.7736052248294,-14.4020981965564,0.));
#32387=CARTESIAN_POINT('Ctrl Pts',(14.8516302160049,-14.4298673266313,0.));
#32388=CARTESIAN_POINT('Ctrl Pts',(14.9300806580357,-14.4569756801697,0.));
#32389=CARTESIAN_POINT('Ctrl Pts',(15.0089462280504,-14.4834296977405,0.));
#32390=CARTESIAN_POINT('Ctrl Pts',(15.0882222764759,-14.5092291736391,0.));
#32391=CARTESIAN_POINT('Ctrl Pts',(15.1679069808052,-14.5343706477051,0.));
#32392=CARTESIAN_POINT('Ctrl Pts',(15.2479982823383,-14.5588510579962,0.));
#32393=CARTESIAN_POINT('Ctrl Pts',(15.3284903715086,-14.5826719336929,0.));
#32394=CARTESIAN_POINT('Ctrl Pts',(15.4093740621547,-14.6058389416146,0.));
#32395=CARTESIAN_POINT('Ctrl Pts',(15.4906383406647,-14.6283600295736,0.));
#32396=CARTESIAN_POINT('Ctrl Pts',(15.5722715494357,-14.6502440080912,0.));
#32397=CARTESIAN_POINT('Ctrl Pts',(15.6542626345121,-14.6714990558793,0.));
#32398=CARTESIAN_POINT('Ctrl Pts',(15.7366025822956,-14.692131002056,0.));
#32399=CARTESIAN_POINT('Ctrl Pts',(15.8192842036838,-14.7121435744495,0.));
#32400=CARTESIAN_POINT('Ctrl Pts',(15.9023014613802,-14.7315391924939,0.));
#32401=CARTESIAN_POINT('Ctrl Pts',(15.9856489347991,-14.7503195973741,0.));
#32402=CARTESIAN_POINT('Ctrl Pts',(16.0693212651732,-14.7684865075326,0.));
#32403=CARTESIAN_POINT('Ctrl Pts',(16.1533125058853,-14.7860423865308,0.));
#32404=CARTESIAN_POINT('Ctrl Pts',(16.2376161919272,-14.8029903659562,0.));
#32405=CARTESIAN_POINT('Ctrl Pts',(16.3222256264574,-14.8193339134125,0.));
#32406=CARTESIAN_POINT('Ctrl Pts',(16.4071341001481,-14.8350765822692,0.));
#32407=CARTESIAN_POINT('Ctrl Pts',(16.492335117066,-14.8502217520165,0.));
#32408=CARTESIAN_POINT('Ctrl Pts',(16.5778226646614,-14.8647723257055,0.));
#32409=CARTESIAN_POINT('Ctrl Pts',(16.6635911790385,-14.8787307479454,0.));
#32410=CARTESIAN_POINT('Ctrl Pts',(16.7496353900706,-14.8920991518626,0.));
#32411=CARTESIAN_POINT('Ctrl Pts',(16.8359501981915,-14.9048794721647,0.));
#32412=CARTESIAN_POINT('Ctrl Pts',(16.9225305499155,-14.9170735658747,0.));
#32413=CARTESIAN_POINT('Ctrl Pts',(17.0093712776822,-14.9286833603319,0.));
#32414=CARTESIAN_POINT('Ctrl Pts',(17.0964671184813,-14.9397108660998,0.));
#32415=CARTESIAN_POINT('Ctrl Pts',(17.1838128327073,-14.9501581118289,0.));
#32416=CARTESIAN_POINT('Ctrl Pts',(17.2714032968314,-14.9600271060471,0.));
#32417=CARTESIAN_POINT('Ctrl Pts',(17.3592335908102,-14.9693197947387,0.));
#32418=CARTESIAN_POINT('Ctrl Pts',(17.4472991215239,-14.9780380183576,0.));
#32419=CARTESIAN_POINT('Ctrl Pts',(17.5355955872257,-14.9861834999847,0.));
#32420=CARTESIAN_POINT('Ctrl Pts',(17.6241187988652,-14.9937578646616,0.));
#32421=CARTESIAN_POINT('Ctrl Pts',(17.7128645299878,-15.0007626541287,0.));
#32422=CARTESIAN_POINT('Ctrl Pts',(17.8018283748074,-15.0071993464636,0.));
#32423=CARTESIAN_POINT('Ctrl Pts',(17.891005548971,-15.0130693803259,0.));
#32424=CARTESIAN_POINT('Ctrl Pts',(17.980390892286,-15.0183741723687,0.));
#32425=CARTESIAN_POINT('Ctrl Pts',(18.0699792164192,-15.0231151183906,0.));
#32426=CARTESIAN_POINT('Ctrl Pts',(18.1597655779328,-15.0272936035154,0.));
#32427=CARTESIAN_POINT('Ctrl Pts',(18.2497455679917,-15.0309110092482,0.));
#32428=CARTESIAN_POINT('Ctrl Pts',(18.3399156227477,-15.0339687345357,0.));
#32429=CARTESIAN_POINT('Ctrl Pts',(18.4483447600233,-15.036968080037,0.));
#32430=CARTESIAN_POINT('Ctrl Pts',(18.5389347492702,-15.038771310026,0.));
#32431=CARTESIAN_POINT('Ctrl Pts',(18.6115544313469,-15.0397694451467,0.));
#32432=CARTESIAN_POINT('Ctrl Pts',(18.6661021851765,-15.0402682932586,0.));
#32433=CARTESIAN_POINT('Ctrl Pts',(18.7025042402277,-15.0404898571911,0.));
#32434=CARTESIAN_POINT('Ctrl Pts',(13.0897235660237,-13.4858453790958,15.));
#32435=CARTESIAN_POINT('Ctrl Pts',(13.1006438497967,-13.4970961329957,15.));
#32436=CARTESIAN_POINT('Ctrl Pts',(13.1228431405579,-13.5191927531554,15.));
#32437=CARTESIAN_POINT('Ctrl Pts',(13.1572182238498,-13.5511230466604,15.));
#32438=CARTESIAN_POINT('Ctrl Pts',(13.2050958591127,-13.5913916488449,15.));
#32439=CARTESIAN_POINT('Ctrl Pts',(13.267724591625,-13.6386021757691,15.));
#32440=CARTESIAN_POINT('Ctrl Pts',(13.332345249068,-13.6835899659728,15.));
#32441=CARTESIAN_POINT('Ctrl Pts',(13.3981837093918,-13.7272351052346,15.));
#32442=CARTESIAN_POINT('Ctrl Pts',(13.4646849459541,-13.7701598398937,15.));
#32443=CARTESIAN_POINT('Ctrl Pts',(13.5316488646659,-13.8125718693898,15.));
#32444=CARTESIAN_POINT('Ctrl Pts',(13.5991011046042,-13.854416158639,15.));
#32445=CARTESIAN_POINT('Ctrl Pts',(13.6672004242289,-13.8954842290745,15.));
#32446=CARTESIAN_POINT('Ctrl Pts',(13.7361389175879,-13.9355316323567,15.));
#32447=CARTESIAN_POINT('Ctrl Pts',(13.806028835706,-13.9744114225699,15.));
#32448=CARTESIAN_POINT('Ctrl Pts',(13.876852657608,-14.0121326766855,15.));
#32449=CARTESIAN_POINT('Ctrl Pts',(13.9485205009332,-14.0487919508068,15.));
#32450=CARTESIAN_POINT('Ctrl Pts',(14.0209038736616,-14.0845327205726,15.));
#32451=CARTESIAN_POINT('Ctrl Pts',(14.0938755647891,-14.1194976094444,15.));
#32452=CARTESIAN_POINT('Ctrl Pts',(14.1673550455622,-14.1537739659715,15.));
#32453=CARTESIAN_POINT('Ctrl Pts',(14.2413181097468,-14.1873822640681,15.));
#32454=CARTESIAN_POINT('Ctrl Pts',(14.3157729256101,-14.2203046917613,15.));
#32455=CARTESIAN_POINT('Ctrl Pts',(14.3907450096103,-14.2525030666863,15.));
#32456=CARTESIAN_POINT('Ctrl Pts',(14.4662599802681,-14.2839394106401,15.));
#32457=CARTESIAN_POINT('Ctrl Pts',(14.5423237181615,-14.3145996213697,15.));
#32458=CARTESIAN_POINT('Ctrl Pts',(14.6189211183837,-14.3444949335274,15.));
#32459=CARTESIAN_POINT('Ctrl Pts',(14.6960255561799,-14.3736505809735,15.));
#32460=CARTESIAN_POINT('Ctrl Pts',(14.7736052248294,-14.4020981965564,15.));
#32461=CARTESIAN_POINT('Ctrl Pts',(14.8516302160049,-14.4298673266313,15.));
#32462=CARTESIAN_POINT('Ctrl Pts',(14.9300806580357,-14.4569756801697,15.));
#32463=CARTESIAN_POINT('Ctrl Pts',(15.0089462280504,-14.4834296977405,15.));
#32464=CARTESIAN_POINT('Ctrl Pts',(15.0882222764759,-14.5092291736391,15.));
#32465=CARTESIAN_POINT('Ctrl Pts',(15.1679069808052,-14.5343706477051,15.));
#32466=CARTESIAN_POINT('Ctrl Pts',(15.2479982823383,-14.5588510579962,15.));
#32467=CARTESIAN_POINT('Ctrl Pts',(15.3284903715086,-14.5826719336929,15.));
#32468=CARTESIAN_POINT('Ctrl Pts',(15.4093740621547,-14.6058389416146,15.));
#32469=CARTESIAN_POINT('Ctrl Pts',(15.4906383406647,-14.6283600295736,15.));
#32470=CARTESIAN_POINT('Ctrl Pts',(15.5722715494357,-14.6502440080912,15.));
#32471=CARTESIAN_POINT('Ctrl Pts',(15.6542626345121,-14.6714990558793,15.));
#32472=CARTESIAN_POINT('Ctrl Pts',(15.7366025822956,-14.692131002056,15.));
#32473=CARTESIAN_POINT('Ctrl Pts',(15.8192842036838,-14.7121435744495,15.));
#32474=CARTESIAN_POINT('Ctrl Pts',(15.9023014613802,-14.7315391924939,15.));
#32475=CARTESIAN_POINT('Ctrl Pts',(15.9856489347991,-14.7503195973741,15.));
#32476=CARTESIAN_POINT('Ctrl Pts',(16.0693212651732,-14.7684865075326,15.));
#32477=CARTESIAN_POINT('Ctrl Pts',(16.1533125058853,-14.7860423865308,15.));
#32478=CARTESIAN_POINT('Ctrl Pts',(16.2376161919272,-14.8029903659562,15.));
#32479=CARTESIAN_POINT('Ctrl Pts',(16.3222256264574,-14.8193339134125,15.));
#32480=CARTESIAN_POINT('Ctrl Pts',(16.4071341001481,-14.8350765822692,15.));
#32481=CARTESIAN_POINT('Ctrl Pts',(16.492335117066,-14.8502217520165,15.));
#32482=CARTESIAN_POINT('Ctrl Pts',(16.5778226646614,-14.8647723257055,15.));
#32483=CARTESIAN_POINT('Ctrl Pts',(16.6635911790385,-14.8787307479454,15.));
#32484=CARTESIAN_POINT('Ctrl Pts',(16.7496353900706,-14.8920991518626,15.));
#32485=CARTESIAN_POINT('Ctrl Pts',(16.8359501981915,-14.9048794721647,15.));
#32486=CARTESIAN_POINT('Ctrl Pts',(16.9225305499155,-14.9170735658747,15.));
#32487=CARTESIAN_POINT('Ctrl Pts',(17.0093712776822,-14.9286833603319,15.));
#32488=CARTESIAN_POINT('Ctrl Pts',(17.0964671184813,-14.9397108660998,15.));
#32489=CARTESIAN_POINT('Ctrl Pts',(17.1838128327073,-14.9501581118289,15.));
#32490=CARTESIAN_POINT('Ctrl Pts',(17.2714032968314,-14.9600271060471,15.));
#32491=CARTESIAN_POINT('Ctrl Pts',(17.3592335908102,-14.9693197947387,15.));
#32492=CARTESIAN_POINT('Ctrl Pts',(17.4472991215239,-14.9780380183576,15.));
#32493=CARTESIAN_POINT('Ctrl Pts',(17.5355955872257,-14.9861834999847,15.));
#32494=CARTESIAN_POINT('Ctrl Pts',(17.6241187988652,-14.9937578646616,15.));
#32495=CARTESIAN_POINT('Ctrl Pts',(17.7128645299878,-15.0007626541287,15.));
#32496=CARTESIAN_POINT('Ctrl Pts',(17.8018283748074,-15.0071993464636,15.));
#32497=CARTESIAN_POINT('Ctrl Pts',(17.891005548971,-15.0130693803259,15.));
#32498=CARTESIAN_POINT('Ctrl Pts',(17.980390892286,-15.0183741723687,15.));
#32499=CARTESIAN_POINT('Ctrl Pts',(18.0699792164192,-15.0231151183906,15.));
#32500=CARTESIAN_POINT('Ctrl Pts',(18.1597655779328,-15.0272936035154,15.));
#32501=CARTESIAN_POINT('Ctrl Pts',(18.2497455679917,-15.0309110092482,15.));
#32502=CARTESIAN_POINT('Ctrl Pts',(18.3399156227477,-15.0339687345357,15.));
#32503=CARTESIAN_POINT('Ctrl Pts',(18.4483447600233,-15.036968080037,15.));
#32504=CARTESIAN_POINT('Ctrl Pts',(18.5389347492702,-15.038771310026,15.));
#32505=CARTESIAN_POINT('Ctrl Pts',(18.6115544313469,-15.0397694451467,15.));
#32506=CARTESIAN_POINT('Ctrl Pts',(18.6661021851765,-15.0402682932586,15.));
#32507=CARTESIAN_POINT('Ctrl Pts',(18.7025042402277,-15.0404898571911,15.));
#32508=CARTESIAN_POINT('Ctrl Pts',(8.52496423935284,-22.4349054983023,0.));
#32509=CARTESIAN_POINT('Ctrl Pts',(8.52496423935284,-22.4349054983023,18.));
#32510=CARTESIAN_POINT('Ctrl Pts',(8.53048330625154,-22.4175610589877,0.));
#32511=CARTESIAN_POINT('Ctrl Pts',(8.53048330625154,-22.4175610589877,18.));
#32512=CARTESIAN_POINT('Ctrl Pts',(8.54146295656906,-22.3828725698612,0.));
#32513=CARTESIAN_POINT('Ctrl Pts',(8.54146295656906,-22.3828725698612,18.));
#32514=CARTESIAN_POINT('Ctrl Pts',(8.55775698160721,-22.3308410047044,0.));
#32515=CARTESIAN_POINT('Ctrl Pts',(8.55775698160721,-22.3308410047044,18.));
#32516=CARTESIAN_POINT('Ctrl Pts',(8.57913133085326,-22.2614679221214,0.));
#32517=CARTESIAN_POINT('Ctrl Pts',(8.57913133085326,-22.2614679221214,18.));
#32518=CARTESIAN_POINT('Ctrl Pts',(8.60526341207613,-22.1747556651024,0.));
#32519=CARTESIAN_POINT('Ctrl Pts',(8.60526341207613,-22.1747556651024,18.));
#32520=CARTESIAN_POINT('Ctrl Pts',(8.63080832792612,-22.0880480931906,0.));
#32521=CARTESIAN_POINT('Ctrl Pts',(8.63080832792612,-22.0880480931906,18.));
#32522=CARTESIAN_POINT('Ctrl Pts',(8.6557643376698,-22.0013463859623,0.));
#32523=CARTESIAN_POINT('Ctrl Pts',(8.6557643376698,-22.0013463859623,18.));
#32524=CARTESIAN_POINT('Ctrl Pts',(8.68012932645739,-21.9146524902336,0.));
#32525=CARTESIAN_POINT('Ctrl Pts',(8.68012932645739,-21.9146524902336,18.));
#32526=CARTESIAN_POINT('Ctrl Pts',(8.70390086252202,-21.8279693631274,0.));
#32527=CARTESIAN_POINT('Ctrl Pts',(8.70390086252202,-21.8279693631274,18.));
#32528=CARTESIAN_POINT('Ctrl Pts',(8.72707626956921,-21.7413007707864,0.));
#32529=CARTESIAN_POINT('Ctrl Pts',(8.72707626956921,-21.7413007707864,18.));
#32530=CARTESIAN_POINT('Ctrl Pts',(8.74965270266163,-21.6546509866725,0.));
#32531=CARTESIAN_POINT('Ctrl Pts',(8.74965270266163,-21.6546509866725,18.));
#32532=CARTESIAN_POINT('Ctrl Pts',(8.77162723103298,-21.5680245138584,0.));
#32533=CARTESIAN_POINT('Ctrl Pts',(8.77162723103298,-21.5680245138584,18.));
#32534=CARTESIAN_POINT('Ctrl Pts',(8.79299691277858,-21.481425822209,0.));
#32535=CARTESIAN_POINT('Ctrl Pts',(8.79299691277858,-21.481425822209,18.));
#32536=CARTESIAN_POINT('Ctrl Pts',(8.81375890120581,-21.3948590173441,0.));
#32537=CARTESIAN_POINT('Ctrl Pts',(8.81375890120581,-21.3948590173441,18.));
#32538=CARTESIAN_POINT('Ctrl Pts',(8.83391042911628,-21.3083278326642,0.));
#32539=CARTESIAN_POINT('Ctrl Pts',(8.83391042911628,-21.3083278326642,18.));
#32540=CARTESIAN_POINT('Ctrl Pts',(8.85344872418155,-21.2218358113425,0.));
#32541=CARTESIAN_POINT('Ctrl Pts',(8.85344872418155,-21.2218358113425,18.));
#32542=CARTESIAN_POINT('Ctrl Pts',(8.87237094640748,-21.1353864352374,0.));
#32543=CARTESIAN_POINT('Ctrl Pts',(8.87237094640748,-21.1353864352374,18.));
#32544=CARTESIAN_POINT('Ctrl Pts',(8.89067412773385,-21.0489832630915,0.));
#32545=CARTESIAN_POINT('Ctrl Pts',(8.89067412773385,-21.0489832630915,18.));
#32546=CARTESIAN_POINT('Ctrl Pts',(8.90835509843284,-20.9626300944902,0.));
#32547=CARTESIAN_POINT('Ctrl Pts',(8.90835509843284,-20.9626300944902,18.));
#32548=CARTESIAN_POINT('Ctrl Pts',(8.92541048738648,-20.8763310073304,0.));
#32549=CARTESIAN_POINT('Ctrl Pts',(8.92541048738648,-20.8763310073304,18.));
#32550=CARTESIAN_POINT('Ctrl Pts',(8.94183680111377,-20.7900902537083,0.));
#32551=CARTESIAN_POINT('Ctrl Pts',(8.94183680111377,-20.7900902537083,18.));
#32552=CARTESIAN_POINT('Ctrl Pts',(8.95763049112623,-20.7039121898975,0.));
#32553=CARTESIAN_POINT('Ctrl Pts',(8.95763049112623,-20.7039121898975,18.));
#32554=CARTESIAN_POINT('Ctrl Pts',(8.97278801890467,-20.6178012000199,0.));
#32555=CARTESIAN_POINT('Ctrl Pts',(8.97278801890467,-20.6178012000199,18.));
#32556=CARTESIAN_POINT('Ctrl Pts',(8.98730595457659,-20.5317616031369,0.));
#32557=CARTESIAN_POINT('Ctrl Pts',(8.98730595457659,-20.5317616031369,18.));
#32558=CARTESIAN_POINT('Ctrl Pts',(9.00118097039516,-20.4457976315472,0.));
#32559=CARTESIAN_POINT('Ctrl Pts',(9.00118097039516,-20.4457976315472,18.));
#32560=CARTESIAN_POINT('Ctrl Pts',(9.01440965049155,-20.3599135373691,0.));
#32561=CARTESIAN_POINT('Ctrl Pts',(9.01440965049155,-20.3599135373691,18.));
#32562=CARTESIAN_POINT('Ctrl Pts',(9.02698833758324,-20.2741136736186,0.));
#32563=CARTESIAN_POINT('Ctrl Pts',(9.02698833758324,-20.2741136736186,18.));
#32564=CARTESIAN_POINT('Ctrl Pts',(9.03891298737031,-20.1884025764493,0.));
#32565=CARTESIAN_POINT('Ctrl Pts',(9.03891298737031,-20.1884025764493,18.));
#32566=CARTESIAN_POINT('Ctrl Pts',(9.0501789809071,-20.1027850670435,0.));
#32567=CARTESIAN_POINT('Ctrl Pts',(9.0501789809071,-20.1027850670435,18.));
#32568=CARTESIAN_POINT('Ctrl Pts',(9.0607810967537,-20.0172662790811,0.));
#32569=CARTESIAN_POINT('Ctrl Pts',(9.0607810967537,-20.0172662790811,18.));
#32570=CARTESIAN_POINT('Ctrl Pts',(9.0707138821585,-19.9318514954605,0.));
#32571=CARTESIAN_POINT('Ctrl Pts',(9.0707138821585,-19.9318514954605,18.));
#32572=CARTESIAN_POINT('Ctrl Pts',(9.07997196979668,-19.846546013708,0.));
#32573=CARTESIAN_POINT('Ctrl Pts',(9.07997196979668,-19.846546013708,18.));
#32574=CARTESIAN_POINT('Ctrl Pts',(9.08855038355401,-19.7613550146978,0.));
#32575=CARTESIAN_POINT('Ctrl Pts',(9.08855038355401,-19.7613550146978,18.));
#32576=CARTESIAN_POINT('Ctrl Pts',(9.0964449428387,-19.6762833927168,0.));
#32577=CARTESIAN_POINT('Ctrl Pts',(9.0964449428387,-19.6762833927168,18.));
#32578=CARTESIAN_POINT('Ctrl Pts',(9.10365235736464,-19.5913357132276,0.));
#32579=CARTESIAN_POINT('Ctrl Pts',(9.10365235736464,-19.5913357132276,18.));
#32580=CARTESIAN_POINT('Ctrl Pts',(9.11016929611335,-19.5065165934577,0.));
#32581=CARTESIAN_POINT('Ctrl Pts',(9.11016929611335,-19.5065165934577,18.));
#32582=CARTESIAN_POINT('Ctrl Pts',(9.11599159243919,-19.4218310275711,0.));
#32583=CARTESIAN_POINT('Ctrl Pts',(9.11599159243919,-19.4218310275711,18.));
#32584=CARTESIAN_POINT('Ctrl Pts',(9.12111347941199,-19.3372847008483,0.));
#32585=CARTESIAN_POINT('Ctrl Pts',(9.12111347941199,-19.3372847008483,18.));
#32586=CARTESIAN_POINT('Ctrl Pts',(9.12552662785599,-19.2528843844341,0.));
#32587=CARTESIAN_POINT('Ctrl Pts',(9.12552662785599,-19.2528843844341,18.));
#32588=CARTESIAN_POINT('Ctrl Pts',(9.12921984349375,-19.1686380639041,0.));
#32589=CARTESIAN_POINT('Ctrl Pts',(9.12921984349375,-19.1686380639041,18.));
#32590=CARTESIAN_POINT('Ctrl Pts',(9.13218114462419,-19.0845541036965,0.));
#32591=CARTESIAN_POINT('Ctrl Pts',(9.13218114462419,-19.0845541036965,18.));
#32592=CARTESIAN_POINT('Ctrl Pts',(9.13439956903532,-19.0006405223697,0.));
#32593=CARTESIAN_POINT('Ctrl Pts',(9.13439956903532,-19.0006405223697,18.));
#32594=CARTESIAN_POINT('Ctrl Pts',(9.13586688858168,-18.9169043053388,0.));
#32595=CARTESIAN_POINT('Ctrl Pts',(9.13586688858168,-18.9169043053388,18.));
#32596=CARTESIAN_POINT('Ctrl Pts',(9.13657985367153,-18.8333505052874,0.));
#32597=CARTESIAN_POINT('Ctrl Pts',(9.13657985367153,-18.8333505052874,18.));
#32598=CARTESIAN_POINT('Ctrl Pts',(9.13654074021147,-18.7499820263476,0.));
#32599=CARTESIAN_POINT('Ctrl Pts',(9.13654074021147,-18.7499820263476,18.));
#32600=CARTESIAN_POINT('Ctrl Pts',(9.13575227582418,-18.6668016710749,0.));
#32601=CARTESIAN_POINT('Ctrl Pts',(9.13575227582418,-18.6668016710749,18.));
#32602=CARTESIAN_POINT('Ctrl Pts',(9.13421321934922,-18.5838139250423,0.));
#32603=CARTESIAN_POINT('Ctrl Pts',(9.13421321934922,-18.5838139250423,18.));
#32604=CARTESIAN_POINT('Ctrl Pts',(9.13191425549883,-18.5010266156389,0.));
#32605=CARTESIAN_POINT('Ctrl Pts',(9.13191425549883,-18.5010266156389,18.));
#32606=CARTESIAN_POINT('Ctrl Pts',(9.12883240135631,-18.4184531695731,0.));
#32607=CARTESIAN_POINT('Ctrl Pts',(9.12883240135631,-18.4184531695731,18.));
#32608=CARTESIAN_POINT('Ctrl Pts',(9.12493031448671,-18.3361129010289,0.));
#32609=CARTESIAN_POINT('Ctrl Pts',(9.12493031448671,-18.3361129010289,18.));
#32610=CARTESIAN_POINT('Ctrl Pts',(9.12016808144599,-18.2540262849075,0.));
#32611=CARTESIAN_POINT('Ctrl Pts',(9.12016808144599,-18.2540262849075,18.));
#32612=CARTESIAN_POINT('Ctrl Pts',(9.11451347590539,-18.1722108451637,0.));
#32613=CARTESIAN_POINT('Ctrl Pts',(9.11451347590539,-18.1722108451637,18.));
#32614=CARTESIAN_POINT('Ctrl Pts',(9.10795114540259,-18.0906774757189,0.));
#32615=CARTESIAN_POINT('Ctrl Pts',(9.10795114540259,-18.0906774757189,18.));
#32616=CARTESIAN_POINT('Ctrl Pts',(9.10049631917583,-18.0094249416472,0.));
#32617=CARTESIAN_POINT('Ctrl Pts',(9.10049631917583,-18.0094249416472,18.));
#32618=CARTESIAN_POINT('Ctrl Pts',(9.09219303320079,-17.9284406141976,0.));
#32619=CARTESIAN_POINT('Ctrl Pts',(9.09219303320079,-17.9284406141976,18.));
#32620=CARTESIAN_POINT('Ctrl Pts',(9.08308548608349,-17.8477120247758,0.));
#32621=CARTESIAN_POINT('Ctrl Pts',(9.08308548608349,-17.8477120247758,18.));
#32622=CARTESIAN_POINT('Ctrl Pts',(9.07319314215026,-17.7672369091005,0.));
#32623=CARTESIAN_POINT('Ctrl Pts',(9.07319314215026,-17.7672369091005,18.));
#32624=CARTESIAN_POINT('Ctrl Pts',(9.06248904941394,-17.6870319618808,0.));
#32625=CARTESIAN_POINT('Ctrl Pts',(9.06248904941394,-17.6870319618808,18.));
#32626=CARTESIAN_POINT('Ctrl Pts',(9.05086524971401,-17.6071467783263,0.));
#32627=CARTESIAN_POINT('Ctrl Pts',(9.05086524971401,-17.6071467783263,18.));
#32628=CARTESIAN_POINT('Ctrl Pts',(9.03814678971601,-17.5276582702181,0.));
#32629=CARTESIAN_POINT('Ctrl Pts',(9.03814678971601,-17.5276582702181,18.));
#32630=CARTESIAN_POINT('Ctrl Pts',(9.0241575097608,-17.4486443043185,0.));
#32631=CARTESIAN_POINT('Ctrl Pts',(9.0241575097608,-17.4486443043185,18.));
#32632=CARTESIAN_POINT('Ctrl Pts',(9.00877780436036,-17.3701605263553,0.));
#32633=CARTESIAN_POINT('Ctrl Pts',(9.00877780436036,-17.3701605263553,18.));
#32634=CARTESIAN_POINT('Ctrl Pts',(8.99199362652256,-17.2922207948279,0.));
#32635=CARTESIAN_POINT('Ctrl Pts',(8.99199362652256,-17.2922207948279,18.));
#32636=CARTESIAN_POINT('Ctrl Pts',(8.97397941759265,-17.2147637614528,0.));
#32637=CARTESIAN_POINT('Ctrl Pts',(8.97397941759265,-17.2147637614528,18.));
#32638=CARTESIAN_POINT('Ctrl Pts',(8.95502702208203,-17.1376822726252,0.));
#32639=CARTESIAN_POINT('Ctrl Pts',(8.95502702208203,-17.1376822726252,18.));
#32640=CARTESIAN_POINT('Ctrl Pts',(8.93538377395243,-17.0608897634975,0.));
#32641=CARTESIAN_POINT('Ctrl Pts',(8.93538377395243,-17.0608897634975,18.));
#32642=CARTESIAN_POINT('Ctrl Pts',(8.91510993758932,-16.9843788566346,0.));
#32643=CARTESIAN_POINT('Ctrl Pts',(8.91510993758932,-16.9843788566346,18.));
#32644=CARTESIAN_POINT('Ctrl Pts',(8.89394614661328,-16.908275670167,0.));
#32645=CARTESIAN_POINT('Ctrl Pts',(8.89394614661328,-16.908275670167,18.));
#32646=CARTESIAN_POINT('Ctrl Pts',(8.87112909692392,-16.8329157811062,0.));
#32647=CARTESIAN_POINT('Ctrl Pts',(8.87112909692392,-16.8329157811062,18.));
#32648=CARTESIAN_POINT('Ctrl Pts',(8.84558256033742,-16.7587634618101,0.));
#32649=CARTESIAN_POINT('Ctrl Pts',(8.84558256033742,-16.7587634618101,18.));
#32650=CARTESIAN_POINT('Ctrl Pts',(8.82207984677446,-16.7007854423938,0.));
#32651=CARTESIAN_POINT('Ctrl Pts',(8.82207984677446,-16.7007854423938,18.));
#32652=CARTESIAN_POINT('Ctrl Pts',(8.8023348179895,-16.6582257921024,0.));
#32653=CARTESIAN_POINT('Ctrl Pts',(8.8023348179895,-16.6582257921024,18.));
#32654=CARTESIAN_POINT('Ctrl Pts',(8.78817964150685,-16.6302847808193,0.));
#32655=CARTESIAN_POINT('Ctrl Pts',(8.78817964150685,-16.6302847808193,18.));
#32656=CARTESIAN_POINT('Ctrl Pts',(8.78085409196639,-16.6164222996225,0.));
#32657=CARTESIAN_POINT('Ctrl Pts',(8.78085409196639,-16.6164222996225,18.));
#32658=CARTESIAN_POINT('',(8.52496423935279,-22.4349054983023,0.));
#32659=CARTESIAN_POINT('Ctrl Pts',(8.78085409196639,-16.6164222996225,0.));
#32660=CARTESIAN_POINT('Ctrl Pts',(8.78817964150685,-16.6302847808193,0.));
#32661=CARTESIAN_POINT('Ctrl Pts',(8.8023348179895,-16.6582257921024,0.));
#32662=CARTESIAN_POINT('Ctrl Pts',(8.82207984677446,-16.7007854423938,0.));
#32663=CARTESIAN_POINT('Ctrl Pts',(8.84558256033742,-16.7587634618101,0.));
#32664=CARTESIAN_POINT('Ctrl Pts',(8.87112909692392,-16.8329157811062,0.));
#32665=CARTESIAN_POINT('Ctrl Pts',(8.89394614661328,-16.908275670167,0.));
#32666=CARTESIAN_POINT('Ctrl Pts',(8.91510993758932,-16.9843788566346,0.));
#32667=CARTESIAN_POINT('Ctrl Pts',(8.93538377395243,-17.0608897634975,0.));
#32668=CARTESIAN_POINT('Ctrl Pts',(8.95502702208203,-17.1376822726252,0.));
#32669=CARTESIAN_POINT('Ctrl Pts',(8.97397941759265,-17.2147637614528,0.));
#32670=CARTESIAN_POINT('Ctrl Pts',(8.99199362652256,-17.2922207948279,0.));
#32671=CARTESIAN_POINT('Ctrl Pts',(9.00877780436036,-17.3701605263553,0.));
#32672=CARTESIAN_POINT('Ctrl Pts',(9.0241575097608,-17.4486443043185,0.));
#32673=CARTESIAN_POINT('Ctrl Pts',(9.03814678971601,-17.5276582702181,0.));
#32674=CARTESIAN_POINT('Ctrl Pts',(9.05086524971401,-17.6071467783263,0.));
#32675=CARTESIAN_POINT('Ctrl Pts',(9.06248904941394,-17.6870319618808,0.));
#32676=CARTESIAN_POINT('Ctrl Pts',(9.07319314215026,-17.7672369091005,0.));
#32677=CARTESIAN_POINT('Ctrl Pts',(9.08308548608349,-17.8477120247758,0.));
#32678=CARTESIAN_POINT('Ctrl Pts',(9.09219303320079,-17.9284406141976,0.));
#32679=CARTESIAN_POINT('Ctrl Pts',(9.10049631917583,-18.0094249416472,0.));
#32680=CARTESIAN_POINT('Ctrl Pts',(9.10795114540259,-18.0906774757189,0.));
#32681=CARTESIAN_POINT('Ctrl Pts',(9.11451347590539,-18.1722108451637,0.));
#32682=CARTESIAN_POINT('Ctrl Pts',(9.12016808144599,-18.2540262849075,0.));
#32683=CARTESIAN_POINT('Ctrl Pts',(9.12493031448671,-18.3361129010289,0.));
#32684=CARTESIAN_POINT('Ctrl Pts',(9.12883240135631,-18.4184531695731,0.));
#32685=CARTESIAN_POINT('Ctrl Pts',(9.13191425549883,-18.5010266156389,0.));
#32686=CARTESIAN_POINT('Ctrl Pts',(9.13421321934922,-18.5838139250423,0.));
#32687=CARTESIAN_POINT('Ctrl Pts',(9.13575227582418,-18.6668016710749,0.));
#32688=CARTESIAN_POINT('Ctrl Pts',(9.13654074021147,-18.7499820263476,0.));
#32689=CARTESIAN_POINT('Ctrl Pts',(9.13657985367153,-18.8333505052874,0.));
#32690=CARTESIAN_POINT('Ctrl Pts',(9.13586688858168,-18.9169043053388,0.));
#32691=CARTESIAN_POINT('Ctrl Pts',(9.13439956903532,-19.0006405223697,0.));
#32692=CARTESIAN_POINT('Ctrl Pts',(9.13218114462419,-19.0845541036965,0.));
#32693=CARTESIAN_POINT('Ctrl Pts',(9.12921984349375,-19.1686380639041,0.));
#32694=CARTESIAN_POINT('Ctrl Pts',(9.12552662785599,-19.2528843844341,0.));
#32695=CARTESIAN_POINT('Ctrl Pts',(9.12111347941199,-19.3372847008483,0.));
#32696=CARTESIAN_POINT('Ctrl Pts',(9.11599159243919,-19.4218310275711,0.));
#32697=CARTESIAN_POINT('Ctrl Pts',(9.11016929611335,-19.5065165934577,0.));
#32698=CARTESIAN_POINT('Ctrl Pts',(9.10365235736464,-19.5913357132276,0.));
#32699=CARTESIAN_POINT('Ctrl Pts',(9.0964449428387,-19.6762833927168,0.));
#32700=CARTESIAN_POINT('Ctrl Pts',(9.08855038355401,-19.7613550146978,0.));
#32701=CARTESIAN_POINT('Ctrl Pts',(9.07997196979668,-19.846546013708,0.));
#32702=CARTESIAN_POINT('Ctrl Pts',(9.0707138821585,-19.9318514954605,0.));
#32703=CARTESIAN_POINT('Ctrl Pts',(9.0607810967537,-20.0172662790811,0.));
#32704=CARTESIAN_POINT('Ctrl Pts',(9.0501789809071,-20.1027850670435,0.));
#32705=CARTESIAN_POINT('Ctrl Pts',(9.03891298737031,-20.1884025764493,0.));
#32706=CARTESIAN_POINT('Ctrl Pts',(9.02698833758324,-20.2741136736186,0.));
#32707=CARTESIAN_POINT('Ctrl Pts',(9.01440965049155,-20.3599135373691,0.));
#32708=CARTESIAN_POINT('Ctrl Pts',(9.00118097039516,-20.4457976315472,0.));
#32709=CARTESIAN_POINT('Ctrl Pts',(8.98730595457659,-20.5317616031369,0.));
#32710=CARTESIAN_POINT('Ctrl Pts',(8.97278801890467,-20.6178012000199,0.));
#32711=CARTESIAN_POINT('Ctrl Pts',(8.95763049112623,-20.7039121898975,0.));
#32712=CARTESIAN_POINT('Ctrl Pts',(8.94183680111377,-20.7900902537083,0.));
#32713=CARTESIAN_POINT('Ctrl Pts',(8.92541048738648,-20.8763310073304,0.));
#32714=CARTESIAN_POINT('Ctrl Pts',(8.90835509843284,-20.9626300944902,0.));
#32715=CARTESIAN_POINT('Ctrl Pts',(8.89067412773385,-21.0489832630915,0.));
#32716=CARTESIAN_POINT('Ctrl Pts',(8.87237094640748,-21.1353864352374,0.));
#32717=CARTESIAN_POINT('Ctrl Pts',(8.85344872418155,-21.2218358113425,0.));
#32718=CARTESIAN_POINT('Ctrl Pts',(8.83391042911628,-21.3083278326642,0.));
#32719=CARTESIAN_POINT('Ctrl Pts',(8.81375890120581,-21.3948590173441,0.));
#32720=CARTESIAN_POINT('Ctrl Pts',(8.79299691277858,-21.481425822209,0.));
#32721=CARTESIAN_POINT('Ctrl Pts',(8.77162723103298,-21.5680245138584,0.));
#32722=CARTESIAN_POINT('Ctrl Pts',(8.74965270266163,-21.6546509866725,0.));
#32723=CARTESIAN_POINT('Ctrl Pts',(8.72707626956921,-21.7413007707864,0.));
#32724=CARTESIAN_POINT('Ctrl Pts',(8.70390086252202,-21.8279693631274,0.));
#32725=CARTESIAN_POINT('Ctrl Pts',(8.68012932645739,-21.9146524902336,0.));
#32726=CARTESIAN_POINT('Ctrl Pts',(8.6557643376698,-22.0013463859623,0.));
#32727=CARTESIAN_POINT('Ctrl Pts',(8.63080832792612,-22.0880480931906,0.));
#32728=CARTESIAN_POINT('Ctrl Pts',(8.60015442890613,-22.1920971794848,0.));
#32729=CARTESIAN_POINT('Ctrl Pts',(8.57387555634004,-22.2788106077806,0.));
#32730=CARTESIAN_POINT('Ctrl Pts',(8.55238412336293,-22.3481844703457,0.));
#32731=CARTESIAN_POINT('Ctrl Pts',(8.53600237317212,-22.400216619619,0.));
#32732=CARTESIAN_POINT('Ctrl Pts',(8.52496423935284,-22.4349054983023,0.));
#32733=CARTESIAN_POINT('',(8.52496423935279,-22.4349054983023,15.));
#32734=CARTESIAN_POINT('Ctrl Pts',(8.52496423935284,-22.4349054983023,15.));
#32735=CARTESIAN_POINT('Ctrl Pts',(8.53048330625154,-22.4175610589877,15.));
#32736=CARTESIAN_POINT('Ctrl Pts',(8.54146295656906,-22.3828725698612,15.));
#32737=CARTESIAN_POINT('Ctrl Pts',(8.55775698160721,-22.3308410047044,15.));
#32738=CARTESIAN_POINT('Ctrl Pts',(8.57913133085326,-22.2614679221214,15.));
#32739=CARTESIAN_POINT('Ctrl Pts',(8.60526341207613,-22.1747556651024,15.));
#32740=CARTESIAN_POINT('Ctrl Pts',(8.63080832792612,-22.0880480931906,15.));
#32741=CARTESIAN_POINT('Ctrl Pts',(8.6557643376698,-22.0013463859623,15.));
#32742=CARTESIAN_POINT('Ctrl Pts',(8.68012932645739,-21.9146524902336,15.));
#32743=CARTESIAN_POINT('Ctrl Pts',(8.70390086252202,-21.8279693631274,15.));
#32744=CARTESIAN_POINT('Ctrl Pts',(8.72707626956921,-21.7413007707864,15.));
#32745=CARTESIAN_POINT('Ctrl Pts',(8.74965270266163,-21.6546509866725,15.));
#32746=CARTESIAN_POINT('Ctrl Pts',(8.77162723103298,-21.5680245138584,15.));
#32747=CARTESIAN_POINT('Ctrl Pts',(8.79299691277858,-21.481425822209,15.));
#32748=CARTESIAN_POINT('Ctrl Pts',(8.81375890120581,-21.3948590173441,15.));
#32749=CARTESIAN_POINT('Ctrl Pts',(8.83391042911628,-21.3083278326642,15.));
#32750=CARTESIAN_POINT('Ctrl Pts',(8.85344872418155,-21.2218358113425,15.));
#32751=CARTESIAN_POINT('Ctrl Pts',(8.87237094640748,-21.1353864352374,15.));
#32752=CARTESIAN_POINT('Ctrl Pts',(8.89067412773385,-21.0489832630915,15.));
#32753=CARTESIAN_POINT('Ctrl Pts',(8.90835509843284,-20.9626300944902,15.));
#32754=CARTESIAN_POINT('Ctrl Pts',(8.92541048738648,-20.8763310073304,15.));
#32755=CARTESIAN_POINT('Ctrl Pts',(8.94183680111377,-20.7900902537083,15.));
#32756=CARTESIAN_POINT('Ctrl Pts',(8.95763049112623,-20.7039121898975,15.));
#32757=CARTESIAN_POINT('Ctrl Pts',(8.97278801890467,-20.6178012000199,15.));
#32758=CARTESIAN_POINT('Ctrl Pts',(8.98730595457659,-20.5317616031369,15.));
#32759=CARTESIAN_POINT('Ctrl Pts',(9.00118097039516,-20.4457976315472,15.));
#32760=CARTESIAN_POINT('Ctrl Pts',(9.01440965049155,-20.3599135373691,15.));
#32761=CARTESIAN_POINT('Ctrl Pts',(9.02698833758324,-20.2741136736186,15.));
#32762=CARTESIAN_POINT('Ctrl Pts',(9.03891298737031,-20.1884025764493,15.));
#32763=CARTESIAN_POINT('Ctrl Pts',(9.0501789809071,-20.1027850670435,15.));
#32764=CARTESIAN_POINT('Ctrl Pts',(9.0607810967537,-20.0172662790811,15.));
#32765=CARTESIAN_POINT('Ctrl Pts',(9.0707138821585,-19.9318514954605,15.));
#32766=CARTESIAN_POINT('Ctrl Pts',(9.07997196979668,-19.846546013708,15.));
#32767=CARTESIAN_POINT('Ctrl Pts',(9.08855038355401,-19.7613550146978,15.));
#32768=CARTESIAN_POINT('Ctrl Pts',(9.0964449428387,-19.6762833927168,15.));
#32769=CARTESIAN_POINT('Ctrl Pts',(9.10365235736464,-19.5913357132276,15.));
#32770=CARTESIAN_POINT('Ctrl Pts',(9.11016929611335,-19.5065165934577,15.));
#32771=CARTESIAN_POINT('Ctrl Pts',(9.11599159243919,-19.4218310275711,15.));
#32772=CARTESIAN_POINT('Ctrl Pts',(9.12111347941199,-19.3372847008483,15.));
#32773=CARTESIAN_POINT('Ctrl Pts',(9.12552662785599,-19.2528843844341,15.));
#32774=CARTESIAN_POINT('Ctrl Pts',(9.12921984349375,-19.1686380639041,15.));
#32775=CARTESIAN_POINT('Ctrl Pts',(9.13218114462419,-19.0845541036965,15.));
#32776=CARTESIAN_POINT('Ctrl Pts',(9.13439956903532,-19.0006405223697,15.));
#32777=CARTESIAN_POINT('Ctrl Pts',(9.13586688858168,-18.9169043053388,15.));
#32778=CARTESIAN_POINT('Ctrl Pts',(9.13657985367153,-18.8333505052874,15.));
#32779=CARTESIAN_POINT('Ctrl Pts',(9.13654074021147,-18.7499820263476,15.));
#32780=CARTESIAN_POINT('Ctrl Pts',(9.13575227582418,-18.6668016710749,15.));
#32781=CARTESIAN_POINT('Ctrl Pts',(9.13421321934922,-18.5838139250423,15.));
#32782=CARTESIAN_POINT('Ctrl Pts',(9.13191425549883,-18.5010266156389,15.));
#32783=CARTESIAN_POINT('Ctrl Pts',(9.12883240135631,-18.4184531695731,15.));
#32784=CARTESIAN_POINT('Ctrl Pts',(9.12493031448671,-18.3361129010289,15.));
#32785=CARTESIAN_POINT('Ctrl Pts',(9.12016808144599,-18.2540262849075,15.));
#32786=CARTESIAN_POINT('Ctrl Pts',(9.11451347590539,-18.1722108451637,15.));
#32787=CARTESIAN_POINT('Ctrl Pts',(9.10795114540259,-18.0906774757189,15.));
#32788=CARTESIAN_POINT('Ctrl Pts',(9.10049631917583,-18.0094249416472,15.));
#32789=CARTESIAN_POINT('Ctrl Pts',(9.09219303320079,-17.9284406141976,15.));
#32790=CARTESIAN_POINT('Ctrl Pts',(9.08308548608349,-17.8477120247758,15.));
#32791=CARTESIAN_POINT('Ctrl Pts',(9.07319314215026,-17.7672369091005,15.));
#32792=CARTESIAN_POINT('Ctrl Pts',(9.06248904941394,-17.6870319618808,15.));
#32793=CARTESIAN_POINT('Ctrl Pts',(9.05086524971401,-17.6071467783263,15.));
#32794=CARTESIAN_POINT('Ctrl Pts',(9.03814678971601,-17.5276582702181,15.));
#32795=CARTESIAN_POINT('Ctrl Pts',(9.0241575097608,-17.4486443043185,15.));
#32796=CARTESIAN_POINT('Ctrl Pts',(9.00877780436036,-17.3701605263553,15.));
#32797=CARTESIAN_POINT('Ctrl Pts',(8.99199362652256,-17.2922207948279,15.));
#32798=CARTESIAN_POINT('Ctrl Pts',(8.97397941759265,-17.2147637614528,15.));
#32799=CARTESIAN_POINT('Ctrl Pts',(8.95502702208203,-17.1376822726252,15.));
#32800=CARTESIAN_POINT('Ctrl Pts',(8.93538377395243,-17.0608897634975,15.));
#32801=CARTESIAN_POINT('Ctrl Pts',(8.91510993758932,-16.9843788566346,15.));
#32802=CARTESIAN_POINT('Ctrl Pts',(8.89394614661328,-16.908275670167,15.));
#32803=CARTESIAN_POINT('Ctrl Pts',(8.87112909692392,-16.8329157811062,15.));
#32804=CARTESIAN_POINT('Ctrl Pts',(8.84558256033742,-16.7587634618101,15.));
#32805=CARTESIAN_POINT('Ctrl Pts',(8.82207984677446,-16.7007854423938,15.));
#32806=CARTESIAN_POINT('Ctrl Pts',(8.8023348179895,-16.6582257921024,15.));
#32807=CARTESIAN_POINT('Ctrl Pts',(8.78817964150685,-16.6302847808193,15.));
#32808=CARTESIAN_POINT('Ctrl Pts',(8.78085409196639,-16.6164222996225,15.));
#32809=CARTESIAN_POINT('',(8.52496423935279,-22.4349054983023,0.));
#32810=CARTESIAN_POINT('Origin',(3.56140965415431E-14,-1.09833465940894E-13,
0.));
#32811=CARTESIAN_POINT('',(6.29006564240226,-23.1610680715348,0.));
#32812=CARTESIAN_POINT('Origin',(3.56140965415431E-14,-1.09833465940894E-13,
0.));
#32813=CARTESIAN_POINT('',(6.29006564240226,-23.1610680715348,15.));
#32814=CARTESIAN_POINT('Origin',(3.56140965415431E-14,-1.09833465940894E-13,
15.));
#32815=CARTESIAN_POINT('',(6.29006564240226,-23.1610680715348,0.));
#32816=CARTESIAN_POINT('Ctrl Pts',(2.66302778805429,-18.6042245638953,0.));
#32817=CARTESIAN_POINT('Ctrl Pts',(2.66302778805429,-18.6042245638953,18.));
#32818=CARTESIAN_POINT('Ctrl Pts',(2.66524945599054,-18.6197453967525,0.));
#32819=CARTESIAN_POINT('Ctrl Pts',(2.66524945599054,-18.6197453967525,18.));
#32820=CARTESIAN_POINT('Ctrl Pts',(2.67022099202408,-18.6506703537007,0.));
#32821=CARTESIAN_POINT('Ctrl Pts',(2.67022099202408,-18.6506703537007,18.));
#32822=CARTESIAN_POINT('Ctrl Pts',(2.67926286296661,-18.696707670787,0.));
#32823=CARTESIAN_POINT('Ctrl Pts',(2.67926286296661,-18.696707670787,18.));
#32824=CARTESIAN_POINT('Ctrl Pts',(2.69432739305027,-18.7574274222161,0.));
#32825=CARTESIAN_POINT('Ctrl Pts',(2.69432739305027,-18.7574274222161,18.));
#32826=CARTESIAN_POINT('Ctrl Pts',(2.71724545050994,-18.8324337861517,0.));
#32827=CARTESIAN_POINT('Ctrl Pts',(2.71724545050994,-18.8324337861517,18.));
#32828=CARTESIAN_POINT('Ctrl Pts',(2.74308150095404,-18.9068127424043,0.));
#32829=CARTESIAN_POINT('Ctrl Pts',(2.74308150095404,-18.9068127424043,18.));
#32830=CARTESIAN_POINT('Ctrl Pts',(2.77069196504715,-18.980821277801,0.));
#32831=CARTESIAN_POINT('Ctrl Pts',(2.77069196504715,-18.980821277801,18.));
#32832=CARTESIAN_POINT('Ctrl Pts',(2.79926206958176,-19.0546365637297,0.));
#32833=CARTESIAN_POINT('Ctrl Pts',(2.79926206958176,-19.0546365637297,18.));
#32834=CARTESIAN_POINT('Ctrl Pts',(2.828507852372,-19.1283090202125,0.));
#32835=CARTESIAN_POINT('Ctrl Pts',(2.828507852372,-19.1283090202125,18.));
#32836=CARTESIAN_POINT('Ctrl Pts',(2.85848240467741,-19.2018091932025,0.));
#32837=CARTESIAN_POINT('Ctrl Pts',(2.85848240467741,-19.2018091932025,18.));
#32838=CARTESIAN_POINT('Ctrl Pts',(2.88943670541708,-19.2750617358775,0.));
#32839=CARTESIAN_POINT('Ctrl Pts',(2.88943670541708,-19.2750617358775,18.));
#32840=CARTESIAN_POINT('Ctrl Pts',(2.92166984506915,-19.3479817954251,0.));
#32841=CARTESIAN_POINT('Ctrl Pts',(2.92166984506915,-19.3479817954251,18.));
#32842=CARTESIAN_POINT('Ctrl Pts',(2.95535900926266,-19.420516469599,0.));
#32843=CARTESIAN_POINT('Ctrl Pts',(2.95535900926266,-19.420516469599,18.));
#32844=CARTESIAN_POINT('Ctrl Pts',(2.99048468792079,-19.4926628032527,0.));
#32845=CARTESIAN_POINT('Ctrl Pts',(2.99048468792079,-19.4926628032527,18.));
#32846=CARTESIAN_POINT('Ctrl Pts',(3.02691741043283,-19.5644460803884,0.));
#32847=CARTESIAN_POINT('Ctrl Pts',(3.02691741043283,-19.5644460803884,18.));
#32848=CARTESIAN_POINT('Ctrl Pts',(3.06446889170638,-19.635906849522,0.));
#32849=CARTESIAN_POINT('Ctrl Pts',(3.06446889170638,-19.635906849522,18.));
#32850=CARTESIAN_POINT('Ctrl Pts',(3.10295238390997,-19.7070857227052,0.));
#32851=CARTESIAN_POINT('Ctrl Pts',(3.10295238390997,-19.7070857227052,18.));
#32852=CARTESIAN_POINT('Ctrl Pts',(3.1422513957243,-19.7780060327855,0.));
#32853=CARTESIAN_POINT('Ctrl Pts',(3.1422513957243,-19.7780060327855,18.));
#32854=CARTESIAN_POINT('Ctrl Pts',(3.18233430962982,-19.8486701154397,0.));
#32855=CARTESIAN_POINT('Ctrl Pts',(3.18233430962982,-19.8486701154397,18.));
#32856=CARTESIAN_POINT('Ctrl Pts',(3.22321820350857,-19.9190683616661,0.));
#32857=CARTESIAN_POINT('Ctrl Pts',(3.22321820350857,-19.9190683616661,18.));
#32858=CARTESIAN_POINT('Ctrl Pts',(3.26494616363974,-19.9891848794807,0.));
#32859=CARTESIAN_POINT('Ctrl Pts',(3.26494616363974,-19.9891848794807,18.));
#32860=CARTESIAN_POINT('Ctrl Pts',(3.30756123886962,-20.0590040020604,0.));
#32861=CARTESIAN_POINT('Ctrl Pts',(3.30756123886962,-20.0590040020604,18.));
#32862=CARTESIAN_POINT('Ctrl Pts',(3.351076475782,-20.1285177769596,0.));
#32863=CARTESIAN_POINT('Ctrl Pts',(3.351076475782,-20.1285177769596,18.));
#32864=CARTESIAN_POINT('Ctrl Pts',(3.39547305068767,-20.1977264147619,0.));
#32865=CARTESIAN_POINT('Ctrl Pts',(3.39547305068767,-20.1977264147619,18.));
#32866=CARTESIAN_POINT('Ctrl Pts',(3.44071459161672,-20.2666346804507,0.));
#32867=CARTESIAN_POINT('Ctrl Pts',(3.44071459161672,-20.2666346804507,18.));
#32868=CARTESIAN_POINT('Ctrl Pts',(3.48675677306966,-20.3352494700167,0.));
#32869=CARTESIAN_POINT('Ctrl Pts',(3.48675677306966,-20.3352494700167,18.));
#32870=CARTESIAN_POINT('Ctrl Pts',(3.53355803178954,-20.4035771072894,0.));
#32871=CARTESIAN_POINT('Ctrl Pts',(3.53355803178954,-20.4035771072894,18.));
#32872=CARTESIAN_POINT('Ctrl Pts',(3.58109188218494,-20.4716202388531,0.));
#32873=CARTESIAN_POINT('Ctrl Pts',(3.58109188218494,-20.4716202388531,18.));
#32874=CARTESIAN_POINT('Ctrl Pts',(3.62934618720589,-20.5393780076056,0.));
#32875=CARTESIAN_POINT('Ctrl Pts',(3.62934618720589,-20.5393780076056,18.));
#32876=CARTESIAN_POINT('Ctrl Pts',(3.67831730617887,-20.6068475141781,0.));
#32877=CARTESIAN_POINT('Ctrl Pts',(3.67831730617887,-20.6068475141781,18.));
#32878=CARTESIAN_POINT('Ctrl Pts',(3.72800579849619,-20.6740248879992,0.));
#32879=CARTESIAN_POINT('Ctrl Pts',(3.72800579849619,-20.6740248879992,18.));
#32880=CARTESIAN_POINT('Ctrl Pts',(3.77841179839888,-20.740906441832,0.));
#32881=CARTESIAN_POINT('Ctrl Pts',(3.77841179839888,-20.740906441832,18.));
#32882=CARTESIAN_POINT('Ctrl Pts',(3.82952970701915,-20.8074899980321,0.));
#32883=CARTESIAN_POINT('Ctrl Pts',(3.82952970701915,-20.8074899980321,18.));
#32884=CARTESIAN_POINT('Ctrl Pts',(3.88134876172353,-20.8737747416623,0.));
#32885=CARTESIAN_POINT('Ctrl Pts',(3.88134876172353,-20.8737747416623,18.));
#32886=CARTESIAN_POINT('Ctrl Pts',(3.93385538070582,-20.9397606289993,0.));
#32887=CARTESIAN_POINT('Ctrl Pts',(3.93385538070582,-20.9397606289993,18.));
#32888=CARTESIAN_POINT('Ctrl Pts',(3.98703495407281,-21.0054479357374,0.));
#32889=CARTESIAN_POINT('Ctrl Pts',(3.98703495407281,-21.0054479357374,18.));
#32890=CARTESIAN_POINT('Ctrl Pts',(4.04087373166023,-21.0708367812416,0.));
#32891=CARTESIAN_POINT('Ctrl Pts',(4.04087373166023,-21.0708367812416,18.));
#32892=CARTESIAN_POINT('Ctrl Pts',(4.09536099504429,-21.1359265833073,0.));
#32893=CARTESIAN_POINT('Ctrl Pts',(4.09536099504429,-21.1359265833073,18.));
#32894=CARTESIAN_POINT('Ctrl Pts',(4.15048873695645,-21.2007161321625,0.));
#32895=CARTESIAN_POINT('Ctrl Pts',(4.15048873695645,-21.2007161321625,18.));
#32896=CARTESIAN_POINT('Ctrl Pts',(4.20625065101369,-21.2652038365365,0.));
#32897=CARTESIAN_POINT('Ctrl Pts',(4.20625065101369,-21.2652038365365,18.));
#32898=CARTESIAN_POINT('Ctrl Pts',(4.26264132842711,-21.3293879189372,0.));
#32899=CARTESIAN_POINT('Ctrl Pts',(4.26264132842711,-21.3293879189372,18.));
#32900=CARTESIAN_POINT('Ctrl Pts',(4.31965542378783,-21.3932666198096,0.));
#32901=CARTESIAN_POINT('Ctrl Pts',(4.31965542378783,-21.3932666198096,18.));
#32902=CARTESIAN_POINT('Ctrl Pts',(4.37728667813637,-21.4568384368826,0.));
#32903=CARTESIAN_POINT('Ctrl Pts',(4.37728667813637,-21.4568384368826,18.));
#32904=CARTESIAN_POINT('Ctrl Pts',(4.43552802047029,-21.5201021036274,0.));
#32905=CARTESIAN_POINT('Ctrl Pts',(4.43552802047029,-21.5201021036274,18.));
#32906=CARTESIAN_POINT('Ctrl Pts',(4.49437199472474,-21.5830564890896,0.));
#32907=CARTESIAN_POINT('Ctrl Pts',(4.49437199472474,-21.5830564890896,18.));
#32908=CARTESIAN_POINT('Ctrl Pts',(4.55381108432127,-21.6457005243617,0.));
#32909=CARTESIAN_POINT('Ctrl Pts',(4.55381108432127,-21.6457005243617,18.));
#32910=CARTESIAN_POINT('Ctrl Pts',(4.6138380475249,-21.7080331252945,0.));
#32911=CARTESIAN_POINT('Ctrl Pts',(4.6138380475249,-21.7080331252945,18.));
#32912=CARTESIAN_POINT('Ctrl Pts',(4.67444631371023,-21.770053106418,0.));
#32913=CARTESIAN_POINT('Ctrl Pts',(4.67444631371023,-21.770053106418,18.));
#32914=CARTESIAN_POINT('Ctrl Pts',(4.73562994468575,-21.8317591750867,0.));
#32915=CARTESIAN_POINT('Ctrl Pts',(4.73562994468575,-21.8317591750867,18.));
#32916=CARTESIAN_POINT('Ctrl Pts',(4.7973834230091,-21.8931499593332,0.));
#32917=CARTESIAN_POINT('Ctrl Pts',(4.7973834230091,-21.8931499593332,18.));
#32918=CARTESIAN_POINT('Ctrl Pts',(4.85970148585195,-21.954224026919,0.));
#32919=CARTESIAN_POINT('Ctrl Pts',(4.85970148585195,-21.954224026919,18.));
#32920=CARTESIAN_POINT('Ctrl Pts',(4.92257895332778,-22.0149799098431,0.));
#32921=CARTESIAN_POINT('Ctrl Pts',(4.92257895332778,-22.0149799098431,18.));
#32922=CARTESIAN_POINT('Ctrl Pts',(4.98601051193086,-22.0754161299398,0.));
#32923=CARTESIAN_POINT('Ctrl Pts',(4.98601051193086,-22.0754161299398,18.));
#32924=CARTESIAN_POINT('Ctrl Pts',(5.0499907220168,-22.1355312202693,0.));
#32925=CARTESIAN_POINT('Ctrl Pts',(5.0499907220168,-22.1355312202693,18.));
#32926=CARTESIAN_POINT('Ctrl Pts',(5.11451415224483,-22.1953237422816,0.));
#32927=CARTESIAN_POINT('Ctrl Pts',(5.11451415224483,-22.1953237422816,18.));
#32928=CARTESIAN_POINT('Ctrl Pts',(5.17957547700992,-22.2547923093751,0.));
#32929=CARTESIAN_POINT('Ctrl Pts',(5.17957547700992,-22.2547923093751,18.));
#32930=CARTESIAN_POINT('Ctrl Pts',(5.24516957209272,-22.3139356039553,0.));
#32931=CARTESIAN_POINT('Ctrl Pts',(5.24516957209272,-22.3139356039553,18.));
#32932=CARTESIAN_POINT('Ctrl Pts',(5.31129163978934,-22.3727524152125,0.));
#32933=CARTESIAN_POINT('Ctrl Pts',(5.31129163978934,-22.3727524152125,18.));
#32934=CARTESIAN_POINT('Ctrl Pts',(5.37793718711213,-22.4312416086453,0.));
#32935=CARTESIAN_POINT('Ctrl Pts',(5.37793718711213,-22.4312416086453,18.));
#32936=CARTESIAN_POINT('Ctrl Pts',(5.44510186987254,-22.4894020366778,0.));
#32937=CARTESIAN_POINT('Ctrl Pts',(5.44510186987254,-22.4894020366778,18.));
#32938=CARTESIAN_POINT('Ctrl Pts',(5.51278136258485,-22.5472324623564,0.));
#32939=CARTESIAN_POINT('Ctrl Pts',(5.51278136258485,-22.5472324623564,18.));
#32940=CARTESIAN_POINT('Ctrl Pts',(5.58097123210075,-22.6047314918151,0.));
#32941=CARTESIAN_POINT('Ctrl Pts',(5.58097123210075,-22.6047314918151,18.));
#32942=CARTESIAN_POINT('Ctrl Pts',(5.64966676217478,-22.6618974767817,0.));
#32943=CARTESIAN_POINT('Ctrl Pts',(5.64966676217478,-22.6618974767817,18.));
#32944=CARTESIAN_POINT('Ctrl Pts',(5.71886294543539,-22.7187285302677,0.));
#32945=CARTESIAN_POINT('Ctrl Pts',(5.71886294543539,-22.7187285302677,18.));
#32946=CARTESIAN_POINT('Ctrl Pts',(5.7885547640031,-22.7752227318719,0.));
#32947=CARTESIAN_POINT('Ctrl Pts',(5.7885547640031,-22.7752227318719,18.));
#32948=CARTESIAN_POINT('Ctrl Pts',(5.85873740439746,-22.8313782965033,0.));
#32949=CARTESIAN_POINT('Ctrl Pts',(5.85873740439746,-22.8313782965033,18.));
#32950=CARTESIAN_POINT('Ctrl Pts',(5.92940648776744,-22.8871937503747,0.));
#32951=CARTESIAN_POINT('Ctrl Pts',(5.92940648776744,-22.8871937503747,18.));
#32952=CARTESIAN_POINT('Ctrl Pts',(6.00055830861927,-22.9426681304804,0.));
#32953=CARTESIAN_POINT('Ctrl Pts',(6.00055830861927,-22.9426681304804,18.));
#32954=CARTESIAN_POINT('Ctrl Pts',(6.07219001169362,-22.9978011048904,0.));
#32955=CARTESIAN_POINT('Ctrl Pts',(6.07219001169362,-22.9978011048904,18.));
#32956=CARTESIAN_POINT('Ctrl Pts',(6.14429949537005,-23.0525927424848,0.));
#32957=CARTESIAN_POINT('Ctrl Pts',(6.14429949537005,-23.0525927424848,18.));
#32958=CARTESIAN_POINT('Ctrl Pts',(6.20236818200218,-23.0961532179825,0.));
#32959=CARTESIAN_POINT('Ctrl Pts',(6.20236818200218,-23.0961532179825,18.));
#32960=CARTESIAN_POINT('Ctrl Pts',(6.24613371181766,-23.1286702508203,0.));
#32961=CARTESIAN_POINT('Ctrl Pts',(6.24613371181766,-23.1286702508203,18.));
#32962=CARTESIAN_POINT('Ctrl Pts',(6.27540581784971,-23.1502801515009,0.));
#32963=CARTESIAN_POINT('Ctrl Pts',(6.27540581784971,-23.1502801515009,18.));
#32964=CARTESIAN_POINT('Ctrl Pts',(6.29006564240226,-23.1610680715348,0.));
#32965=CARTESIAN_POINT('Ctrl Pts',(6.29006564240226,-23.1610680715348,18.));
#32966=CARTESIAN_POINT('Ctrl Pts',(2.66302778805429,-18.6042245638953,0.));
#32967=CARTESIAN_POINT('Ctrl Pts',(2.66524945599054,-18.6197453967525,0.));
#32968=CARTESIAN_POINT('Ctrl Pts',(2.67022099202408,-18.6506703537007,0.));
#32969=CARTESIAN_POINT('Ctrl Pts',(2.67926286296661,-18.696707670787,0.));
#32970=CARTESIAN_POINT('Ctrl Pts',(2.69432739305027,-18.7574274222161,0.));
#32971=CARTESIAN_POINT('Ctrl Pts',(2.71724545050994,-18.8324337861517,0.));
#32972=CARTESIAN_POINT('Ctrl Pts',(2.74308150095404,-18.9068127424043,0.));
#32973=CARTESIAN_POINT('Ctrl Pts',(2.77069196504715,-18.980821277801,0.));
#32974=CARTESIAN_POINT('Ctrl Pts',(2.79926206958176,-19.0546365637297,0.));
#32975=CARTESIAN_POINT('Ctrl Pts',(2.828507852372,-19.1283090202125,0.));
#32976=CARTESIAN_POINT('Ctrl Pts',(2.85848240467741,-19.2018091932025,0.));
#32977=CARTESIAN_POINT('Ctrl Pts',(2.88943670541708,-19.2750617358775,0.));
#32978=CARTESIAN_POINT('Ctrl Pts',(2.92166984506915,-19.3479817954251,0.));
#32979=CARTESIAN_POINT('Ctrl Pts',(2.95535900926266,-19.420516469599,0.));
#32980=CARTESIAN_POINT('Ctrl Pts',(2.99048468792079,-19.4926628032527,0.));
#32981=CARTESIAN_POINT('Ctrl Pts',(3.02691741043283,-19.5644460803884,0.));
#32982=CARTESIAN_POINT('Ctrl Pts',(3.06446889170638,-19.635906849522,0.));
#32983=CARTESIAN_POINT('Ctrl Pts',(3.10295238390997,-19.7070857227052,0.));
#32984=CARTESIAN_POINT('Ctrl Pts',(3.1422513957243,-19.7780060327855,0.));
#32985=CARTESIAN_POINT('Ctrl Pts',(3.18233430962982,-19.8486701154397,0.));
#32986=CARTESIAN_POINT('Ctrl Pts',(3.22321820350857,-19.9190683616661,0.));
#32987=CARTESIAN_POINT('Ctrl Pts',(3.26494616363974,-19.9891848794807,0.));
#32988=CARTESIAN_POINT('Ctrl Pts',(3.30756123886962,-20.0590040020604,0.));
#32989=CARTESIAN_POINT('Ctrl Pts',(3.351076475782,-20.1285177769596,0.));
#32990=CARTESIAN_POINT('Ctrl Pts',(3.39547305068767,-20.1977264147619,0.));
#32991=CARTESIAN_POINT('Ctrl Pts',(3.44071459161672,-20.2666346804507,0.));
#32992=CARTESIAN_POINT('Ctrl Pts',(3.48675677306966,-20.3352494700167,0.));
#32993=CARTESIAN_POINT('Ctrl Pts',(3.53355803178954,-20.4035771072894,0.));
#32994=CARTESIAN_POINT('Ctrl Pts',(3.58109188218494,-20.4716202388531,0.));
#32995=CARTESIAN_POINT('Ctrl Pts',(3.62934618720589,-20.5393780076056,0.));
#32996=CARTESIAN_POINT('Ctrl Pts',(3.67831730617887,-20.6068475141781,0.));
#32997=CARTESIAN_POINT('Ctrl Pts',(3.72800579849619,-20.6740248879992,0.));
#32998=CARTESIAN_POINT('Ctrl Pts',(3.77841179839888,-20.740906441832,0.));
#32999=CARTESIAN_POINT('Ctrl Pts',(3.82952970701915,-20.8074899980321,0.));
#33000=CARTESIAN_POINT('Ctrl Pts',(3.88134876172353,-20.8737747416623,0.));
#33001=CARTESIAN_POINT('Ctrl Pts',(3.93385538070582,-20.9397606289993,0.));
#33002=CARTESIAN_POINT('Ctrl Pts',(3.98703495407281,-21.0054479357374,0.));
#33003=CARTESIAN_POINT('Ctrl Pts',(4.04087373166023,-21.0708367812416,0.));
#33004=CARTESIAN_POINT('Ctrl Pts',(4.09536099504429,-21.1359265833073,0.));
#33005=CARTESIAN_POINT('Ctrl Pts',(4.15048873695645,-21.2007161321625,0.));
#33006=CARTESIAN_POINT('Ctrl Pts',(4.20625065101369,-21.2652038365365,0.));
#33007=CARTESIAN_POINT('Ctrl Pts',(4.26264132842711,-21.3293879189372,0.));
#33008=CARTESIAN_POINT('Ctrl Pts',(4.31965542378783,-21.3932666198096,0.));
#33009=CARTESIAN_POINT('Ctrl Pts',(4.37728667813637,-21.4568384368826,0.));
#33010=CARTESIAN_POINT('Ctrl Pts',(4.43552802047029,-21.5201021036274,0.));
#33011=CARTESIAN_POINT('Ctrl Pts',(4.49437199472474,-21.5830564890896,0.));
#33012=CARTESIAN_POINT('Ctrl Pts',(4.55381108432127,-21.6457005243617,0.));
#33013=CARTESIAN_POINT('Ctrl Pts',(4.6138380475249,-21.7080331252945,0.));
#33014=CARTESIAN_POINT('Ctrl Pts',(4.67444631371023,-21.770053106418,0.));
#33015=CARTESIAN_POINT('Ctrl Pts',(4.73562994468575,-21.8317591750867,0.));
#33016=CARTESIAN_POINT('Ctrl Pts',(4.7973834230091,-21.8931499593332,0.));
#33017=CARTESIAN_POINT('Ctrl Pts',(4.85970148585195,-21.954224026919,0.));
#33018=CARTESIAN_POINT('Ctrl Pts',(4.92257895332778,-22.0149799098431,0.));
#33019=CARTESIAN_POINT('Ctrl Pts',(4.98601051193086,-22.0754161299398,0.));
#33020=CARTESIAN_POINT('Ctrl Pts',(5.0499907220168,-22.1355312202693,0.));
#33021=CARTESIAN_POINT('Ctrl Pts',(5.11451415224483,-22.1953237422816,0.));
#33022=CARTESIAN_POINT('Ctrl Pts',(5.17957547700992,-22.2547923093751,0.));
#33023=CARTESIAN_POINT('Ctrl Pts',(5.24516957209272,-22.3139356039553,0.));
#33024=CARTESIAN_POINT('Ctrl Pts',(5.31129163978934,-22.3727524152125,0.));
#33025=CARTESIAN_POINT('Ctrl Pts',(5.37793718711213,-22.4312416086453,0.));
#33026=CARTESIAN_POINT('Ctrl Pts',(5.44510186987254,-22.4894020366778,0.));
#33027=CARTESIAN_POINT('Ctrl Pts',(5.51278136258485,-22.5472324623564,0.));
#33028=CARTESIAN_POINT('Ctrl Pts',(5.58097123210075,-22.6047314918151,0.));
#33029=CARTESIAN_POINT('Ctrl Pts',(5.64966676217478,-22.6618974767817,0.));
#33030=CARTESIAN_POINT('Ctrl Pts',(5.71886294543539,-22.7187285302677,0.));
#33031=CARTESIAN_POINT('Ctrl Pts',(5.7885547640031,-22.7752227318719,0.));
#33032=CARTESIAN_POINT('Ctrl Pts',(5.85873740439746,-22.8313782965033,0.));
#33033=CARTESIAN_POINT('Ctrl Pts',(5.92940648776744,-22.8871937503747,0.));
#33034=CARTESIAN_POINT('Ctrl Pts',(6.00055830861927,-22.9426681304804,0.));
#33035=CARTESIAN_POINT('Ctrl Pts',(6.08651635230849,-23.0088276997724,0.));
#33036=CARTESIAN_POINT('Ctrl Pts',(6.15874528113544,-23.0635340031629,0.));
#33037=CARTESIAN_POINT('Ctrl Pts',(6.21690914895776,-23.107026289589,0.));
#33038=CARTESIAN_POINT('Ctrl Pts',(6.26074599324761,-23.1394922314359,0.));
#33039=CARTESIAN_POINT('Ctrl Pts',(6.29006564240226,-23.1610680715348,0.));
#33040=CARTESIAN_POINT('Ctrl Pts',(2.66302778805429,-18.6042245638953,15.));
#33041=CARTESIAN_POINT('Ctrl Pts',(2.66524945599054,-18.6197453967525,15.));
#33042=CARTESIAN_POINT('Ctrl Pts',(2.67022099202408,-18.6506703537007,15.));
#33043=CARTESIAN_POINT('Ctrl Pts',(2.67926286296661,-18.696707670787,15.));
#33044=CARTESIAN_POINT('Ctrl Pts',(2.69432739305027,-18.7574274222161,15.));
#33045=CARTESIAN_POINT('Ctrl Pts',(2.71724545050994,-18.8324337861517,15.));
#33046=CARTESIAN_POINT('Ctrl Pts',(2.74308150095404,-18.9068127424043,15.));
#33047=CARTESIAN_POINT('Ctrl Pts',(2.77069196504715,-18.980821277801,15.));
#33048=CARTESIAN_POINT('Ctrl Pts',(2.79926206958176,-19.0546365637297,15.));
#33049=CARTESIAN_POINT('Ctrl Pts',(2.828507852372,-19.1283090202125,15.));
#33050=CARTESIAN_POINT('Ctrl Pts',(2.85848240467741,-19.2018091932025,15.));
#33051=CARTESIAN_POINT('Ctrl Pts',(2.88943670541708,-19.2750617358775,15.));
#33052=CARTESIAN_POINT('Ctrl Pts',(2.92166984506915,-19.3479817954251,15.));
#33053=CARTESIAN_POINT('Ctrl Pts',(2.95535900926266,-19.420516469599,15.));
#33054=CARTESIAN_POINT('Ctrl Pts',(2.99048468792079,-19.4926628032527,15.));
#33055=CARTESIAN_POINT('Ctrl Pts',(3.02691741043283,-19.5644460803884,15.));
#33056=CARTESIAN_POINT('Ctrl Pts',(3.06446889170638,-19.635906849522,15.));
#33057=CARTESIAN_POINT('Ctrl Pts',(3.10295238390997,-19.7070857227052,15.));
#33058=CARTESIAN_POINT('Ctrl Pts',(3.1422513957243,-19.7780060327855,15.));
#33059=CARTESIAN_POINT('Ctrl Pts',(3.18233430962982,-19.8486701154397,15.));
#33060=CARTESIAN_POINT('Ctrl Pts',(3.22321820350857,-19.9190683616661,15.));
#33061=CARTESIAN_POINT('Ctrl Pts',(3.26494616363974,-19.9891848794807,15.));
#33062=CARTESIAN_POINT('Ctrl Pts',(3.30756123886962,-20.0590040020604,15.));
#33063=CARTESIAN_POINT('Ctrl Pts',(3.351076475782,-20.1285177769596,15.));
#33064=CARTESIAN_POINT('Ctrl Pts',(3.39547305068767,-20.1977264147619,15.));
#33065=CARTESIAN_POINT('Ctrl Pts',(3.44071459161672,-20.2666346804507,15.));
#33066=CARTESIAN_POINT('Ctrl Pts',(3.48675677306966,-20.3352494700167,15.));
#33067=CARTESIAN_POINT('Ctrl Pts',(3.53355803178954,-20.4035771072894,15.));
#33068=CARTESIAN_POINT('Ctrl Pts',(3.58109188218494,-20.4716202388531,15.));
#33069=CARTESIAN_POINT('Ctrl Pts',(3.62934618720589,-20.5393780076056,15.));
#33070=CARTESIAN_POINT('Ctrl Pts',(3.67831730617887,-20.6068475141781,15.));
#33071=CARTESIAN_POINT('Ctrl Pts',(3.72800579849619,-20.6740248879992,15.));
#33072=CARTESIAN_POINT('Ctrl Pts',(3.77841179839888,-20.740906441832,15.));
#33073=CARTESIAN_POINT('Ctrl Pts',(3.82952970701915,-20.8074899980321,15.));
#33074=CARTESIAN_POINT('Ctrl Pts',(3.88134876172353,-20.8737747416623,15.));
#33075=CARTESIAN_POINT('Ctrl Pts',(3.93385538070582,-20.9397606289993,15.));
#33076=CARTESIAN_POINT('Ctrl Pts',(3.98703495407281,-21.0054479357374,15.));
#33077=CARTESIAN_POINT('Ctrl Pts',(4.04087373166023,-21.0708367812416,15.));
#33078=CARTESIAN_POINT('Ctrl Pts',(4.09536099504429,-21.1359265833073,15.));
#33079=CARTESIAN_POINT('Ctrl Pts',(4.15048873695645,-21.2007161321625,15.));
#33080=CARTESIAN_POINT('Ctrl Pts',(4.20625065101369,-21.2652038365365,15.));
#33081=CARTESIAN_POINT('Ctrl Pts',(4.26264132842711,-21.3293879189372,15.));
#33082=CARTESIAN_POINT('Ctrl Pts',(4.31965542378783,-21.3932666198096,15.));
#33083=CARTESIAN_POINT('Ctrl Pts',(4.37728667813637,-21.4568384368826,15.));
#33084=CARTESIAN_POINT('Ctrl Pts',(4.43552802047029,-21.5201021036274,15.));
#33085=CARTESIAN_POINT('Ctrl Pts',(4.49437199472474,-21.5830564890896,15.));
#33086=CARTESIAN_POINT('Ctrl Pts',(4.55381108432127,-21.6457005243617,15.));
#33087=CARTESIAN_POINT('Ctrl Pts',(4.6138380475249,-21.7080331252945,15.));
#33088=CARTESIAN_POINT('Ctrl Pts',(4.67444631371023,-21.770053106418,15.));
#33089=CARTESIAN_POINT('Ctrl Pts',(4.73562994468575,-21.8317591750867,15.));
#33090=CARTESIAN_POINT('Ctrl Pts',(4.7973834230091,-21.8931499593332,15.));
#33091=CARTESIAN_POINT('Ctrl Pts',(4.85970148585195,-21.954224026919,15.));
#33092=CARTESIAN_POINT('Ctrl Pts',(4.92257895332778,-22.0149799098431,15.));
#33093=CARTESIAN_POINT('Ctrl Pts',(4.98601051193086,-22.0754161299398,15.));
#33094=CARTESIAN_POINT('Ctrl Pts',(5.0499907220168,-22.1355312202693,15.));
#33095=CARTESIAN_POINT('Ctrl Pts',(5.11451415224483,-22.1953237422816,15.));
#33096=CARTESIAN_POINT('Ctrl Pts',(5.17957547700992,-22.2547923093751,15.));
#33097=CARTESIAN_POINT('Ctrl Pts',(5.24516957209272,-22.3139356039553,15.));
#33098=CARTESIAN_POINT('Ctrl Pts',(5.31129163978934,-22.3727524152125,15.));
#33099=CARTESIAN_POINT('Ctrl Pts',(5.37793718711213,-22.4312416086453,15.));
#33100=CARTESIAN_POINT('Ctrl Pts',(5.44510186987254,-22.4894020366778,15.));
#33101=CARTESIAN_POINT('Ctrl Pts',(5.51278136258485,-22.5472324623564,15.));
#33102=CARTESIAN_POINT('Ctrl Pts',(5.58097123210075,-22.6047314918151,15.));
#33103=CARTESIAN_POINT('Ctrl Pts',(5.64966676217478,-22.6618974767817,15.));
#33104=CARTESIAN_POINT('Ctrl Pts',(5.71886294543539,-22.7187285302677,15.));
#33105=CARTESIAN_POINT('Ctrl Pts',(5.7885547640031,-22.7752227318719,15.));
#33106=CARTESIAN_POINT('Ctrl Pts',(5.85873740439746,-22.8313782965033,15.));
#33107=CARTESIAN_POINT('Ctrl Pts',(5.92940648776744,-22.8871937503747,15.));
#33108=CARTESIAN_POINT('Ctrl Pts',(6.00055830861927,-22.9426681304804,15.));
#33109=CARTESIAN_POINT('Ctrl Pts',(6.08651635230849,-23.0088276997724,15.));
#33110=CARTESIAN_POINT('Ctrl Pts',(6.15874528113544,-23.0635340031629,15.));
#33111=CARTESIAN_POINT('Ctrl Pts',(6.21690914895776,-23.107026289589,15.));
#33112=CARTESIAN_POINT('Ctrl Pts',(6.26074599324761,-23.1394922314359,15.));
#33113=CARTESIAN_POINT('Ctrl Pts',(6.29006564240226,-23.1610680715348,15.));
#33114=CARTESIAN_POINT('Ctrl Pts',(-6.29006564240227,-23.1610680715348,
0.));
#33115=CARTESIAN_POINT('Ctrl Pts',(-6.29006564240227,-23.1610680715348,
18.));
#33116=CARTESIAN_POINT('Ctrl Pts',(-6.27540581784972,-23.1502801515009,
0.));
#33117=CARTESIAN_POINT('Ctrl Pts',(-6.27540581784972,-23.1502801515009,
18.));
#33118=CARTESIAN_POINT('Ctrl Pts',(-6.24613371181767,-23.1286702508203,
0.));
#33119=CARTESIAN_POINT('Ctrl Pts',(-6.24613371181767,-23.1286702508203,
18.));
#33120=CARTESIAN_POINT('Ctrl Pts',(-6.20236818200219,-23.0961532179825,
0.));
#33121=CARTESIAN_POINT('Ctrl Pts',(-6.20236818200219,-23.0961532179825,
18.));
#33122=CARTESIAN_POINT('Ctrl Pts',(-6.14429949537005,-23.0525927424848,
0.));
#33123=CARTESIAN_POINT('Ctrl Pts',(-6.14429949537005,-23.0525927424848,
18.));
#33124=CARTESIAN_POINT('Ctrl Pts',(-6.07219001169363,-22.9978011048904,
0.));
#33125=CARTESIAN_POINT('Ctrl Pts',(-6.07219001169363,-22.9978011048904,
18.));
#33126=CARTESIAN_POINT('Ctrl Pts',(-6.00055830861928,-22.9426681304804,
0.));
#33127=CARTESIAN_POINT('Ctrl Pts',(-6.00055830861928,-22.9426681304804,
18.));
#33128=CARTESIAN_POINT('Ctrl Pts',(-5.92940648776744,-22.8871937503747,
0.));
#33129=CARTESIAN_POINT('Ctrl Pts',(-5.92940648776744,-22.8871937503747,
18.));
#33130=CARTESIAN_POINT('Ctrl Pts',(-5.85873740439747,-22.8313782965033,
0.));
#33131=CARTESIAN_POINT('Ctrl Pts',(-5.85873740439747,-22.8313782965033,
18.));
#33132=CARTESIAN_POINT('Ctrl Pts',(-5.78855476400311,-22.7752227318719,
0.));
#33133=CARTESIAN_POINT('Ctrl Pts',(-5.78855476400311,-22.7752227318719,
18.));
#33134=CARTESIAN_POINT('Ctrl Pts',(-5.71886294543539,-22.7187285302677,
0.));
#33135=CARTESIAN_POINT('Ctrl Pts',(-5.71886294543539,-22.7187285302677,
18.));
#33136=CARTESIAN_POINT('Ctrl Pts',(-5.64966676217478,-22.6618974767817,
0.));
#33137=CARTESIAN_POINT('Ctrl Pts',(-5.64966676217478,-22.6618974767817,
18.));
#33138=CARTESIAN_POINT('Ctrl Pts',(-5.58097123210075,-22.6047314918152,
0.));
#33139=CARTESIAN_POINT('Ctrl Pts',(-5.58097123210075,-22.6047314918152,
18.));
#33140=CARTESIAN_POINT('Ctrl Pts',(-5.51278136258486,-22.5472324623564,
0.));
#33141=CARTESIAN_POINT('Ctrl Pts',(-5.51278136258486,-22.5472324623564,
18.));
#33142=CARTESIAN_POINT('Ctrl Pts',(-5.44510186987254,-22.4894020366778,
0.));
#33143=CARTESIAN_POINT('Ctrl Pts',(-5.44510186987254,-22.4894020366778,
18.));
#33144=CARTESIAN_POINT('Ctrl Pts',(-5.37793718711213,-22.4312416086453,
0.));
#33145=CARTESIAN_POINT('Ctrl Pts',(-5.37793718711213,-22.4312416086453,
18.));
#33146=CARTESIAN_POINT('Ctrl Pts',(-5.31129163978934,-22.3727524152125,
0.));
#33147=CARTESIAN_POINT('Ctrl Pts',(-5.31129163978934,-22.3727524152125,
18.));
#33148=CARTESIAN_POINT('Ctrl Pts',(-5.24516957209273,-22.3139356039553,
0.));
#33149=CARTESIAN_POINT('Ctrl Pts',(-5.24516957209273,-22.3139356039553,
18.));
#33150=CARTESIAN_POINT('Ctrl Pts',(-5.17957547700993,-22.2547923093751,
0.));
#33151=CARTESIAN_POINT('Ctrl Pts',(-5.17957547700993,-22.2547923093751,
18.));
#33152=CARTESIAN_POINT('Ctrl Pts',(-5.11451415224484,-22.1953237422816,
0.));
#33153=CARTESIAN_POINT('Ctrl Pts',(-5.11451415224484,-22.1953237422816,
18.));
#33154=CARTESIAN_POINT('Ctrl Pts',(-5.04999072201681,-22.1355312202693,
0.));
#33155=CARTESIAN_POINT('Ctrl Pts',(-5.04999072201681,-22.1355312202693,
18.));
#33156=CARTESIAN_POINT('Ctrl Pts',(-4.98601051193087,-22.0754161299398,
0.));
#33157=CARTESIAN_POINT('Ctrl Pts',(-4.98601051193087,-22.0754161299398,
18.));
#33158=CARTESIAN_POINT('Ctrl Pts',(-4.92257895332779,-22.0149799098431,
0.));
#33159=CARTESIAN_POINT('Ctrl Pts',(-4.92257895332779,-22.0149799098431,
18.));
#33160=CARTESIAN_POINT('Ctrl Pts',(-4.85970148585196,-21.9542240269191,
0.));
#33161=CARTESIAN_POINT('Ctrl Pts',(-4.85970148585196,-21.9542240269191,
18.));
#33162=CARTESIAN_POINT('Ctrl Pts',(-4.7973834230091,-21.8931499593332,0.));
#33163=CARTESIAN_POINT('Ctrl Pts',(-4.7973834230091,-21.8931499593332,18.));
#33164=CARTESIAN_POINT('Ctrl Pts',(-4.73562994468575,-21.8317591750867,
0.));
#33165=CARTESIAN_POINT('Ctrl Pts',(-4.73562994468575,-21.8317591750867,
18.));
#33166=CARTESIAN_POINT('Ctrl Pts',(-4.67444631371023,-21.770053106418,0.));
#33167=CARTESIAN_POINT('Ctrl Pts',(-4.67444631371023,-21.770053106418,18.));
#33168=CARTESIAN_POINT('Ctrl Pts',(-4.6138380475249,-21.7080331252945,0.));
#33169=CARTESIAN_POINT('Ctrl Pts',(-4.6138380475249,-21.7080331252945,18.));
#33170=CARTESIAN_POINT('Ctrl Pts',(-4.55381108432127,-21.6457005243617,
0.));
#33171=CARTESIAN_POINT('Ctrl Pts',(-4.55381108432127,-21.6457005243617,
18.));
#33172=CARTESIAN_POINT('Ctrl Pts',(-4.49437199472475,-21.5830564890896,
0.));
#33173=CARTESIAN_POINT('Ctrl Pts',(-4.49437199472475,-21.5830564890896,
18.));
#33174=CARTESIAN_POINT('Ctrl Pts',(-4.4355280204703,-21.5201021036274,0.));
#33175=CARTESIAN_POINT('Ctrl Pts',(-4.4355280204703,-21.5201021036274,18.));
#33176=CARTESIAN_POINT('Ctrl Pts',(-4.37728667813637,-21.4568384368826,
0.));
#33177=CARTESIAN_POINT('Ctrl Pts',(-4.37728667813637,-21.4568384368826,
18.));
#33178=CARTESIAN_POINT('Ctrl Pts',(-4.31965542378783,-21.3932666198096,
0.));
#33179=CARTESIAN_POINT('Ctrl Pts',(-4.31965542378783,-21.3932666198096,
18.));
#33180=CARTESIAN_POINT('Ctrl Pts',(-4.26264132842712,-21.3293879189372,
0.));
#33181=CARTESIAN_POINT('Ctrl Pts',(-4.26264132842712,-21.3293879189372,
18.));
#33182=CARTESIAN_POINT('Ctrl Pts',(-4.20625065101369,-21.2652038365365,
0.));
#33183=CARTESIAN_POINT('Ctrl Pts',(-4.20625065101369,-21.2652038365365,
18.));
#33184=CARTESIAN_POINT('Ctrl Pts',(-4.15048873695646,-21.2007161321625,
0.));
#33185=CARTESIAN_POINT('Ctrl Pts',(-4.15048873695646,-21.2007161321625,
18.));
#33186=CARTESIAN_POINT('Ctrl Pts',(-4.09536099504429,-21.1359265833073,
0.));
#33187=CARTESIAN_POINT('Ctrl Pts',(-4.09536099504429,-21.1359265833073,
18.));
#33188=CARTESIAN_POINT('Ctrl Pts',(-4.04087373166023,-21.0708367812416,
0.));
#33189=CARTESIAN_POINT('Ctrl Pts',(-4.04087373166023,-21.0708367812416,
18.));
#33190=CARTESIAN_POINT('Ctrl Pts',(-3.98703495407281,-21.0054479357374,
0.));
#33191=CARTESIAN_POINT('Ctrl Pts',(-3.98703495407281,-21.0054479357374,
18.));
#33192=CARTESIAN_POINT('Ctrl Pts',(-3.93385538070582,-20.9397606289993,
0.));
#33193=CARTESIAN_POINT('Ctrl Pts',(-3.93385538070582,-20.9397606289993,
18.));
#33194=CARTESIAN_POINT('Ctrl Pts',(-3.88134876172354,-20.8737747416623,
0.));
#33195=CARTESIAN_POINT('Ctrl Pts',(-3.88134876172354,-20.8737747416623,
18.));
#33196=CARTESIAN_POINT('Ctrl Pts',(-3.82952970701916,-20.8074899980321,
0.));
#33197=CARTESIAN_POINT('Ctrl Pts',(-3.82952970701916,-20.8074899980321,
18.));
#33198=CARTESIAN_POINT('Ctrl Pts',(-3.77841179839888,-20.740906441832,0.));
#33199=CARTESIAN_POINT('Ctrl Pts',(-3.77841179839888,-20.740906441832,18.));
#33200=CARTESIAN_POINT('Ctrl Pts',(-3.7280057984962,-20.6740248879992,0.));
#33201=CARTESIAN_POINT('Ctrl Pts',(-3.7280057984962,-20.6740248879992,18.));
#33202=CARTESIAN_POINT('Ctrl Pts',(-3.67831730617888,-20.6068475141781,
0.));
#33203=CARTESIAN_POINT('Ctrl Pts',(-3.67831730617888,-20.6068475141781,
18.));
#33204=CARTESIAN_POINT('Ctrl Pts',(-3.6293461872059,-20.5393780076057,0.));
#33205=CARTESIAN_POINT('Ctrl Pts',(-3.6293461872059,-20.5393780076057,18.));
#33206=CARTESIAN_POINT('Ctrl Pts',(-3.58109188218494,-20.4716202388531,
0.));
#33207=CARTESIAN_POINT('Ctrl Pts',(-3.58109188218494,-20.4716202388531,
18.));
#33208=CARTESIAN_POINT('Ctrl Pts',(-3.53355803178955,-20.4035771072894,
0.));
#33209=CARTESIAN_POINT('Ctrl Pts',(-3.53355803178955,-20.4035771072894,
18.));
#33210=CARTESIAN_POINT('Ctrl Pts',(-3.48675677306967,-20.3352494700167,
0.));
#33211=CARTESIAN_POINT('Ctrl Pts',(-3.48675677306967,-20.3352494700167,
18.));
#33212=CARTESIAN_POINT('Ctrl Pts',(-3.44071459161672,-20.2666346804507,
0.));
#33213=CARTESIAN_POINT('Ctrl Pts',(-3.44071459161672,-20.2666346804507,
18.));
#33214=CARTESIAN_POINT('Ctrl Pts',(-3.39547305068768,-20.1977264147619,
0.));
#33215=CARTESIAN_POINT('Ctrl Pts',(-3.39547305068768,-20.1977264147619,
18.));
#33216=CARTESIAN_POINT('Ctrl Pts',(-3.35107647578201,-20.1285177769596,
0.));
#33217=CARTESIAN_POINT('Ctrl Pts',(-3.35107647578201,-20.1285177769596,
18.));
#33218=CARTESIAN_POINT('Ctrl Pts',(-3.30756123886962,-20.0590040020604,
0.));
#33219=CARTESIAN_POINT('Ctrl Pts',(-3.30756123886962,-20.0590040020604,
18.));
#33220=CARTESIAN_POINT('Ctrl Pts',(-3.26494616363974,-19.9891848794807,
0.));
#33221=CARTESIAN_POINT('Ctrl Pts',(-3.26494616363974,-19.9891848794807,
18.));
#33222=CARTESIAN_POINT('Ctrl Pts',(-3.22321820350857,-19.9190683616661,
0.));
#33223=CARTESIAN_POINT('Ctrl Pts',(-3.22321820350857,-19.9190683616661,
18.));
#33224=CARTESIAN_POINT('Ctrl Pts',(-3.18233430962982,-19.8486701154397,
0.));
#33225=CARTESIAN_POINT('Ctrl Pts',(-3.18233430962982,-19.8486701154397,
18.));
#33226=CARTESIAN_POINT('Ctrl Pts',(-3.14225139572431,-19.7780060327855,
0.));
#33227=CARTESIAN_POINT('Ctrl Pts',(-3.14225139572431,-19.7780060327855,
18.));
#33228=CARTESIAN_POINT('Ctrl Pts',(-3.10295238390997,-19.7070857227052,
0.));
#33229=CARTESIAN_POINT('Ctrl Pts',(-3.10295238390997,-19.7070857227052,
18.));
#33230=CARTESIAN_POINT('Ctrl Pts',(-3.06446889170638,-19.635906849522,0.));
#33231=CARTESIAN_POINT('Ctrl Pts',(-3.06446889170638,-19.635906849522,18.));
#33232=CARTESIAN_POINT('Ctrl Pts',(-3.02691741043284,-19.5644460803884,
0.));
#33233=CARTESIAN_POINT('Ctrl Pts',(-3.02691741043284,-19.5644460803884,
18.));
#33234=CARTESIAN_POINT('Ctrl Pts',(-2.99048468792079,-19.4926628032527,
0.));
#33235=CARTESIAN_POINT('Ctrl Pts',(-2.99048468792079,-19.4926628032527,
18.));
#33236=CARTESIAN_POINT('Ctrl Pts',(-2.95535900926266,-19.420516469599,0.));
#33237=CARTESIAN_POINT('Ctrl Pts',(-2.95535900926266,-19.420516469599,18.));
#33238=CARTESIAN_POINT('Ctrl Pts',(-2.92166984506916,-19.3479817954251,
0.));
#33239=CARTESIAN_POINT('Ctrl Pts',(-2.92166984506916,-19.3479817954251,
18.));
#33240=CARTESIAN_POINT('Ctrl Pts',(-2.88943670541709,-19.2750617358775,
0.));
#33241=CARTESIAN_POINT('Ctrl Pts',(-2.88943670541709,-19.2750617358775,
18.));
#33242=CARTESIAN_POINT('Ctrl Pts',(-2.85848240467742,-19.2018091932025,
0.));
#33243=CARTESIAN_POINT('Ctrl Pts',(-2.85848240467742,-19.2018091932025,
18.));
#33244=CARTESIAN_POINT('Ctrl Pts',(-2.828507852372,-19.1283090202125,0.));
#33245=CARTESIAN_POINT('Ctrl Pts',(-2.828507852372,-19.1283090202125,18.));
#33246=CARTESIAN_POINT('Ctrl Pts',(-2.79926206958176,-19.0546365637297,
0.));
#33247=CARTESIAN_POINT('Ctrl Pts',(-2.79926206958176,-19.0546365637297,
18.));
#33248=CARTESIAN_POINT('Ctrl Pts',(-2.77069196504715,-18.980821277801,0.));
#33249=CARTESIAN_POINT('Ctrl Pts',(-2.77069196504715,-18.980821277801,18.));
#33250=CARTESIAN_POINT('Ctrl Pts',(-2.74308150095405,-18.9068127424043,
0.));
#33251=CARTESIAN_POINT('Ctrl Pts',(-2.74308150095405,-18.9068127424043,
18.));
#33252=CARTESIAN_POINT('Ctrl Pts',(-2.71724545050995,-18.8324337861517,
0.));
#33253=CARTESIAN_POINT('Ctrl Pts',(-2.71724545050995,-18.8324337861517,
18.));
#33254=CARTESIAN_POINT('Ctrl Pts',(-2.69432739305028,-18.7574274222161,
0.));
#33255=CARTESIAN_POINT('Ctrl Pts',(-2.69432739305028,-18.7574274222161,
18.));
#33256=CARTESIAN_POINT('Ctrl Pts',(-2.67926286296662,-18.696707670787,0.));
#33257=CARTESIAN_POINT('Ctrl Pts',(-2.67926286296662,-18.696707670787,18.));
#33258=CARTESIAN_POINT('Ctrl Pts',(-2.67022099202409,-18.6506703537007,
0.));
#33259=CARTESIAN_POINT('Ctrl Pts',(-2.67022099202409,-18.6506703537007,
18.));
#33260=CARTESIAN_POINT('Ctrl Pts',(-2.66524945599055,-18.6197453967525,
0.));
#33261=CARTESIAN_POINT('Ctrl Pts',(-2.66524945599055,-18.6197453967525,
18.));
#33262=CARTESIAN_POINT('Ctrl Pts',(-2.6630277880543,-18.6042245638953,0.));
#33263=CARTESIAN_POINT('Ctrl Pts',(-2.6630277880543,-18.6042245638953,18.));
#33264=CARTESIAN_POINT('',(-6.29006564240232,-23.1610680715348,0.));
#33265=CARTESIAN_POINT('Ctrl Pts',(-2.6630277880543,-18.6042245638953,0.));
#33266=CARTESIAN_POINT('Ctrl Pts',(-2.66524945599055,-18.6197453967525,
0.));
#33267=CARTESIAN_POINT('Ctrl Pts',(-2.67022099202409,-18.6506703537007,
0.));
#33268=CARTESIAN_POINT('Ctrl Pts',(-2.67926286296662,-18.696707670787,0.));
#33269=CARTESIAN_POINT('Ctrl Pts',(-2.69432739305028,-18.7574274222161,
0.));
#33270=CARTESIAN_POINT('Ctrl Pts',(-2.71724545050995,-18.8324337861517,
0.));
#33271=CARTESIAN_POINT('Ctrl Pts',(-2.74308150095405,-18.9068127424043,
0.));
#33272=CARTESIAN_POINT('Ctrl Pts',(-2.77069196504715,-18.980821277801,0.));
#33273=CARTESIAN_POINT('Ctrl Pts',(-2.79926206958176,-19.0546365637297,
0.));
#33274=CARTESIAN_POINT('Ctrl Pts',(-2.828507852372,-19.1283090202125,0.));
#33275=CARTESIAN_POINT('Ctrl Pts',(-2.85848240467742,-19.2018091932025,
0.));
#33276=CARTESIAN_POINT('Ctrl Pts',(-2.88943670541709,-19.2750617358775,
0.));
#33277=CARTESIAN_POINT('Ctrl Pts',(-2.92166984506916,-19.3479817954251,
0.));
#33278=CARTESIAN_POINT('Ctrl Pts',(-2.95535900926266,-19.420516469599,0.));
#33279=CARTESIAN_POINT('Ctrl Pts',(-2.99048468792079,-19.4926628032527,
0.));
#33280=CARTESIAN_POINT('Ctrl Pts',(-3.02691741043284,-19.5644460803884,
0.));
#33281=CARTESIAN_POINT('Ctrl Pts',(-3.06446889170638,-19.635906849522,0.));
#33282=CARTESIAN_POINT('Ctrl Pts',(-3.10295238390997,-19.7070857227052,
0.));
#33283=CARTESIAN_POINT('Ctrl Pts',(-3.14225139572431,-19.7780060327855,
0.));
#33284=CARTESIAN_POINT('Ctrl Pts',(-3.18233430962982,-19.8486701154397,
0.));
#33285=CARTESIAN_POINT('Ctrl Pts',(-3.22321820350857,-19.9190683616661,
0.));
#33286=CARTESIAN_POINT('Ctrl Pts',(-3.26494616363974,-19.9891848794807,
0.));
#33287=CARTESIAN_POINT('Ctrl Pts',(-3.30756123886962,-20.0590040020604,
0.));
#33288=CARTESIAN_POINT('Ctrl Pts',(-3.35107647578201,-20.1285177769596,
0.));
#33289=CARTESIAN_POINT('Ctrl Pts',(-3.39547305068768,-20.1977264147619,
0.));
#33290=CARTESIAN_POINT('Ctrl Pts',(-3.44071459161672,-20.2666346804507,
0.));
#33291=CARTESIAN_POINT('Ctrl Pts',(-3.48675677306967,-20.3352494700167,
0.));
#33292=CARTESIAN_POINT('Ctrl Pts',(-3.53355803178955,-20.4035771072894,
0.));
#33293=CARTESIAN_POINT('Ctrl Pts',(-3.58109188218494,-20.4716202388531,
0.));
#33294=CARTESIAN_POINT('Ctrl Pts',(-3.6293461872059,-20.5393780076057,0.));
#33295=CARTESIAN_POINT('Ctrl Pts',(-3.67831730617888,-20.6068475141781,
0.));
#33296=CARTESIAN_POINT('Ctrl Pts',(-3.7280057984962,-20.6740248879992,0.));
#33297=CARTESIAN_POINT('Ctrl Pts',(-3.77841179839888,-20.740906441832,0.));
#33298=CARTESIAN_POINT('Ctrl Pts',(-3.82952970701916,-20.8074899980321,
0.));
#33299=CARTESIAN_POINT('Ctrl Pts',(-3.88134876172354,-20.8737747416623,
0.));
#33300=CARTESIAN_POINT('Ctrl Pts',(-3.93385538070582,-20.9397606289993,
0.));
#33301=CARTESIAN_POINT('Ctrl Pts',(-3.98703495407281,-21.0054479357374,
0.));
#33302=CARTESIAN_POINT('Ctrl Pts',(-4.04087373166023,-21.0708367812416,
0.));
#33303=CARTESIAN_POINT('Ctrl Pts',(-4.09536099504429,-21.1359265833073,
0.));
#33304=CARTESIAN_POINT('Ctrl Pts',(-4.15048873695646,-21.2007161321625,
0.));
#33305=CARTESIAN_POINT('Ctrl Pts',(-4.20625065101369,-21.2652038365365,
0.));
#33306=CARTESIAN_POINT('Ctrl Pts',(-4.26264132842712,-21.3293879189372,
0.));
#33307=CARTESIAN_POINT('Ctrl Pts',(-4.31965542378783,-21.3932666198096,
0.));
#33308=CARTESIAN_POINT('Ctrl Pts',(-4.37728667813637,-21.4568384368826,
0.));
#33309=CARTESIAN_POINT('Ctrl Pts',(-4.4355280204703,-21.5201021036274,0.));
#33310=CARTESIAN_POINT('Ctrl Pts',(-4.49437199472475,-21.5830564890896,
0.));
#33311=CARTESIAN_POINT('Ctrl Pts',(-4.55381108432127,-21.6457005243617,
0.));
#33312=CARTESIAN_POINT('Ctrl Pts',(-4.6138380475249,-21.7080331252945,0.));
#33313=CARTESIAN_POINT('Ctrl Pts',(-4.67444631371023,-21.770053106418,0.));
#33314=CARTESIAN_POINT('Ctrl Pts',(-4.73562994468575,-21.8317591750867,
0.));
#33315=CARTESIAN_POINT('Ctrl Pts',(-4.7973834230091,-21.8931499593332,0.));
#33316=CARTESIAN_POINT('Ctrl Pts',(-4.85970148585196,-21.9542240269191,
0.));
#33317=CARTESIAN_POINT('Ctrl Pts',(-4.92257895332779,-22.0149799098431,
0.));
#33318=CARTESIAN_POINT('Ctrl Pts',(-4.98601051193087,-22.0754161299398,
0.));
#33319=CARTESIAN_POINT('Ctrl Pts',(-5.04999072201681,-22.1355312202693,
0.));
#33320=CARTESIAN_POINT('Ctrl Pts',(-5.11451415224484,-22.1953237422816,
0.));
#33321=CARTESIAN_POINT('Ctrl Pts',(-5.17957547700993,-22.2547923093751,
0.));
#33322=CARTESIAN_POINT('Ctrl Pts',(-5.24516957209273,-22.3139356039553,
0.));
#33323=CARTESIAN_POINT('Ctrl Pts',(-5.31129163978934,-22.3727524152125,
0.));
#33324=CARTESIAN_POINT('Ctrl Pts',(-5.37793718711213,-22.4312416086453,
0.));
#33325=CARTESIAN_POINT('Ctrl Pts',(-5.44510186987254,-22.4894020366778,
0.));
#33326=CARTESIAN_POINT('Ctrl Pts',(-5.51278136258486,-22.5472324623564,
0.));
#33327=CARTESIAN_POINT('Ctrl Pts',(-5.58097123210075,-22.6047314918152,
0.));
#33328=CARTESIAN_POINT('Ctrl Pts',(-5.64966676217478,-22.6618974767817,
0.));
#33329=CARTESIAN_POINT('Ctrl Pts',(-5.71886294543539,-22.7187285302677,
0.));
#33330=CARTESIAN_POINT('Ctrl Pts',(-5.78855476400311,-22.7752227318719,
0.));
#33331=CARTESIAN_POINT('Ctrl Pts',(-5.85873740439747,-22.8313782965033,
0.));
#33332=CARTESIAN_POINT('Ctrl Pts',(-5.92940648776744,-22.8871937503747,
0.));
#33333=CARTESIAN_POINT('Ctrl Pts',(-6.00055830861928,-22.9426681304804,
0.));
#33334=CARTESIAN_POINT('Ctrl Pts',(-6.0865163523085,-23.0088276997724,0.));
#33335=CARTESIAN_POINT('Ctrl Pts',(-6.15874528113544,-23.0635340031629,
0.));
#33336=CARTESIAN_POINT('Ctrl Pts',(-6.21690914895778,-23.107026289589,0.));
#33337=CARTESIAN_POINT('Ctrl Pts',(-6.26074599324762,-23.1394922314359,
0.));
#33338=CARTESIAN_POINT('Ctrl Pts',(-6.29006564240227,-23.1610680715348,
0.));
#33339=CARTESIAN_POINT('',(-6.29006564240232,-23.1610680715348,15.));
#33340=CARTESIAN_POINT('Ctrl Pts',(-6.29006564240227,-23.1610680715348,
15.));
#33341=CARTESIAN_POINT('Ctrl Pts',(-6.27540581784972,-23.1502801515009,
15.));
#33342=CARTESIAN_POINT('Ctrl Pts',(-6.24613371181767,-23.1286702508203,
15.));
#33343=CARTESIAN_POINT('Ctrl Pts',(-6.20236818200219,-23.0961532179825,
15.));
#33344=CARTESIAN_POINT('Ctrl Pts',(-6.14429949537005,-23.0525927424848,
15.));
#33345=CARTESIAN_POINT('Ctrl Pts',(-6.07219001169363,-22.9978011048904,
15.));
#33346=CARTESIAN_POINT('Ctrl Pts',(-6.00055830861928,-22.9426681304804,
15.));
#33347=CARTESIAN_POINT('Ctrl Pts',(-5.92940648776744,-22.8871937503747,
15.));
#33348=CARTESIAN_POINT('Ctrl Pts',(-5.85873740439747,-22.8313782965033,
15.));
#33349=CARTESIAN_POINT('Ctrl Pts',(-5.78855476400311,-22.7752227318719,
15.));
#33350=CARTESIAN_POINT('Ctrl Pts',(-5.71886294543539,-22.7187285302677,
15.));
#33351=CARTESIAN_POINT('Ctrl Pts',(-5.64966676217478,-22.6618974767817,
15.));
#33352=CARTESIAN_POINT('Ctrl Pts',(-5.58097123210075,-22.6047314918152,
15.));
#33353=CARTESIAN_POINT('Ctrl Pts',(-5.51278136258486,-22.5472324623564,
15.));
#33354=CARTESIAN_POINT('Ctrl Pts',(-5.44510186987254,-22.4894020366778,
15.));
#33355=CARTESIAN_POINT('Ctrl Pts',(-5.37793718711213,-22.4312416086453,
15.));
#33356=CARTESIAN_POINT('Ctrl Pts',(-5.31129163978934,-22.3727524152125,
15.));
#33357=CARTESIAN_POINT('Ctrl Pts',(-5.24516957209273,-22.3139356039553,
15.));
#33358=CARTESIAN_POINT('Ctrl Pts',(-5.17957547700993,-22.2547923093751,
15.));
#33359=CARTESIAN_POINT('Ctrl Pts',(-5.11451415224484,-22.1953237422816,
15.));
#33360=CARTESIAN_POINT('Ctrl Pts',(-5.04999072201681,-22.1355312202693,
15.));
#33361=CARTESIAN_POINT('Ctrl Pts',(-4.98601051193087,-22.0754161299398,
15.));
#33362=CARTESIAN_POINT('Ctrl Pts',(-4.92257895332779,-22.0149799098431,
15.));
#33363=CARTESIAN_POINT('Ctrl Pts',(-4.85970148585196,-21.9542240269191,
15.));
#33364=CARTESIAN_POINT('Ctrl Pts',(-4.7973834230091,-21.8931499593332,15.));
#33365=CARTESIAN_POINT('Ctrl Pts',(-4.73562994468575,-21.8317591750867,
15.));
#33366=CARTESIAN_POINT('Ctrl Pts',(-4.67444631371023,-21.770053106418,15.));
#33367=CARTESIAN_POINT('Ctrl Pts',(-4.6138380475249,-21.7080331252945,15.));
#33368=CARTESIAN_POINT('Ctrl Pts',(-4.55381108432127,-21.6457005243617,
15.));
#33369=CARTESIAN_POINT('Ctrl Pts',(-4.49437199472475,-21.5830564890896,
15.));
#33370=CARTESIAN_POINT('Ctrl Pts',(-4.4355280204703,-21.5201021036274,15.));
#33371=CARTESIAN_POINT('Ctrl Pts',(-4.37728667813637,-21.4568384368826,
15.));
#33372=CARTESIAN_POINT('Ctrl Pts',(-4.31965542378783,-21.3932666198096,
15.));
#33373=CARTESIAN_POINT('Ctrl Pts',(-4.26264132842712,-21.3293879189372,
15.));
#33374=CARTESIAN_POINT('Ctrl Pts',(-4.20625065101369,-21.2652038365365,
15.));
#33375=CARTESIAN_POINT('Ctrl Pts',(-4.15048873695646,-21.2007161321625,
15.));
#33376=CARTESIAN_POINT('Ctrl Pts',(-4.09536099504429,-21.1359265833073,
15.));
#33377=CARTESIAN_POINT('Ctrl Pts',(-4.04087373166023,-21.0708367812416,
15.));
#33378=CARTESIAN_POINT('Ctrl Pts',(-3.98703495407281,-21.0054479357374,
15.));
#33379=CARTESIAN_POINT('Ctrl Pts',(-3.93385538070582,-20.9397606289993,
15.));
#33380=CARTESIAN_POINT('Ctrl Pts',(-3.88134876172354,-20.8737747416623,
15.));
#33381=CARTESIAN_POINT('Ctrl Pts',(-3.82952970701916,-20.8074899980321,
15.));
#33382=CARTESIAN_POINT('Ctrl Pts',(-3.77841179839888,-20.740906441832,15.));
#33383=CARTESIAN_POINT('Ctrl Pts',(-3.7280057984962,-20.6740248879992,15.));
#33384=CARTESIAN_POINT('Ctrl Pts',(-3.67831730617888,-20.6068475141781,
15.));
#33385=CARTESIAN_POINT('Ctrl Pts',(-3.6293461872059,-20.5393780076057,15.));
#33386=CARTESIAN_POINT('Ctrl Pts',(-3.58109188218494,-20.4716202388531,
15.));
#33387=CARTESIAN_POINT('Ctrl Pts',(-3.53355803178955,-20.4035771072894,
15.));
#33388=CARTESIAN_POINT('Ctrl Pts',(-3.48675677306967,-20.3352494700167,
15.));
#33389=CARTESIAN_POINT('Ctrl Pts',(-3.44071459161672,-20.2666346804507,
15.));
#33390=CARTESIAN_POINT('Ctrl Pts',(-3.39547305068768,-20.1977264147619,
15.));
#33391=CARTESIAN_POINT('Ctrl Pts',(-3.35107647578201,-20.1285177769596,
15.));
#33392=CARTESIAN_POINT('Ctrl Pts',(-3.30756123886962,-20.0590040020604,
15.));
#33393=CARTESIAN_POINT('Ctrl Pts',(-3.26494616363974,-19.9891848794807,
15.));
#33394=CARTESIAN_POINT('Ctrl Pts',(-3.22321820350857,-19.9190683616661,
15.));
#33395=CARTESIAN_POINT('Ctrl Pts',(-3.18233430962982,-19.8486701154397,
15.));
#33396=CARTESIAN_POINT('Ctrl Pts',(-3.14225139572431,-19.7780060327855,
15.));
#33397=CARTESIAN_POINT('Ctrl Pts',(-3.10295238390997,-19.7070857227052,
15.));
#33398=CARTESIAN_POINT('Ctrl Pts',(-3.06446889170638,-19.635906849522,15.));
#33399=CARTESIAN_POINT('Ctrl Pts',(-3.02691741043284,-19.5644460803884,
15.));
#33400=CARTESIAN_POINT('Ctrl Pts',(-2.99048468792079,-19.4926628032527,
15.));
#33401=CARTESIAN_POINT('Ctrl Pts',(-2.95535900926266,-19.420516469599,15.));
#33402=CARTESIAN_POINT('Ctrl Pts',(-2.92166984506916,-19.3479817954251,
15.));
#33403=CARTESIAN_POINT('Ctrl Pts',(-2.88943670541709,-19.2750617358775,
15.));
#33404=CARTESIAN_POINT('Ctrl Pts',(-2.85848240467742,-19.2018091932025,
15.));
#33405=CARTESIAN_POINT('Ctrl Pts',(-2.828507852372,-19.1283090202125,15.));
#33406=CARTESIAN_POINT('Ctrl Pts',(-2.79926206958176,-19.0546365637297,
15.));
#33407=CARTESIAN_POINT('Ctrl Pts',(-2.77069196504715,-18.980821277801,15.));
#33408=CARTESIAN_POINT('Ctrl Pts',(-2.74308150095405,-18.9068127424043,
15.));
#33409=CARTESIAN_POINT('Ctrl Pts',(-2.71724545050995,-18.8324337861517,
15.));
#33410=CARTESIAN_POINT('Ctrl Pts',(-2.69432739305028,-18.7574274222161,
15.));
#33411=CARTESIAN_POINT('Ctrl Pts',(-2.67926286296662,-18.696707670787,15.));
#33412=CARTESIAN_POINT('Ctrl Pts',(-2.67022099202409,-18.6506703537007,
15.));
#33413=CARTESIAN_POINT('Ctrl Pts',(-2.66524945599055,-18.6197453967525,
15.));
#33414=CARTESIAN_POINT('Ctrl Pts',(-2.6630277880543,-18.6042245638953,15.));
#33415=CARTESIAN_POINT('',(-6.29006564240232,-23.1610680715348,0.));
#33416=CARTESIAN_POINT('Origin',(-3.5746082146807E-14,-1.09790581218125E-13,
0.));
#33417=CARTESIAN_POINT('',(-8.52496423935285,-22.4349054983023,0.));
#33418=CARTESIAN_POINT('Origin',(-3.5746082146807E-14,-1.09790581218125E-13,
0.));
#33419=CARTESIAN_POINT('',(-8.52496423935285,-22.4349054983023,15.));
#33420=CARTESIAN_POINT('Origin',(-3.5746082146807E-14,-1.09790581218125E-13,
15.));
#33421=CARTESIAN_POINT('',(-8.52496423935285,-22.4349054983023,0.));
#33422=CARTESIAN_POINT('Ctrl Pts',(-8.7808540919664,-16.6164222996225,0.));
#33423=CARTESIAN_POINT('Ctrl Pts',(-8.7808540919664,-16.6164222996225,18.));
#33424=CARTESIAN_POINT('Ctrl Pts',(-8.78817964150686,-16.6302847808193,
0.));
#33425=CARTESIAN_POINT('Ctrl Pts',(-8.78817964150686,-16.6302847808193,
18.));
#33426=CARTESIAN_POINT('Ctrl Pts',(-8.80233481798951,-16.6582257921024,
0.));
#33427=CARTESIAN_POINT('Ctrl Pts',(-8.80233481798951,-16.6582257921024,
18.));
#33428=CARTESIAN_POINT('Ctrl Pts',(-8.82207984677447,-16.7007854423938,
0.));
#33429=CARTESIAN_POINT('Ctrl Pts',(-8.82207984677447,-16.7007854423938,
18.));
#33430=CARTESIAN_POINT('Ctrl Pts',(-8.84558256033742,-16.7587634618101,
0.));
#33431=CARTESIAN_POINT('Ctrl Pts',(-8.84558256033742,-16.7587634618101,
18.));
#33432=CARTESIAN_POINT('Ctrl Pts',(-8.87112909692392,-16.8329157811062,
0.));
#33433=CARTESIAN_POINT('Ctrl Pts',(-8.87112909692392,-16.8329157811062,
18.));
#33434=CARTESIAN_POINT('Ctrl Pts',(-8.89394614661329,-16.908275670167,0.));
#33435=CARTESIAN_POINT('Ctrl Pts',(-8.89394614661329,-16.908275670167,18.));
#33436=CARTESIAN_POINT('Ctrl Pts',(-8.91510993758933,-16.9843788566346,
0.));
#33437=CARTESIAN_POINT('Ctrl Pts',(-8.91510993758933,-16.9843788566346,
18.));
#33438=CARTESIAN_POINT('Ctrl Pts',(-8.93538377395244,-17.0608897634975,
0.));
#33439=CARTESIAN_POINT('Ctrl Pts',(-8.93538377395244,-17.0608897634975,
18.));
#33440=CARTESIAN_POINT('Ctrl Pts',(-8.95502702208204,-17.1376822726252,
0.));
#33441=CARTESIAN_POINT('Ctrl Pts',(-8.95502702208204,-17.1376822726252,
18.));
#33442=CARTESIAN_POINT('Ctrl Pts',(-8.97397941759265,-17.2147637614528,
0.));
#33443=CARTESIAN_POINT('Ctrl Pts',(-8.97397941759265,-17.2147637614528,
18.));
#33444=CARTESIAN_POINT('Ctrl Pts',(-8.99199362652257,-17.2922207948279,
0.));
#33445=CARTESIAN_POINT('Ctrl Pts',(-8.99199362652257,-17.2922207948279,
18.));
#33446=CARTESIAN_POINT('Ctrl Pts',(-9.00877780436037,-17.3701605263553,
0.));
#33447=CARTESIAN_POINT('Ctrl Pts',(-9.00877780436037,-17.3701605263553,
18.));
#33448=CARTESIAN_POINT('Ctrl Pts',(-9.0241575097608,-17.4486443043185,0.));
#33449=CARTESIAN_POINT('Ctrl Pts',(-9.0241575097608,-17.4486443043185,18.));
#33450=CARTESIAN_POINT('Ctrl Pts',(-9.03814678971601,-17.5276582702181,
0.));
#33451=CARTESIAN_POINT('Ctrl Pts',(-9.03814678971601,-17.5276582702181,
18.));
#33452=CARTESIAN_POINT('Ctrl Pts',(-9.05086524971401,-17.6071467783263,
0.));
#33453=CARTESIAN_POINT('Ctrl Pts',(-9.05086524971401,-17.6071467783263,
18.));
#33454=CARTESIAN_POINT('Ctrl Pts',(-9.06248904941395,-17.6870319618808,
0.));
#33455=CARTESIAN_POINT('Ctrl Pts',(-9.06248904941395,-17.6870319618808,
18.));
#33456=CARTESIAN_POINT('Ctrl Pts',(-9.07319314215027,-17.7672369091005,
0.));
#33457=CARTESIAN_POINT('Ctrl Pts',(-9.07319314215027,-17.7672369091005,
18.));
#33458=CARTESIAN_POINT('Ctrl Pts',(-9.08308548608349,-17.8477120247758,
0.));
#33459=CARTESIAN_POINT('Ctrl Pts',(-9.08308548608349,-17.8477120247758,
18.));
#33460=CARTESIAN_POINT('Ctrl Pts',(-9.09219303320079,-17.9284406141976,
0.));
#33461=CARTESIAN_POINT('Ctrl Pts',(-9.09219303320079,-17.9284406141976,
18.));
#33462=CARTESIAN_POINT('Ctrl Pts',(-9.10049631917583,-18.0094249416472,
0.));
#33463=CARTESIAN_POINT('Ctrl Pts',(-9.10049631917583,-18.0094249416472,
18.));
#33464=CARTESIAN_POINT('Ctrl Pts',(-9.10795114540259,-18.0906774757189,
0.));
#33465=CARTESIAN_POINT('Ctrl Pts',(-9.10795114540259,-18.0906774757189,
18.));
#33466=CARTESIAN_POINT('Ctrl Pts',(-9.1145134759054,-18.1722108451637,0.));
#33467=CARTESIAN_POINT('Ctrl Pts',(-9.1145134759054,-18.1722108451637,18.));
#33468=CARTESIAN_POINT('Ctrl Pts',(-9.12016808144599,-18.2540262849075,
0.));
#33469=CARTESIAN_POINT('Ctrl Pts',(-9.12016808144599,-18.2540262849075,
18.));
#33470=CARTESIAN_POINT('Ctrl Pts',(-9.12493031448672,-18.3361129010289,
0.));
#33471=CARTESIAN_POINT('Ctrl Pts',(-9.12493031448672,-18.3361129010289,
18.));
#33472=CARTESIAN_POINT('Ctrl Pts',(-9.12883240135631,-18.4184531695731,
0.));
#33473=CARTESIAN_POINT('Ctrl Pts',(-9.12883240135631,-18.4184531695731,
18.));
#33474=CARTESIAN_POINT('Ctrl Pts',(-9.13191425549883,-18.5010266156389,
0.));
#33475=CARTESIAN_POINT('Ctrl Pts',(-9.13191425549883,-18.5010266156389,
18.));
#33476=CARTESIAN_POINT('Ctrl Pts',(-9.13421321934922,-18.5838139250423,
0.));
#33477=CARTESIAN_POINT('Ctrl Pts',(-9.13421321934922,-18.5838139250423,
18.));
#33478=CARTESIAN_POINT('Ctrl Pts',(-9.13575227582419,-18.6668016710749,
0.));
#33479=CARTESIAN_POINT('Ctrl Pts',(-9.13575227582419,-18.6668016710749,
18.));
#33480=CARTESIAN_POINT('Ctrl Pts',(-9.13654074021147,-18.7499820263476,
0.));
#33481=CARTESIAN_POINT('Ctrl Pts',(-9.13654074021147,-18.7499820263476,
18.));
#33482=CARTESIAN_POINT('Ctrl Pts',(-9.13657985367154,-18.8333505052874,
0.));
#33483=CARTESIAN_POINT('Ctrl Pts',(-9.13657985367154,-18.8333505052874,
18.));
#33484=CARTESIAN_POINT('Ctrl Pts',(-9.13586688858169,-18.9169043053388,
0.));
#33485=CARTESIAN_POINT('Ctrl Pts',(-9.13586688858169,-18.9169043053388,
18.));
#33486=CARTESIAN_POINT('Ctrl Pts',(-9.13439956903533,-19.0006405223697,
0.));
#33487=CARTESIAN_POINT('Ctrl Pts',(-9.13439956903533,-19.0006405223697,
18.));
#33488=CARTESIAN_POINT('Ctrl Pts',(-9.13218114462419,-19.0845541036965,
0.));
#33489=CARTESIAN_POINT('Ctrl Pts',(-9.13218114462419,-19.0845541036965,
18.));
#33490=CARTESIAN_POINT('Ctrl Pts',(-9.12921984349375,-19.1686380639041,
0.));
#33491=CARTESIAN_POINT('Ctrl Pts',(-9.12921984349375,-19.1686380639041,
18.));
#33492=CARTESIAN_POINT('Ctrl Pts',(-9.125526627856,-19.2528843844341,0.));
#33493=CARTESIAN_POINT('Ctrl Pts',(-9.125526627856,-19.2528843844341,18.));
#33494=CARTESIAN_POINT('Ctrl Pts',(-9.121113479412,-19.3372847008483,0.));
#33495=CARTESIAN_POINT('Ctrl Pts',(-9.121113479412,-19.3372847008483,18.));
#33496=CARTESIAN_POINT('Ctrl Pts',(-9.1159915924392,-19.4218310275711,0.));
#33497=CARTESIAN_POINT('Ctrl Pts',(-9.1159915924392,-19.4218310275711,18.));
#33498=CARTESIAN_POINT('Ctrl Pts',(-9.11016929611336,-19.5065165934577,
0.));
#33499=CARTESIAN_POINT('Ctrl Pts',(-9.11016929611336,-19.5065165934577,
18.));
#33500=CARTESIAN_POINT('Ctrl Pts',(-9.10365235736465,-19.5913357132276,
0.));
#33501=CARTESIAN_POINT('Ctrl Pts',(-9.10365235736465,-19.5913357132276,
18.));
#33502=CARTESIAN_POINT('Ctrl Pts',(-9.0964449428387,-19.6762833927168,0.));
#33503=CARTESIAN_POINT('Ctrl Pts',(-9.0964449428387,-19.6762833927168,18.));
#33504=CARTESIAN_POINT('Ctrl Pts',(-9.08855038355402,-19.7613550146978,
0.));
#33505=CARTESIAN_POINT('Ctrl Pts',(-9.08855038355402,-19.7613550146978,
18.));
#33506=CARTESIAN_POINT('Ctrl Pts',(-9.07997196979668,-19.846546013708,0.));
#33507=CARTESIAN_POINT('Ctrl Pts',(-9.07997196979668,-19.846546013708,18.));
#33508=CARTESIAN_POINT('Ctrl Pts',(-9.0707138821585,-19.9318514954605,0.));
#33509=CARTESIAN_POINT('Ctrl Pts',(-9.0707138821585,-19.9318514954605,18.));
#33510=CARTESIAN_POINT('Ctrl Pts',(-9.0607810967537,-20.0172662790811,0.));
#33511=CARTESIAN_POINT('Ctrl Pts',(-9.0607810967537,-20.0172662790811,18.));
#33512=CARTESIAN_POINT('Ctrl Pts',(-9.05017898090711,-20.1027850670435,
0.));
#33513=CARTESIAN_POINT('Ctrl Pts',(-9.05017898090711,-20.1027850670435,
18.));
#33514=CARTESIAN_POINT('Ctrl Pts',(-9.03891298737032,-20.1884025764493,
0.));
#33515=CARTESIAN_POINT('Ctrl Pts',(-9.03891298737032,-20.1884025764493,
18.));
#33516=CARTESIAN_POINT('Ctrl Pts',(-9.02698833758324,-20.2741136736186,
0.));
#33517=CARTESIAN_POINT('Ctrl Pts',(-9.02698833758324,-20.2741136736186,
18.));
#33518=CARTESIAN_POINT('Ctrl Pts',(-9.01440965049155,-20.3599135373691,
0.));
#33519=CARTESIAN_POINT('Ctrl Pts',(-9.01440965049155,-20.3599135373691,
18.));
#33520=CARTESIAN_POINT('Ctrl Pts',(-9.00118097039517,-20.4457976315472,
0.));
#33521=CARTESIAN_POINT('Ctrl Pts',(-9.00118097039517,-20.4457976315472,
18.));
#33522=CARTESIAN_POINT('Ctrl Pts',(-8.98730595457659,-20.5317616031369,
0.));
#33523=CARTESIAN_POINT('Ctrl Pts',(-8.98730595457659,-20.5317616031369,
18.));
#33524=CARTESIAN_POINT('Ctrl Pts',(-8.97278801890468,-20.6178012000199,
0.));
#33525=CARTESIAN_POINT('Ctrl Pts',(-8.97278801890468,-20.6178012000199,
18.));
#33526=CARTESIAN_POINT('Ctrl Pts',(-8.95763049112623,-20.7039121898975,
0.));
#33527=CARTESIAN_POINT('Ctrl Pts',(-8.95763049112623,-20.7039121898975,
18.));
#33528=CARTESIAN_POINT('Ctrl Pts',(-8.94183680111377,-20.7900902537083,
0.));
#33529=CARTESIAN_POINT('Ctrl Pts',(-8.94183680111377,-20.7900902537083,
18.));
#33530=CARTESIAN_POINT('Ctrl Pts',(-8.92541048738649,-20.8763310073304,
0.));
#33531=CARTESIAN_POINT('Ctrl Pts',(-8.92541048738649,-20.8763310073304,
18.));
#33532=CARTESIAN_POINT('Ctrl Pts',(-8.90835509843285,-20.9626300944902,
0.));
#33533=CARTESIAN_POINT('Ctrl Pts',(-8.90835509843285,-20.9626300944902,
18.));
#33534=CARTESIAN_POINT('Ctrl Pts',(-8.89067412773386,-21.0489832630915,
0.));
#33535=CARTESIAN_POINT('Ctrl Pts',(-8.89067412773386,-21.0489832630915,
18.));
#33536=CARTESIAN_POINT('Ctrl Pts',(-8.87237094640749,-21.1353864352374,
0.));
#33537=CARTESIAN_POINT('Ctrl Pts',(-8.87237094640749,-21.1353864352374,
18.));
#33538=CARTESIAN_POINT('Ctrl Pts',(-8.85344872418156,-21.2218358113425,
0.));
#33539=CARTESIAN_POINT('Ctrl Pts',(-8.85344872418156,-21.2218358113425,
18.));
#33540=CARTESIAN_POINT('Ctrl Pts',(-8.83391042911629,-21.3083278326642,
0.));
#33541=CARTESIAN_POINT('Ctrl Pts',(-8.83391042911629,-21.3083278326642,
18.));
#33542=CARTESIAN_POINT('Ctrl Pts',(-8.81375890120582,-21.3948590173441,
0.));
#33543=CARTESIAN_POINT('Ctrl Pts',(-8.81375890120582,-21.3948590173441,
18.));
#33544=CARTESIAN_POINT('Ctrl Pts',(-8.79299691277858,-21.481425822209,0.));
#33545=CARTESIAN_POINT('Ctrl Pts',(-8.79299691277858,-21.481425822209,18.));
#33546=CARTESIAN_POINT('Ctrl Pts',(-8.77162723103299,-21.5680245138584,
0.));
#33547=CARTESIAN_POINT('Ctrl Pts',(-8.77162723103299,-21.5680245138584,
18.));
#33548=CARTESIAN_POINT('Ctrl Pts',(-8.74965270266163,-21.6546509866725,
0.));
#33549=CARTESIAN_POINT('Ctrl Pts',(-8.74965270266163,-21.6546509866725,
18.));
#33550=CARTESIAN_POINT('Ctrl Pts',(-8.72707626956922,-21.7413007707864,
0.));
#33551=CARTESIAN_POINT('Ctrl Pts',(-8.72707626956922,-21.7413007707864,
18.));
#33552=CARTESIAN_POINT('Ctrl Pts',(-8.70390086252203,-21.8279693631274,
0.));
#33553=CARTESIAN_POINT('Ctrl Pts',(-8.70390086252203,-21.8279693631274,
18.));
#33554=CARTESIAN_POINT('Ctrl Pts',(-8.68012932645739,-21.9146524902336,
0.));
#33555=CARTESIAN_POINT('Ctrl Pts',(-8.68012932645739,-21.9146524902336,
18.));
#33556=CARTESIAN_POINT('Ctrl Pts',(-8.6557643376698,-22.0013463859623,0.));
#33557=CARTESIAN_POINT('Ctrl Pts',(-8.6557643376698,-22.0013463859623,18.));
#33558=CARTESIAN_POINT('Ctrl Pts',(-8.63080832792612,-22.0880480931906,
0.));
#33559=CARTESIAN_POINT('Ctrl Pts',(-8.63080832792612,-22.0880480931906,
18.));
#33560=CARTESIAN_POINT('Ctrl Pts',(-8.60526341207614,-22.1747556651024,
0.));
#33561=CARTESIAN_POINT('Ctrl Pts',(-8.60526341207614,-22.1747556651024,
18.));
#33562=CARTESIAN_POINT('Ctrl Pts',(-8.57913133085326,-22.2614679221213,
0.));
#33563=CARTESIAN_POINT('Ctrl Pts',(-8.57913133085326,-22.2614679221213,
18.));
#33564=CARTESIAN_POINT('Ctrl Pts',(-8.55775698160722,-22.3308410047044,
0.));
#33565=CARTESIAN_POINT('Ctrl Pts',(-8.55775698160722,-22.3308410047044,
18.));
#33566=CARTESIAN_POINT('Ctrl Pts',(-8.54146295656907,-22.3828725698612,
0.));
#33567=CARTESIAN_POINT('Ctrl Pts',(-8.54146295656907,-22.3828725698612,
18.));
#33568=CARTESIAN_POINT('Ctrl Pts',(-8.53048330625155,-22.4175610589877,
0.));
#33569=CARTESIAN_POINT('Ctrl Pts',(-8.53048330625155,-22.4175610589877,
18.));
#33570=CARTESIAN_POINT('Ctrl Pts',(-8.52496423935285,-22.4349054983023,
0.));
#33571=CARTESIAN_POINT('Ctrl Pts',(-8.52496423935285,-22.4349054983023,
18.));
#33572=CARTESIAN_POINT('Ctrl Pts',(-8.7808540919664,-16.6164222996225,0.));
#33573=CARTESIAN_POINT('Ctrl Pts',(-8.78817964150686,-16.6302847808193,
0.));
#33574=CARTESIAN_POINT('Ctrl Pts',(-8.80233481798951,-16.6582257921024,
0.));
#33575=CARTESIAN_POINT('Ctrl Pts',(-8.82207984677447,-16.7007854423938,
0.));
#33576=CARTESIAN_POINT('Ctrl Pts',(-8.84558256033742,-16.7587634618101,
0.));
#33577=CARTESIAN_POINT('Ctrl Pts',(-8.87112909692392,-16.8329157811062,
0.));
#33578=CARTESIAN_POINT('Ctrl Pts',(-8.89394614661329,-16.908275670167,0.));
#33579=CARTESIAN_POINT('Ctrl Pts',(-8.91510993758933,-16.9843788566346,
0.));
#33580=CARTESIAN_POINT('Ctrl Pts',(-8.93538377395244,-17.0608897634975,
0.));
#33581=CARTESIAN_POINT('Ctrl Pts',(-8.95502702208204,-17.1376822726252,
0.));
#33582=CARTESIAN_POINT('Ctrl Pts',(-8.97397941759265,-17.2147637614528,
0.));
#33583=CARTESIAN_POINT('Ctrl Pts',(-8.99199362652257,-17.2922207948279,
0.));
#33584=CARTESIAN_POINT('Ctrl Pts',(-9.00877780436037,-17.3701605263553,
0.));
#33585=CARTESIAN_POINT('Ctrl Pts',(-9.0241575097608,-17.4486443043185,0.));
#33586=CARTESIAN_POINT('Ctrl Pts',(-9.03814678971601,-17.5276582702181,
0.));
#33587=CARTESIAN_POINT('Ctrl Pts',(-9.05086524971401,-17.6071467783263,
0.));
#33588=CARTESIAN_POINT('Ctrl Pts',(-9.06248904941395,-17.6870319618808,
0.));
#33589=CARTESIAN_POINT('Ctrl Pts',(-9.07319314215027,-17.7672369091005,
0.));
#33590=CARTESIAN_POINT('Ctrl Pts',(-9.08308548608349,-17.8477120247758,
0.));
#33591=CARTESIAN_POINT('Ctrl Pts',(-9.09219303320079,-17.9284406141976,
0.));
#33592=CARTESIAN_POINT('Ctrl Pts',(-9.10049631917583,-18.0094249416472,
0.));
#33593=CARTESIAN_POINT('Ctrl Pts',(-9.10795114540259,-18.0906774757189,
0.));
#33594=CARTESIAN_POINT('Ctrl Pts',(-9.1145134759054,-18.1722108451637,0.));
#33595=CARTESIAN_POINT('Ctrl Pts',(-9.12016808144599,-18.2540262849075,
0.));
#33596=CARTESIAN_POINT('Ctrl Pts',(-9.12493031448672,-18.3361129010289,
0.));
#33597=CARTESIAN_POINT('Ctrl Pts',(-9.12883240135631,-18.4184531695731,
0.));
#33598=CARTESIAN_POINT('Ctrl Pts',(-9.13191425549883,-18.5010266156389,
0.));
#33599=CARTESIAN_POINT('Ctrl Pts',(-9.13421321934922,-18.5838139250423,
0.));
#33600=CARTESIAN_POINT('Ctrl Pts',(-9.13575227582419,-18.6668016710749,
0.));
#33601=CARTESIAN_POINT('Ctrl Pts',(-9.13654074021147,-18.7499820263476,
0.));
#33602=CARTESIAN_POINT('Ctrl Pts',(-9.13657985367154,-18.8333505052874,
0.));
#33603=CARTESIAN_POINT('Ctrl Pts',(-9.13586688858169,-18.9169043053388,
0.));
#33604=CARTESIAN_POINT('Ctrl Pts',(-9.13439956903533,-19.0006405223697,
0.));
#33605=CARTESIAN_POINT('Ctrl Pts',(-9.13218114462419,-19.0845541036965,
0.));
#33606=CARTESIAN_POINT('Ctrl Pts',(-9.12921984349375,-19.1686380639041,
0.));
#33607=CARTESIAN_POINT('Ctrl Pts',(-9.125526627856,-19.2528843844341,0.));
#33608=CARTESIAN_POINT('Ctrl Pts',(-9.121113479412,-19.3372847008483,0.));
#33609=CARTESIAN_POINT('Ctrl Pts',(-9.1159915924392,-19.4218310275711,0.));
#33610=CARTESIAN_POINT('Ctrl Pts',(-9.11016929611336,-19.5065165934577,
0.));
#33611=CARTESIAN_POINT('Ctrl Pts',(-9.10365235736465,-19.5913357132276,
0.));
#33612=CARTESIAN_POINT('Ctrl Pts',(-9.0964449428387,-19.6762833927168,0.));
#33613=CARTESIAN_POINT('Ctrl Pts',(-9.08855038355402,-19.7613550146978,
0.));
#33614=CARTESIAN_POINT('Ctrl Pts',(-9.07997196979668,-19.846546013708,0.));
#33615=CARTESIAN_POINT('Ctrl Pts',(-9.0707138821585,-19.9318514954605,0.));
#33616=CARTESIAN_POINT('Ctrl Pts',(-9.0607810967537,-20.0172662790811,0.));
#33617=CARTESIAN_POINT('Ctrl Pts',(-9.05017898090711,-20.1027850670435,
0.));
#33618=CARTESIAN_POINT('Ctrl Pts',(-9.03891298737032,-20.1884025764493,
0.));
#33619=CARTESIAN_POINT('Ctrl Pts',(-9.02698833758324,-20.2741136736186,
0.));
#33620=CARTESIAN_POINT('Ctrl Pts',(-9.01440965049155,-20.3599135373691,
0.));
#33621=CARTESIAN_POINT('Ctrl Pts',(-9.00118097039517,-20.4457976315472,
0.));
#33622=CARTESIAN_POINT('Ctrl Pts',(-8.98730595457659,-20.5317616031369,
0.));
#33623=CARTESIAN_POINT('Ctrl Pts',(-8.97278801890468,-20.6178012000199,
0.));
#33624=CARTESIAN_POINT('Ctrl Pts',(-8.95763049112623,-20.7039121898975,
0.));
#33625=CARTESIAN_POINT('Ctrl Pts',(-8.94183680111377,-20.7900902537083,
0.));
#33626=CARTESIAN_POINT('Ctrl Pts',(-8.92541048738649,-20.8763310073304,
0.));
#33627=CARTESIAN_POINT('Ctrl Pts',(-8.90835509843285,-20.9626300944902,
0.));
#33628=CARTESIAN_POINT('Ctrl Pts',(-8.89067412773386,-21.0489832630915,
0.));
#33629=CARTESIAN_POINT('Ctrl Pts',(-8.87237094640749,-21.1353864352374,
0.));
#33630=CARTESIAN_POINT('Ctrl Pts',(-8.85344872418156,-21.2218358113425,
0.));
#33631=CARTESIAN_POINT('Ctrl Pts',(-8.83391042911629,-21.3083278326642,
0.));
#33632=CARTESIAN_POINT('Ctrl Pts',(-8.81375890120582,-21.3948590173441,
0.));
#33633=CARTESIAN_POINT('Ctrl Pts',(-8.79299691277858,-21.481425822209,0.));
#33634=CARTESIAN_POINT('Ctrl Pts',(-8.77162723103299,-21.5680245138584,
0.));
#33635=CARTESIAN_POINT('Ctrl Pts',(-8.74965270266163,-21.6546509866725,
0.));
#33636=CARTESIAN_POINT('Ctrl Pts',(-8.72707626956922,-21.7413007707864,
0.));
#33637=CARTESIAN_POINT('Ctrl Pts',(-8.70390086252203,-21.8279693631274,
0.));
#33638=CARTESIAN_POINT('Ctrl Pts',(-8.68012932645739,-21.9146524902336,
0.));
#33639=CARTESIAN_POINT('Ctrl Pts',(-8.6557643376698,-22.0013463859623,0.));
#33640=CARTESIAN_POINT('Ctrl Pts',(-8.63080832792612,-22.0880480931906,
0.));
#33641=CARTESIAN_POINT('Ctrl Pts',(-8.60015442890614,-22.1920971794848,
0.));
#33642=CARTESIAN_POINT('Ctrl Pts',(-8.57387555634004,-22.2788106077804,
0.));
#33643=CARTESIAN_POINT('Ctrl Pts',(-8.55238412336295,-22.3481844703457,
0.));
#33644=CARTESIAN_POINT('Ctrl Pts',(-8.53600237317213,-22.4002166196189,
0.));
#33645=CARTESIAN_POINT('Ctrl Pts',(-8.52496423935285,-22.4349054983023,
0.));
#33646=CARTESIAN_POINT('Ctrl Pts',(-8.7808540919664,-16.6164222996225,15.));
#33647=CARTESIAN_POINT('Ctrl Pts',(-8.78817964150686,-16.6302847808193,
15.));
#33648=CARTESIAN_POINT('Ctrl Pts',(-8.80233481798951,-16.6582257921024,
15.));
#33649=CARTESIAN_POINT('Ctrl Pts',(-8.82207984677447,-16.7007854423938,
15.));
#33650=CARTESIAN_POINT('Ctrl Pts',(-8.84558256033742,-16.7587634618101,
15.));
#33651=CARTESIAN_POINT('Ctrl Pts',(-8.87112909692392,-16.8329157811062,
15.));
#33652=CARTESIAN_POINT('Ctrl Pts',(-8.89394614661329,-16.908275670167,15.));
#33653=CARTESIAN_POINT('Ctrl Pts',(-8.91510993758933,-16.9843788566346,
15.));
#33654=CARTESIAN_POINT('Ctrl Pts',(-8.93538377395244,-17.0608897634975,
15.));
#33655=CARTESIAN_POINT('Ctrl Pts',(-8.95502702208204,-17.1376822726252,
15.));
#33656=CARTESIAN_POINT('Ctrl Pts',(-8.97397941759265,-17.2147637614528,
15.));
#33657=CARTESIAN_POINT('Ctrl Pts',(-8.99199362652257,-17.2922207948279,
15.));
#33658=CARTESIAN_POINT('Ctrl Pts',(-9.00877780436037,-17.3701605263553,
15.));
#33659=CARTESIAN_POINT('Ctrl Pts',(-9.0241575097608,-17.4486443043185,15.));
#33660=CARTESIAN_POINT('Ctrl Pts',(-9.03814678971601,-17.5276582702181,
15.));
#33661=CARTESIAN_POINT('Ctrl Pts',(-9.05086524971401,-17.6071467783263,
15.));
#33662=CARTESIAN_POINT('Ctrl Pts',(-9.06248904941395,-17.6870319618808,
15.));
#33663=CARTESIAN_POINT('Ctrl Pts',(-9.07319314215027,-17.7672369091005,
15.));
#33664=CARTESIAN_POINT('Ctrl Pts',(-9.08308548608349,-17.8477120247758,
15.));
#33665=CARTESIAN_POINT('Ctrl Pts',(-9.09219303320079,-17.9284406141976,
15.));
#33666=CARTESIAN_POINT('Ctrl Pts',(-9.10049631917583,-18.0094249416472,
15.));
#33667=CARTESIAN_POINT('Ctrl Pts',(-9.10795114540259,-18.0906774757189,
15.));
#33668=CARTESIAN_POINT('Ctrl Pts',(-9.1145134759054,-18.1722108451637,15.));
#33669=CARTESIAN_POINT('Ctrl Pts',(-9.12016808144599,-18.2540262849075,
15.));
#33670=CARTESIAN_POINT('Ctrl Pts',(-9.12493031448672,-18.3361129010289,
15.));
#33671=CARTESIAN_POINT('Ctrl Pts',(-9.12883240135631,-18.4184531695731,
15.));
#33672=CARTESIAN_POINT('Ctrl Pts',(-9.13191425549883,-18.5010266156389,
15.));
#33673=CARTESIAN_POINT('Ctrl Pts',(-9.13421321934922,-18.5838139250423,
15.));
#33674=CARTESIAN_POINT('Ctrl Pts',(-9.13575227582419,-18.6668016710749,
15.));
#33675=CARTESIAN_POINT('Ctrl Pts',(-9.13654074021147,-18.7499820263476,
15.));
#33676=CARTESIAN_POINT('Ctrl Pts',(-9.13657985367154,-18.8333505052874,
15.));
#33677=CARTESIAN_POINT('Ctrl Pts',(-9.13586688858169,-18.9169043053388,
15.));
#33678=CARTESIAN_POINT('Ctrl Pts',(-9.13439956903533,-19.0006405223697,
15.));
#33679=CARTESIAN_POINT('Ctrl Pts',(-9.13218114462419,-19.0845541036965,
15.));
#33680=CARTESIAN_POINT('Ctrl Pts',(-9.12921984349375,-19.1686380639041,
15.));
#33681=CARTESIAN_POINT('Ctrl Pts',(-9.125526627856,-19.2528843844341,15.));
#33682=CARTESIAN_POINT('Ctrl Pts',(-9.121113479412,-19.3372847008483,15.));
#33683=CARTESIAN_POINT('Ctrl Pts',(-9.1159915924392,-19.4218310275711,15.));
#33684=CARTESIAN_POINT('Ctrl Pts',(-9.11016929611336,-19.5065165934577,
15.));
#33685=CARTESIAN_POINT('Ctrl Pts',(-9.10365235736465,-19.5913357132276,
15.));
#33686=CARTESIAN_POINT('Ctrl Pts',(-9.0964449428387,-19.6762833927168,15.));
#33687=CARTESIAN_POINT('Ctrl Pts',(-9.08855038355402,-19.7613550146978,
15.));
#33688=CARTESIAN_POINT('Ctrl Pts',(-9.07997196979668,-19.846546013708,15.));
#33689=CARTESIAN_POINT('Ctrl Pts',(-9.0707138821585,-19.9318514954605,15.));
#33690=CARTESIAN_POINT('Ctrl Pts',(-9.0607810967537,-20.0172662790811,15.));
#33691=CARTESIAN_POINT('Ctrl Pts',(-9.05017898090711,-20.1027850670435,
15.));
#33692=CARTESIAN_POINT('Ctrl Pts',(-9.03891298737032,-20.1884025764493,
15.));
#33693=CARTESIAN_POINT('Ctrl Pts',(-9.02698833758324,-20.2741136736186,
15.));
#33694=CARTESIAN_POINT('Ctrl Pts',(-9.01440965049155,-20.3599135373691,
15.));
#33695=CARTESIAN_POINT('Ctrl Pts',(-9.00118097039517,-20.4457976315472,
15.));
#33696=CARTESIAN_POINT('Ctrl Pts',(-8.98730595457659,-20.5317616031369,
15.));
#33697=CARTESIAN_POINT('Ctrl Pts',(-8.97278801890468,-20.6178012000199,
15.));
#33698=CARTESIAN_POINT('Ctrl Pts',(-8.95763049112623,-20.7039121898975,
15.));
#33699=CARTESIAN_POINT('Ctrl Pts',(-8.94183680111377,-20.7900902537083,
15.));
#33700=CARTESIAN_POINT('Ctrl Pts',(-8.92541048738649,-20.8763310073304,
15.));
#33701=CARTESIAN_POINT('Ctrl Pts',(-8.90835509843285,-20.9626300944902,
15.));
#33702=CARTESIAN_POINT('Ctrl Pts',(-8.89067412773386,-21.0489832630915,
15.));
#33703=CARTESIAN_POINT('Ctrl Pts',(-8.87237094640749,-21.1353864352374,
15.));
#33704=CARTESIAN_POINT('Ctrl Pts',(-8.85344872418156,-21.2218358113425,
15.));
#33705=CARTESIAN_POINT('Ctrl Pts',(-8.83391042911629,-21.3083278326642,
15.));
#33706=CARTESIAN_POINT('Ctrl Pts',(-8.81375890120582,-21.3948590173441,
15.));
#33707=CARTESIAN_POINT('Ctrl Pts',(-8.79299691277858,-21.481425822209,15.));
#33708=CARTESIAN_POINT('Ctrl Pts',(-8.77162723103299,-21.5680245138584,
15.));
#33709=CARTESIAN_POINT('Ctrl Pts',(-8.74965270266163,-21.6546509866725,
15.));
#33710=CARTESIAN_POINT('Ctrl Pts',(-8.72707626956922,-21.7413007707864,
15.));
#33711=CARTESIAN_POINT('Ctrl Pts',(-8.70390086252203,-21.8279693631274,
15.));
#33712=CARTESIAN_POINT('Ctrl Pts',(-8.68012932645739,-21.9146524902336,
15.));
#33713=CARTESIAN_POINT('Ctrl Pts',(-8.6557643376698,-22.0013463859623,15.));
#33714=CARTESIAN_POINT('Ctrl Pts',(-8.63080832792612,-22.0880480931906,
15.));
#33715=CARTESIAN_POINT('Ctrl Pts',(-8.60015442890614,-22.1920971794848,
15.));
#33716=CARTESIAN_POINT('Ctrl Pts',(-8.57387555634004,-22.2788106077804,
15.));
#33717=CARTESIAN_POINT('Ctrl Pts',(-8.55238412336295,-22.3481844703457,
15.));
#33718=CARTESIAN_POINT('Ctrl Pts',(-8.53600237317213,-22.4002166196189,
15.));
#33719=CARTESIAN_POINT('Ctrl Pts',(-8.52496423935285,-22.4349054983023,
15.));
#33720=CARTESIAN_POINT('Ctrl Pts',(-18.7025042402277,-15.040489857191,0.));
#33721=CARTESIAN_POINT('Ctrl Pts',(-18.7025042402277,-15.040489857191,18.));
#33722=CARTESIAN_POINT('Ctrl Pts',(-18.6843032127312,-15.0403790752228,
0.));
#33723=CARTESIAN_POINT('Ctrl Pts',(-18.6843032127312,-15.0403790752228,
18.));
#33724=CARTESIAN_POINT('Ctrl Pts',(-18.6479196005666,-15.0401020105546,
0.));
#33725=CARTESIAN_POINT('Ctrl Pts',(-18.6479196005666,-15.0401020105546,
18.));
#33726=CARTESIAN_POINT('Ctrl Pts',(-18.5933995108277,-15.0395199113665,
0.));
#33727=CARTESIAN_POINT('Ctrl Pts',(-18.5933995108277,-15.0395199113665,
18.));
#33728=CARTESIAN_POINT('Ctrl Pts',(-18.5208167514208,-15.0384106640281,
0.));
#33729=CARTESIAN_POINT('Ctrl Pts',(-18.5208167514208,-15.0384106640281,
18.));
#33730=CARTESIAN_POINT('Ctrl Pts',(-18.4302732371441,-15.0364681891201,
0.));
#33731=CARTESIAN_POINT('Ctrl Pts',(-18.4302732371441,-15.0364681891201,
18.));
#33732=CARTESIAN_POINT('Ctrl Pts',(-18.3399156227477,-15.0339687345357,
0.));
#33733=CARTESIAN_POINT('Ctrl Pts',(-18.3399156227477,-15.0339687345357,
18.));
#33734=CARTESIAN_POINT('Ctrl Pts',(-18.2497455679917,-15.0309110092482,
0.));
#33735=CARTESIAN_POINT('Ctrl Pts',(-18.2497455679917,-15.0309110092482,
18.));
#33736=CARTESIAN_POINT('Ctrl Pts',(-18.1597655779328,-15.0272936035154,
0.));
#33737=CARTESIAN_POINT('Ctrl Pts',(-18.1597655779328,-15.0272936035154,
18.));
#33738=CARTESIAN_POINT('Ctrl Pts',(-18.0699792164192,-15.0231151183906,
0.));
#33739=CARTESIAN_POINT('Ctrl Pts',(-18.0699792164192,-15.0231151183906,
18.));
#33740=CARTESIAN_POINT('Ctrl Pts',(-17.980390892286,-15.0183741723687,0.));
#33741=CARTESIAN_POINT('Ctrl Pts',(-17.980390892286,-15.0183741723687,18.));
#33742=CARTESIAN_POINT('Ctrl Pts',(-17.891005548971,-15.0130693803259,0.));
#33743=CARTESIAN_POINT('Ctrl Pts',(-17.891005548971,-15.0130693803259,18.));
#33744=CARTESIAN_POINT('Ctrl Pts',(-17.8018283748074,-15.0071993464636,
0.));
#33745=CARTESIAN_POINT('Ctrl Pts',(-17.8018283748074,-15.0071993464636,
18.));
#33746=CARTESIAN_POINT('Ctrl Pts',(-17.7128645299878,-15.0007626541286,
0.));
#33747=CARTESIAN_POINT('Ctrl Pts',(-17.7128645299878,-15.0007626541286,
18.));
#33748=CARTESIAN_POINT('Ctrl Pts',(-17.6241187988652,-14.9937578646616,
0.));
#33749=CARTESIAN_POINT('Ctrl Pts',(-17.6241187988652,-14.9937578646616,
18.));
#33750=CARTESIAN_POINT('Ctrl Pts',(-17.5355955872257,-14.9861834999847,
0.));
#33751=CARTESIAN_POINT('Ctrl Pts',(-17.5355955872257,-14.9861834999847,
18.));
#33752=CARTESIAN_POINT('Ctrl Pts',(-17.4472991215239,-14.9780380183576,
0.));
#33753=CARTESIAN_POINT('Ctrl Pts',(-17.4472991215239,-14.9780380183576,
18.));
#33754=CARTESIAN_POINT('Ctrl Pts',(-17.3592335908103,-14.9693197947387,
0.));
#33755=CARTESIAN_POINT('Ctrl Pts',(-17.3592335908103,-14.9693197947387,
18.));
#33756=CARTESIAN_POINT('Ctrl Pts',(-17.2714032968314,-14.9600271060471,
0.));
#33757=CARTESIAN_POINT('Ctrl Pts',(-17.2714032968314,-14.9600271060471,
18.));
#33758=CARTESIAN_POINT('Ctrl Pts',(-17.1838128327073,-14.9501581118289,
0.));
#33759=CARTESIAN_POINT('Ctrl Pts',(-17.1838128327073,-14.9501581118289,
18.));
#33760=CARTESIAN_POINT('Ctrl Pts',(-17.0964671184813,-14.9397108660998,
0.));
#33761=CARTESIAN_POINT('Ctrl Pts',(-17.0964671184813,-14.9397108660998,
18.));
#33762=CARTESIAN_POINT('Ctrl Pts',(-17.0093712776822,-14.9286833603319,
0.));
#33763=CARTESIAN_POINT('Ctrl Pts',(-17.0093712776822,-14.9286833603319,
18.));
#33764=CARTESIAN_POINT('Ctrl Pts',(-16.9225305499155,-14.9170735658747,
0.));
#33765=CARTESIAN_POINT('Ctrl Pts',(-16.9225305499155,-14.9170735658747,
18.));
#33766=CARTESIAN_POINT('Ctrl Pts',(-16.8359501981915,-14.9048794721647,
0.));
#33767=CARTESIAN_POINT('Ctrl Pts',(-16.8359501981915,-14.9048794721647,
18.));
#33768=CARTESIAN_POINT('Ctrl Pts',(-16.7496353900706,-14.8920991518626,
0.));
#33769=CARTESIAN_POINT('Ctrl Pts',(-16.7496353900706,-14.8920991518626,
18.));
#33770=CARTESIAN_POINT('Ctrl Pts',(-16.6635911790385,-14.8787307479454,
0.));
#33771=CARTESIAN_POINT('Ctrl Pts',(-16.6635911790385,-14.8787307479454,
18.));
#33772=CARTESIAN_POINT('Ctrl Pts',(-16.5778226646614,-14.8647723257055,
0.));
#33773=CARTESIAN_POINT('Ctrl Pts',(-16.5778226646614,-14.8647723257055,
18.));
#33774=CARTESIAN_POINT('Ctrl Pts',(-16.492335117066,-14.8502217520165,0.));
#33775=CARTESIAN_POINT('Ctrl Pts',(-16.492335117066,-14.8502217520165,18.));
#33776=CARTESIAN_POINT('Ctrl Pts',(-16.4071341001481,-14.8350765822692,
0.));
#33777=CARTESIAN_POINT('Ctrl Pts',(-16.4071341001481,-14.8350765822692,
18.));
#33778=CARTESIAN_POINT('Ctrl Pts',(-16.3222256264574,-14.8193339134125,
0.));
#33779=CARTESIAN_POINT('Ctrl Pts',(-16.3222256264574,-14.8193339134125,
18.));
#33780=CARTESIAN_POINT('Ctrl Pts',(-16.2376161919272,-14.8029903659562,
0.));
#33781=CARTESIAN_POINT('Ctrl Pts',(-16.2376161919272,-14.8029903659562,
18.));
#33782=CARTESIAN_POINT('Ctrl Pts',(-16.1533125058853,-14.7860423865308,
0.));
#33783=CARTESIAN_POINT('Ctrl Pts',(-16.1533125058853,-14.7860423865308,
18.));
#33784=CARTESIAN_POINT('Ctrl Pts',(-16.0693212651732,-14.7684865075326,
0.));
#33785=CARTESIAN_POINT('Ctrl Pts',(-16.0693212651732,-14.7684865075326,
18.));
#33786=CARTESIAN_POINT('Ctrl Pts',(-15.9856489347991,-14.7503195973741,
0.));
#33787=CARTESIAN_POINT('Ctrl Pts',(-15.9856489347991,-14.7503195973741,
18.));
#33788=CARTESIAN_POINT('Ctrl Pts',(-15.9023014613802,-14.7315391924939,
0.));
#33789=CARTESIAN_POINT('Ctrl Pts',(-15.9023014613802,-14.7315391924939,
18.));
#33790=CARTESIAN_POINT('Ctrl Pts',(-15.8192842036838,-14.7121435744495,
0.));
#33791=CARTESIAN_POINT('Ctrl Pts',(-15.8192842036838,-14.7121435744495,
18.));
#33792=CARTESIAN_POINT('Ctrl Pts',(-15.7366025822956,-14.692131002056,0.));
#33793=CARTESIAN_POINT('Ctrl Pts',(-15.7366025822956,-14.692131002056,18.));
#33794=CARTESIAN_POINT('Ctrl Pts',(-15.6542626345121,-14.6714990558793,
0.));
#33795=CARTESIAN_POINT('Ctrl Pts',(-15.6542626345121,-14.6714990558793,
18.));
#33796=CARTESIAN_POINT('Ctrl Pts',(-15.5722715494357,-14.6502440080911,
0.));
#33797=CARTESIAN_POINT('Ctrl Pts',(-15.5722715494357,-14.6502440080911,
18.));
#33798=CARTESIAN_POINT('Ctrl Pts',(-15.4906383406647,-14.6283600295736,
0.));
#33799=CARTESIAN_POINT('Ctrl Pts',(-15.4906383406647,-14.6283600295736,
18.));
#33800=CARTESIAN_POINT('Ctrl Pts',(-15.4093740621548,-14.6058389416146,
0.));
#33801=CARTESIAN_POINT('Ctrl Pts',(-15.4093740621548,-14.6058389416146,
18.));
#33802=CARTESIAN_POINT('Ctrl Pts',(-15.3284903715086,-14.5826719336929,
0.));
#33803=CARTESIAN_POINT('Ctrl Pts',(-15.3284903715086,-14.5826719336929,
18.));
#33804=CARTESIAN_POINT('Ctrl Pts',(-15.2479982823383,-14.5588510579962,
0.));
#33805=CARTESIAN_POINT('Ctrl Pts',(-15.2479982823383,-14.5588510579962,
18.));
#33806=CARTESIAN_POINT('Ctrl Pts',(-15.1679069808052,-14.534370647705,0.));
#33807=CARTESIAN_POINT('Ctrl Pts',(-15.1679069808052,-14.534370647705,18.));
#33808=CARTESIAN_POINT('Ctrl Pts',(-15.0882222764759,-14.5092291736391,
0.));
#33809=CARTESIAN_POINT('Ctrl Pts',(-15.0882222764759,-14.5092291736391,
18.));
#33810=CARTESIAN_POINT('Ctrl Pts',(-15.0089462280505,-14.4834296977405,
0.));
#33811=CARTESIAN_POINT('Ctrl Pts',(-15.0089462280505,-14.4834296977405,
18.));
#33812=CARTESIAN_POINT('Ctrl Pts',(-14.9300806580357,-14.4569756801697,
0.));
#33813=CARTESIAN_POINT('Ctrl Pts',(-14.9300806580357,-14.4569756801697,
18.));
#33814=CARTESIAN_POINT('Ctrl Pts',(-14.8516302160049,-14.4298673266313,
0.));
#33815=CARTESIAN_POINT('Ctrl Pts',(-14.8516302160049,-14.4298673266313,
18.));
#33816=CARTESIAN_POINT('Ctrl Pts',(-14.7736052248294,-14.4020981965564,
0.));
#33817=CARTESIAN_POINT('Ctrl Pts',(-14.7736052248294,-14.4020981965564,
18.));
#33818=CARTESIAN_POINT('Ctrl Pts',(-14.6960255561799,-14.3736505809735,
0.));
#33819=CARTESIAN_POINT('Ctrl Pts',(-14.6960255561799,-14.3736505809735,
18.));
#33820=CARTESIAN_POINT('Ctrl Pts',(-14.6189211183837,-14.3444949335274,
0.));
#33821=CARTESIAN_POINT('Ctrl Pts',(-14.6189211183837,-14.3444949335274,
18.));
#33822=CARTESIAN_POINT('Ctrl Pts',(-14.5423237181615,-14.3145996213697,
0.));
#33823=CARTESIAN_POINT('Ctrl Pts',(-14.5423237181615,-14.3145996213697,
18.));
#33824=CARTESIAN_POINT('Ctrl Pts',(-14.4662599802682,-14.2839394106401,
0.));
#33825=CARTESIAN_POINT('Ctrl Pts',(-14.4662599802682,-14.2839394106401,
18.));
#33826=CARTESIAN_POINT('Ctrl Pts',(-14.3907450096103,-14.2525030666863,
0.));
#33827=CARTESIAN_POINT('Ctrl Pts',(-14.3907450096103,-14.2525030666863,
18.));
#33828=CARTESIAN_POINT('Ctrl Pts',(-14.3157729256101,-14.2203046917613,
0.));
#33829=CARTESIAN_POINT('Ctrl Pts',(-14.3157729256101,-14.2203046917613,
18.));
#33830=CARTESIAN_POINT('Ctrl Pts',(-14.2413181097468,-14.1873822640681,
0.));
#33831=CARTESIAN_POINT('Ctrl Pts',(-14.2413181097468,-14.1873822640681,
18.));
#33832=CARTESIAN_POINT('Ctrl Pts',(-14.1673550455622,-14.1537739659715,
0.));
#33833=CARTESIAN_POINT('Ctrl Pts',(-14.1673550455622,-14.1537739659715,
18.));
#33834=CARTESIAN_POINT('Ctrl Pts',(-14.0938755647891,-14.1194976094444,
0.));
#33835=CARTESIAN_POINT('Ctrl Pts',(-14.0938755647891,-14.1194976094444,
18.));
#33836=CARTESIAN_POINT('Ctrl Pts',(-14.0209038736616,-14.0845327205726,
0.));
#33837=CARTESIAN_POINT('Ctrl Pts',(-14.0209038736616,-14.0845327205726,
18.));
#33838=CARTESIAN_POINT('Ctrl Pts',(-13.9485205009332,-14.0487919508068,
0.));
#33839=CARTESIAN_POINT('Ctrl Pts',(-13.9485205009332,-14.0487919508068,
18.));
#33840=CARTESIAN_POINT('Ctrl Pts',(-13.876852657608,-14.0121326766855,0.));
#33841=CARTESIAN_POINT('Ctrl Pts',(-13.876852657608,-14.0121326766855,18.));
#33842=CARTESIAN_POINT('Ctrl Pts',(-13.806028835706,-13.9744114225699,0.));
#33843=CARTESIAN_POINT('Ctrl Pts',(-13.806028835706,-13.9744114225699,18.));
#33844=CARTESIAN_POINT('Ctrl Pts',(-13.7361389175879,-13.9355316323567,
0.));
#33845=CARTESIAN_POINT('Ctrl Pts',(-13.7361389175879,-13.9355316323567,
18.));
#33846=CARTESIAN_POINT('Ctrl Pts',(-13.6672004242289,-13.8954842290745,
0.));
#33847=CARTESIAN_POINT('Ctrl Pts',(-13.6672004242289,-13.8954842290745,
18.));
#33848=CARTESIAN_POINT('Ctrl Pts',(-13.5991011046042,-13.854416158639,0.));
#33849=CARTESIAN_POINT('Ctrl Pts',(-13.5991011046042,-13.854416158639,18.));
#33850=CARTESIAN_POINT('Ctrl Pts',(-13.5316488646659,-13.8125718693898,
0.));
#33851=CARTESIAN_POINT('Ctrl Pts',(-13.5316488646659,-13.8125718693898,
18.));
#33852=CARTESIAN_POINT('Ctrl Pts',(-13.4646849459541,-13.7701598398937,
0.));
#33853=CARTESIAN_POINT('Ctrl Pts',(-13.4646849459541,-13.7701598398937,
18.));
#33854=CARTESIAN_POINT('Ctrl Pts',(-13.3981837093919,-13.7272351052346,
0.));
#33855=CARTESIAN_POINT('Ctrl Pts',(-13.3981837093919,-13.7272351052346,
18.));
#33856=CARTESIAN_POINT('Ctrl Pts',(-13.332345249068,-13.6835899659728,0.));
#33857=CARTESIAN_POINT('Ctrl Pts',(-13.332345249068,-13.6835899659728,18.));
#33858=CARTESIAN_POINT('Ctrl Pts',(-13.267724591625,-13.6386021757691,0.));
#33859=CARTESIAN_POINT('Ctrl Pts',(-13.267724591625,-13.6386021757691,18.));
#33860=CARTESIAN_POINT('Ctrl Pts',(-13.2050958591127,-13.5913916488449,
0.));
#33861=CARTESIAN_POINT('Ctrl Pts',(-13.2050958591127,-13.5913916488449,
18.));
#33862=CARTESIAN_POINT('Ctrl Pts',(-13.1572182238498,-13.5511230466604,
0.));
#33863=CARTESIAN_POINT('Ctrl Pts',(-13.1572182238498,-13.5511230466604,
18.));
#33864=CARTESIAN_POINT('Ctrl Pts',(-13.1228431405579,-13.5191927531554,
0.));
#33865=CARTESIAN_POINT('Ctrl Pts',(-13.1228431405579,-13.5191927531554,
18.));
#33866=CARTESIAN_POINT('Ctrl Pts',(-13.1006438497967,-13.4970961329957,
0.));
#33867=CARTESIAN_POINT('Ctrl Pts',(-13.1006438497967,-13.4970961329957,
18.));
#33868=CARTESIAN_POINT('Ctrl Pts',(-13.0897235660237,-13.4858453790958,
0.));
#33869=CARTESIAN_POINT('Ctrl Pts',(-13.0897235660237,-13.4858453790958,
18.));
#33870=CARTESIAN_POINT('',(-18.7025042402277,-15.040489857191,0.));
#33871=CARTESIAN_POINT('Ctrl Pts',(-13.0897235660237,-13.4858453790958,
0.));
#33872=CARTESIAN_POINT('Ctrl Pts',(-13.1006438497967,-13.4970961329957,
0.));
#33873=CARTESIAN_POINT('Ctrl Pts',(-13.1228431405579,-13.5191927531554,
0.));
#33874=CARTESIAN_POINT('Ctrl Pts',(-13.1572182238498,-13.5511230466604,
0.));
#33875=CARTESIAN_POINT('Ctrl Pts',(-13.2050958591127,-13.5913916488449,
0.));
#33876=CARTESIAN_POINT('Ctrl Pts',(-13.267724591625,-13.6386021757691,0.));
#33877=CARTESIAN_POINT('Ctrl Pts',(-13.332345249068,-13.6835899659728,0.));
#33878=CARTESIAN_POINT('Ctrl Pts',(-13.3981837093919,-13.7272351052346,
0.));
#33879=CARTESIAN_POINT('Ctrl Pts',(-13.4646849459541,-13.7701598398937,
0.));
#33880=CARTESIAN_POINT('Ctrl Pts',(-13.5316488646659,-13.8125718693898,
0.));
#33881=CARTESIAN_POINT('Ctrl Pts',(-13.5991011046042,-13.854416158639,0.));
#33882=CARTESIAN_POINT('Ctrl Pts',(-13.6672004242289,-13.8954842290745,
0.));
#33883=CARTESIAN_POINT('Ctrl Pts',(-13.7361389175879,-13.9355316323567,
0.));
#33884=CARTESIAN_POINT('Ctrl Pts',(-13.806028835706,-13.9744114225699,0.));
#33885=CARTESIAN_POINT('Ctrl Pts',(-13.876852657608,-14.0121326766855,0.));
#33886=CARTESIAN_POINT('Ctrl Pts',(-13.9485205009332,-14.0487919508068,
0.));
#33887=CARTESIAN_POINT('Ctrl Pts',(-14.0209038736616,-14.0845327205726,
0.));
#33888=CARTESIAN_POINT('Ctrl Pts',(-14.0938755647891,-14.1194976094444,
0.));
#33889=CARTESIAN_POINT('Ctrl Pts',(-14.1673550455622,-14.1537739659715,
0.));
#33890=CARTESIAN_POINT('Ctrl Pts',(-14.2413181097468,-14.1873822640681,
0.));
#33891=CARTESIAN_POINT('Ctrl Pts',(-14.3157729256101,-14.2203046917613,
0.));
#33892=CARTESIAN_POINT('Ctrl Pts',(-14.3907450096103,-14.2525030666863,
0.));
#33893=CARTESIAN_POINT('Ctrl Pts',(-14.4662599802682,-14.2839394106401,
0.));
#33894=CARTESIAN_POINT('Ctrl Pts',(-14.5423237181615,-14.3145996213697,
0.));
#33895=CARTESIAN_POINT('Ctrl Pts',(-14.6189211183837,-14.3444949335274,
0.));
#33896=CARTESIAN_POINT('Ctrl Pts',(-14.6960255561799,-14.3736505809735,
0.));
#33897=CARTESIAN_POINT('Ctrl Pts',(-14.7736052248294,-14.4020981965564,
0.));
#33898=CARTESIAN_POINT('Ctrl Pts',(-14.8516302160049,-14.4298673266313,
0.));
#33899=CARTESIAN_POINT('Ctrl Pts',(-14.9300806580357,-14.4569756801697,
0.));
#33900=CARTESIAN_POINT('Ctrl Pts',(-15.0089462280505,-14.4834296977405,
0.));
#33901=CARTESIAN_POINT('Ctrl Pts',(-15.0882222764759,-14.5092291736391,
0.));
#33902=CARTESIAN_POINT('Ctrl Pts',(-15.1679069808052,-14.534370647705,0.));
#33903=CARTESIAN_POINT('Ctrl Pts',(-15.2479982823383,-14.5588510579962,
0.));
#33904=CARTESIAN_POINT('Ctrl Pts',(-15.3284903715086,-14.5826719336929,
0.));
#33905=CARTESIAN_POINT('Ctrl Pts',(-15.4093740621548,-14.6058389416146,
0.));
#33906=CARTESIAN_POINT('Ctrl Pts',(-15.4906383406647,-14.6283600295736,
0.));
#33907=CARTESIAN_POINT('Ctrl Pts',(-15.5722715494357,-14.6502440080911,
0.));
#33908=CARTESIAN_POINT('Ctrl Pts',(-15.6542626345121,-14.6714990558793,
0.));
#33909=CARTESIAN_POINT('Ctrl Pts',(-15.7366025822956,-14.692131002056,0.));
#33910=CARTESIAN_POINT('Ctrl Pts',(-15.8192842036838,-14.7121435744495,
0.));
#33911=CARTESIAN_POINT('Ctrl Pts',(-15.9023014613802,-14.7315391924939,
0.));
#33912=CARTESIAN_POINT('Ctrl Pts',(-15.9856489347991,-14.7503195973741,
0.));
#33913=CARTESIAN_POINT('Ctrl Pts',(-16.0693212651732,-14.7684865075326,
0.));
#33914=CARTESIAN_POINT('Ctrl Pts',(-16.1533125058853,-14.7860423865308,
0.));
#33915=CARTESIAN_POINT('Ctrl Pts',(-16.2376161919272,-14.8029903659562,
0.));
#33916=CARTESIAN_POINT('Ctrl Pts',(-16.3222256264574,-14.8193339134125,
0.));
#33917=CARTESIAN_POINT('Ctrl Pts',(-16.4071341001481,-14.8350765822692,
0.));
#33918=CARTESIAN_POINT('Ctrl Pts',(-16.492335117066,-14.8502217520165,0.));
#33919=CARTESIAN_POINT('Ctrl Pts',(-16.5778226646614,-14.8647723257055,
0.));
#33920=CARTESIAN_POINT('Ctrl Pts',(-16.6635911790385,-14.8787307479454,
0.));
#33921=CARTESIAN_POINT('Ctrl Pts',(-16.7496353900706,-14.8920991518626,
0.));
#33922=CARTESIAN_POINT('Ctrl Pts',(-16.8359501981915,-14.9048794721647,
0.));
#33923=CARTESIAN_POINT('Ctrl Pts',(-16.9225305499155,-14.9170735658747,
0.));
#33924=CARTESIAN_POINT('Ctrl Pts',(-17.0093712776822,-14.9286833603319,
0.));
#33925=CARTESIAN_POINT('Ctrl Pts',(-17.0964671184813,-14.9397108660998,
0.));
#33926=CARTESIAN_POINT('Ctrl Pts',(-17.1838128327073,-14.9501581118289,
0.));
#33927=CARTESIAN_POINT('Ctrl Pts',(-17.2714032968314,-14.9600271060471,
0.));
#33928=CARTESIAN_POINT('Ctrl Pts',(-17.3592335908103,-14.9693197947387,
0.));
#33929=CARTESIAN_POINT('Ctrl Pts',(-17.4472991215239,-14.9780380183576,
0.));
#33930=CARTESIAN_POINT('Ctrl Pts',(-17.5355955872257,-14.9861834999847,
0.));
#33931=CARTESIAN_POINT('Ctrl Pts',(-17.6241187988652,-14.9937578646616,
0.));
#33932=CARTESIAN_POINT('Ctrl Pts',(-17.7128645299878,-15.0007626541286,
0.));
#33933=CARTESIAN_POINT('Ctrl Pts',(-17.8018283748074,-15.0071993464636,
0.));
#33934=CARTESIAN_POINT('Ctrl Pts',(-17.891005548971,-15.0130693803259,0.));
#33935=CARTESIAN_POINT('Ctrl Pts',(-17.980390892286,-15.0183741723687,0.));
#33936=CARTESIAN_POINT('Ctrl Pts',(-18.0699792164192,-15.0231151183906,
0.));
#33937=CARTESIAN_POINT('Ctrl Pts',(-18.1597655779328,-15.0272936035154,
0.));
#33938=CARTESIAN_POINT('Ctrl Pts',(-18.2497455679917,-15.0309110092482,
0.));
#33939=CARTESIAN_POINT('Ctrl Pts',(-18.3399156227477,-15.0339687345357,
0.));
#33940=CARTESIAN_POINT('Ctrl Pts',(-18.4483447600234,-15.036968080037,0.));
#33941=CARTESIAN_POINT('Ctrl Pts',(-18.5389347492702,-15.0387713100259,
0.));
#33942=CARTESIAN_POINT('Ctrl Pts',(-18.6115544313469,-15.0397694451467,
0.));
#33943=CARTESIAN_POINT('Ctrl Pts',(-18.6661021851765,-15.0402682932585,
0.));
#33944=CARTESIAN_POINT('Ctrl Pts',(-18.7025042402277,-15.040489857191,0.));
#33945=CARTESIAN_POINT('',(-18.7025042402277,-15.040489857191,15.));
#33946=CARTESIAN_POINT('Ctrl Pts',(-18.7025042402277,-15.040489857191,15.));
#33947=CARTESIAN_POINT('Ctrl Pts',(-18.6843032127312,-15.0403790752228,
15.));
#33948=CARTESIAN_POINT('Ctrl Pts',(-18.6479196005666,-15.0401020105546,
15.));
#33949=CARTESIAN_POINT('Ctrl Pts',(-18.5933995108277,-15.0395199113665,
15.));
#33950=CARTESIAN_POINT('Ctrl Pts',(-18.5208167514208,-15.0384106640281,
15.));
#33951=CARTESIAN_POINT('Ctrl Pts',(-18.4302732371441,-15.0364681891201,
15.));
#33952=CARTESIAN_POINT('Ctrl Pts',(-18.3399156227477,-15.0339687345357,
15.));
#33953=CARTESIAN_POINT('Ctrl Pts',(-18.2497455679917,-15.0309110092482,
15.));
#33954=CARTESIAN_POINT('Ctrl Pts',(-18.1597655779328,-15.0272936035154,
15.));
#33955=CARTESIAN_POINT('Ctrl Pts',(-18.0699792164192,-15.0231151183906,
15.));
#33956=CARTESIAN_POINT('Ctrl Pts',(-17.980390892286,-15.0183741723687,15.));
#33957=CARTESIAN_POINT('Ctrl Pts',(-17.891005548971,-15.0130693803259,15.));
#33958=CARTESIAN_POINT('Ctrl Pts',(-17.8018283748074,-15.0071993464636,
15.));
#33959=CARTESIAN_POINT('Ctrl Pts',(-17.7128645299878,-15.0007626541286,
15.));
#33960=CARTESIAN_POINT('Ctrl Pts',(-17.6241187988652,-14.9937578646616,
15.));
#33961=CARTESIAN_POINT('Ctrl Pts',(-17.5355955872257,-14.9861834999847,
15.));
#33962=CARTESIAN_POINT('Ctrl Pts',(-17.4472991215239,-14.9780380183576,
15.));
#33963=CARTESIAN_POINT('Ctrl Pts',(-17.3592335908103,-14.9693197947387,
15.));
#33964=CARTESIAN_POINT('Ctrl Pts',(-17.2714032968314,-14.9600271060471,
15.));
#33965=CARTESIAN_POINT('Ctrl Pts',(-17.1838128327073,-14.9501581118289,
15.));
#33966=CARTESIAN_POINT('Ctrl Pts',(-17.0964671184813,-14.9397108660998,
15.));
#33967=CARTESIAN_POINT('Ctrl Pts',(-17.0093712776822,-14.9286833603319,
15.));
#33968=CARTESIAN_POINT('Ctrl Pts',(-16.9225305499155,-14.9170735658747,
15.));
#33969=CARTESIAN_POINT('Ctrl Pts',(-16.8359501981915,-14.9048794721647,
15.));
#33970=CARTESIAN_POINT('Ctrl Pts',(-16.7496353900706,-14.8920991518626,
15.));
#33971=CARTESIAN_POINT('Ctrl Pts',(-16.6635911790385,-14.8787307479454,
15.));
#33972=CARTESIAN_POINT('Ctrl Pts',(-16.5778226646614,-14.8647723257055,
15.));
#33973=CARTESIAN_POINT('Ctrl Pts',(-16.492335117066,-14.8502217520165,15.));
#33974=CARTESIAN_POINT('Ctrl Pts',(-16.4071341001481,-14.8350765822692,
15.));
#33975=CARTESIAN_POINT('Ctrl Pts',(-16.3222256264574,-14.8193339134125,
15.));
#33976=CARTESIAN_POINT('Ctrl Pts',(-16.2376161919272,-14.8029903659562,
15.));
#33977=CARTESIAN_POINT('Ctrl Pts',(-16.1533125058853,-14.7860423865308,
15.));
#33978=CARTESIAN_POINT('Ctrl Pts',(-16.0693212651732,-14.7684865075326,
15.));
#33979=CARTESIAN_POINT('Ctrl Pts',(-15.9856489347991,-14.7503195973741,
15.));
#33980=CARTESIAN_POINT('Ctrl Pts',(-15.9023014613802,-14.7315391924939,
15.));
#33981=CARTESIAN_POINT('Ctrl Pts',(-15.8192842036838,-14.7121435744495,
15.));
#33982=CARTESIAN_POINT('Ctrl Pts',(-15.7366025822956,-14.692131002056,15.));
#33983=CARTESIAN_POINT('Ctrl Pts',(-15.6542626345121,-14.6714990558793,
15.));
#33984=CARTESIAN_POINT('Ctrl Pts',(-15.5722715494357,-14.6502440080911,
15.));
#33985=CARTESIAN_POINT('Ctrl Pts',(-15.4906383406647,-14.6283600295736,
15.));
#33986=CARTESIAN_POINT('Ctrl Pts',(-15.4093740621548,-14.6058389416146,
15.));
#33987=CARTESIAN_POINT('Ctrl Pts',(-15.3284903715086,-14.5826719336929,
15.));
#33988=CARTESIAN_POINT('Ctrl Pts',(-15.2479982823383,-14.5588510579962,
15.));
#33989=CARTESIAN_POINT('Ctrl Pts',(-15.1679069808052,-14.534370647705,15.));
#33990=CARTESIAN_POINT('Ctrl Pts',(-15.0882222764759,-14.5092291736391,
15.));
#33991=CARTESIAN_POINT('Ctrl Pts',(-15.0089462280505,-14.4834296977405,
15.));
#33992=CARTESIAN_POINT('Ctrl Pts',(-14.9300806580357,-14.4569756801697,
15.));
#33993=CARTESIAN_POINT('Ctrl Pts',(-14.8516302160049,-14.4298673266313,
15.));
#33994=CARTESIAN_POINT('Ctrl Pts',(-14.7736052248294,-14.4020981965564,
15.));
#33995=CARTESIAN_POINT('Ctrl Pts',(-14.6960255561799,-14.3736505809735,
15.));
#33996=CARTESIAN_POINT('Ctrl Pts',(-14.6189211183837,-14.3444949335274,
15.));
#33997=CARTESIAN_POINT('Ctrl Pts',(-14.5423237181615,-14.3145996213697,
15.));
#33998=CARTESIAN_POINT('Ctrl Pts',(-14.4662599802682,-14.2839394106401,
15.));
#33999=CARTESIAN_POINT('Ctrl Pts',(-14.3907450096103,-14.2525030666863,
15.));
#34000=CARTESIAN_POINT('Ctrl Pts',(-14.3157729256101,-14.2203046917613,
15.));
#34001=CARTESIAN_POINT('Ctrl Pts',(-14.2413181097468,-14.1873822640681,
15.));
#34002=CARTESIAN_POINT('Ctrl Pts',(-14.1673550455622,-14.1537739659715,
15.));
#34003=CARTESIAN_POINT('Ctrl Pts',(-14.0938755647891,-14.1194976094444,
15.));
#34004=CARTESIAN_POINT('Ctrl Pts',(-14.0209038736616,-14.0845327205726,
15.));
#34005=CARTESIAN_POINT('Ctrl Pts',(-13.9485205009332,-14.0487919508068,
15.));
#34006=CARTESIAN_POINT('Ctrl Pts',(-13.876852657608,-14.0121326766855,15.));
#34007=CARTESIAN_POINT('Ctrl Pts',(-13.806028835706,-13.9744114225699,15.));
#34008=CARTESIAN_POINT('Ctrl Pts',(-13.7361389175879,-13.9355316323567,
15.));
#34009=CARTESIAN_POINT('Ctrl Pts',(-13.6672004242289,-13.8954842290745,
15.));
#34010=CARTESIAN_POINT('Ctrl Pts',(-13.5991011046042,-13.854416158639,15.));
#34011=CARTESIAN_POINT('Ctrl Pts',(-13.5316488646659,-13.8125718693898,
15.));
#34012=CARTESIAN_POINT('Ctrl Pts',(-13.4646849459541,-13.7701598398937,
15.));
#34013=CARTESIAN_POINT('Ctrl Pts',(-13.3981837093919,-13.7272351052346,
15.));
#34014=CARTESIAN_POINT('Ctrl Pts',(-13.332345249068,-13.6835899659728,15.));
#34015=CARTESIAN_POINT('Ctrl Pts',(-13.267724591625,-13.6386021757691,15.));
#34016=CARTESIAN_POINT('Ctrl Pts',(-13.2050958591127,-13.5913916488449,
15.));
#34017=CARTESIAN_POINT('Ctrl Pts',(-13.1572182238498,-13.5511230466604,
15.));
#34018=CARTESIAN_POINT('Ctrl Pts',(-13.1228431405579,-13.5191927531554,
15.));
#34019=CARTESIAN_POINT('Ctrl Pts',(-13.1006438497967,-13.4970961329957,
15.));
#34020=CARTESIAN_POINT('Ctrl Pts',(-13.0897235660237,-13.4858453790958,
15.));
#34021=CARTESIAN_POINT('',(-18.7025042402277,-15.040489857191,0.));
#34022=CARTESIAN_POINT('Origin',(-9.34524724197226E-14,-6.78114261146376E-14,
0.));
#34023=CARTESIAN_POINT('',(-20.0837475345526,-13.1393715591102,0.));
#34024=CARTESIAN_POINT('Origin',(-9.34524724197226E-14,-6.78114261146376E-14,
0.));
#34025=CARTESIAN_POINT('',(-20.0837475345526,-13.1393715591102,15.));
#34026=CARTESIAN_POINT('Origin',(-9.34524724197226E-14,-6.78114261146376E-14,
15.));
#34027=CARTESIAN_POINT('',(-20.0837475345526,-13.1393715591102,0.));
#34028=CARTESIAN_POINT('Ctrl Pts',(-16.8707481591095,-8.28171148831561,
0.));
#34029=CARTESIAN_POINT('Ctrl Pts',(-16.8707481591095,-8.28171148831561,
18.));
#34030=CARTESIAN_POINT('Ctrl Pts',(-16.8848228151885,-8.28862062120314,
0.));
#34031=CARTESIAN_POINT('Ctrl Pts',(-16.8848228151885,-8.28862062120314,
18.));
#34032=CARTESIAN_POINT('Ctrl Pts',(-16.9126979078877,-8.30290517019115,
0.));
#34033=CARTESIAN_POINT('Ctrl Pts',(-16.9126979078877,-8.30290517019115,
18.));
#34034=CARTESIAN_POINT('Ctrl Pts',(-16.9536879065132,-8.32573081382562,
0.));
#34035=CARTESIAN_POINT('Ctrl Pts',(-16.9536879065132,-8.32573081382562,
18.));
#34036=CARTESIAN_POINT('Ctrl Pts',(-17.0067806259695,-8.35882146841243,
0.));
#34037=CARTESIAN_POINT('Ctrl Pts',(-17.0067806259695,-8.35882146841243,
18.));
#34038=CARTESIAN_POINT('Ctrl Pts',(-17.071033847921,-8.40379607744265,0.));
#34039=CARTESIAN_POINT('Ctrl Pts',(-17.071033847921,-8.40379607744265,18.));
#34040=CARTESIAN_POINT('Ctrl Pts',(-17.1337886602855,-8.45135198307876,
0.));
#34041=CARTESIAN_POINT('Ctrl Pts',(-17.1337886602855,-8.45135198307876,
18.));
#34042=CARTESIAN_POINT('Ctrl Pts',(-17.1956428575086,-8.50048099003882,
0.));
#34043=CARTESIAN_POINT('Ctrl Pts',(-17.1956428575086,-8.50048099003882,
18.));
#34044=CARTESIAN_POINT('Ctrl Pts',(-17.2570167183611,-8.55046295192433,
0.));
#34045=CARTESIAN_POINT('Ctrl Pts',(-17.2570167183611,-8.55046295192433,
18.));
#34046=CARTESIAN_POINT('Ctrl Pts',(-17.3180459442745,-8.60104338529165,
0.));
#34047=CARTESIAN_POINT('Ctrl Pts',(-17.3180459442745,-8.60104338529165,
18.));
#34048=CARTESIAN_POINT('Ctrl Pts',(-17.3786861166843,-8.65226368112815,
0.));
#34049=CARTESIAN_POINT('Ctrl Pts',(-17.3786861166843,-8.65226368112815,
18.));
#34050=CARTESIAN_POINT('Ctrl Pts',(-17.438788019753,-8.70433925112174,0.));
#34051=CARTESIAN_POINT('Ctrl Pts',(-17.438788019753,-8.70433925112174,18.));
#34052=CARTESIAN_POINT('Ctrl Pts',(-17.4981785296199,-8.75752832625954,
0.));
#34053=CARTESIAN_POINT('Ctrl Pts',(-17.4981785296199,-8.75752832625954,
18.));
#34054=CARTESIAN_POINT('Ctrl Pts',(-17.5567525798882,-8.8119830723955,0.));
#34055=CARTESIAN_POINT('Ctrl Pts',(-17.5567525798882,-8.8119830723955,18.));
#34056=CARTESIAN_POINT('Ctrl Pts',(-17.614513388992,-8.86768402115343,0.));
#34057=CARTESIAN_POINT('Ctrl Pts',(-17.614513388992,-8.86768402115343,18.));
#34058=CARTESIAN_POINT('Ctrl Pts',(-17.6715250120654,-8.92451585185175,
0.));
#34059=CARTESIAN_POINT('Ctrl Pts',(-17.6715250120654,-8.92451585185175,
18.));
#34060=CARTESIAN_POINT('Ctrl Pts',(-17.7278841963319,-8.98231202490685,
0.));
#34061=CARTESIAN_POINT('Ctrl Pts',(-17.7278841963319,-8.98231202490685,
18.));
#34062=CARTESIAN_POINT('Ctrl Pts',(-17.7836872744016,-9.04090748239097,
0.));
#34063=CARTESIAN_POINT('Ctrl Pts',(-17.7836872744016,-9.04090748239097,
18.));
#34064=CARTESIAN_POINT('Ctrl Pts',(-17.8389924349283,-9.10019864472208,
0.));
#34065=CARTESIAN_POINT('Ctrl Pts',(-17.8389924349283,-9.10019864472208,
18.));
#34066=CARTESIAN_POINT('Ctrl Pts',(-17.8938116696237,-9.16015616361609,
0.));
#34067=CARTESIAN_POINT('Ctrl Pts',(-17.8938116696237,-9.16015616361609,
18.));
#34068=CARTESIAN_POINT('Ctrl Pts',(-17.9481305624284,-9.22079331175917,
0.));
#34069=CARTESIAN_POINT('Ctrl Pts',(-17.9481305624284,-9.22079331175917,
18.));
#34070=CARTESIAN_POINT('Ctrl Pts',(-18.0019206847747,-9.2821461557447,0.));
#34071=CARTESIAN_POINT('Ctrl Pts',(-18.0019206847747,-9.2821461557447,18.));
#34072=CARTESIAN_POINT('Ctrl Pts',(-18.0551538338035,-9.34425079614395,
0.));
#34073=CARTESIAN_POINT('Ctrl Pts',(-18.0551538338035,-9.34425079614395,
18.));
#34074=CARTESIAN_POINT('Ctrl Pts',(-18.1078184146735,-9.40711718355464,
0.));
#34075=CARTESIAN_POINT('Ctrl Pts',(-18.1078184146735,-9.40711718355464,
18.));
#34076=CARTESIAN_POINT('Ctrl Pts',(-18.1599204445014,-9.47072748065831,
0.));
#34077=CARTESIAN_POINT('Ctrl Pts',(-18.1599204445014,-9.47072748065831,
18.));
#34078=CARTESIAN_POINT('Ctrl Pts',(-18.2114756946126,-9.53504856811685,
0.));
#34079=CARTESIAN_POINT('Ctrl Pts',(-18.2114756946126,-9.53504856811685,
18.));
#34080=CARTESIAN_POINT('Ctrl Pts',(-18.2625044208165,-9.60004042085346,
0.));
#34081=CARTESIAN_POINT('Ctrl Pts',(-18.2625044208165,-9.60004042085346,
18.));
#34082=CARTESIAN_POINT('Ctrl Pts',(-18.3130254811852,-9.66566546403259,
0.));
#34083=CARTESIAN_POINT('Ctrl Pts',(-18.3130254811852,-9.66566546403259,
18.));
#34084=CARTESIAN_POINT('Ctrl Pts',(-18.3630495772677,-9.73189932619939,
0.));
#34085=CARTESIAN_POINT('Ctrl Pts',(-18.3630495772677,-9.73189932619939,
18.));
#34086=CARTESIAN_POINT('Ctrl Pts',(-18.4125796444662,-9.79873019947433,
0.));
#34087=CARTESIAN_POINT('Ctrl Pts',(-18.4125796444662,-9.79873019947433,
18.));
#34088=CARTESIAN_POINT('Ctrl Pts',(-18.461614050347,-9.86615372541684,0.));
#34089=CARTESIAN_POINT('Ctrl Pts',(-18.461614050347,-9.86615372541684,18.));
#34090=CARTESIAN_POINT('Ctrl Pts',(-18.5101489409161,-9.93416923996828,
0.));
#34091=CARTESIAN_POINT('Ctrl Pts',(-18.5101489409161,-9.93416923996828,
18.));
#34092=CARTESIAN_POINT('Ctrl Pts',(-18.5581807679204,-10.0027757313807,
0.));
#34093=CARTESIAN_POINT('Ctrl Pts',(-18.5581807679204,-10.0027757313807,
18.));
#34094=CARTESIAN_POINT('Ctrl Pts',(-18.605709190442,-10.0719672018851,0.));
#34095=CARTESIAN_POINT('Ctrl Pts',(-18.605709190442,-10.0719672018851,18.));
#34096=CARTESIAN_POINT('Ctrl Pts',(-18.6527367592664,-10.1417331637795,
0.));
#34097=CARTESIAN_POINT('Ctrl Pts',(-18.6527367592664,-10.1417331637795,
18.));
#34098=CARTESIAN_POINT('Ctrl Pts',(-18.699267629819,-10.2120606864872,0.));
#34099=CARTESIAN_POINT('Ctrl Pts',(-18.699267629819,-10.2120606864872,18.));
#34100=CARTESIAN_POINT('Ctrl Pts',(-18.7453065790062,-10.2829359603685,
0.));
#34101=CARTESIAN_POINT('Ctrl Pts',(-18.7453065790062,-10.2829359603685,
18.));
#34102=CARTESIAN_POINT('Ctrl Pts',(-18.7908579693851,-10.3543459451258,
0.));
#34103=CARTESIAN_POINT('Ctrl Pts',(-18.7908579693851,-10.3543459451258,
18.));
#34104=CARTESIAN_POINT('Ctrl Pts',(-18.8359245594214,-10.4262802670211,
0.));
#34105=CARTESIAN_POINT('Ctrl Pts',(-18.8359245594214,-10.4262802670211,
18.));
#34106=CARTESIAN_POINT('Ctrl Pts',(-18.8805076729356,-10.4987309368494,
0.));
#34107=CARTESIAN_POINT('Ctrl Pts',(-18.8805076729356,-10.4987309368494,
18.));
#34108=CARTESIAN_POINT('Ctrl Pts',(-18.9246077453188,-10.5716914651544,
0.));
#34109=CARTESIAN_POINT('Ctrl Pts',(-18.9246077453188,-10.5716914651544,
18.));
#34110=CARTESIAN_POINT('Ctrl Pts',(-18.9682247574834,-10.6451561585969,
0.));
#34111=CARTESIAN_POINT('Ctrl Pts',(-18.9682247574834,-10.6451561585969,
18.));
#34112=CARTESIAN_POINT('Ctrl Pts',(-19.0113586878152,-10.7191193896586,
0.));
#34113=CARTESIAN_POINT('Ctrl Pts',(-19.0113586878152,-10.7191193896586,
18.));
#34114=CARTESIAN_POINT('Ctrl Pts',(-19.0540100416943,-10.7935747414879,
0.));
#34115=CARTESIAN_POINT('Ctrl Pts',(-19.0540100416943,-10.7935747414879,
18.));
#34116=CARTESIAN_POINT('Ctrl Pts',(-19.0961797996403,-10.868515097783,0.));
#34117=CARTESIAN_POINT('Ctrl Pts',(-19.0961797996403,-10.868515097783,18.));
#34118=CARTESIAN_POINT('Ctrl Pts',(-19.1378691901023,-10.9439330179206,
0.));
#34119=CARTESIAN_POINT('Ctrl Pts',(-19.1378691901023,-10.9439330179206,
18.));
#34120=CARTESIAN_POINT('Ctrl Pts',(-19.1790795192393,-11.0198210228993,
0.));
#34121=CARTESIAN_POINT('Ctrl Pts',(-19.1790795192393,-11.0198210228993,
18.));
#34122=CARTESIAN_POINT('Ctrl Pts',(-19.2198119937835,-11.0961718903994,
0.));
#34123=CARTESIAN_POINT('Ctrl Pts',(-19.2198119937835,-11.0961718903994,
18.));
#34124=CARTESIAN_POINT('Ctrl Pts',(-19.2600675167206,-11.1729790050543,
0.));
#34125=CARTESIAN_POINT('Ctrl Pts',(-19.2600675167206,-11.1729790050543,
18.));
#34126=CARTESIAN_POINT('Ctrl Pts',(-19.2998466936739,-11.2502363198588,
0.));
#34127=CARTESIAN_POINT('Ctrl Pts',(-19.2998466936739,-11.2502363198588,
18.));
#34128=CARTESIAN_POINT('Ctrl Pts',(-19.3391499248083,-11.3279381634523,
0.));
#34129=CARTESIAN_POINT('Ctrl Pts',(-19.3391499248083,-11.3279381634523,
18.));
#34130=CARTESIAN_POINT('Ctrl Pts',(-19.3779774742876,-11.4060790880015,
0.));
#34131=CARTESIAN_POINT('Ctrl Pts',(-19.3779774742876,-11.4060790880015,
18.));
#34132=CARTESIAN_POINT('Ctrl Pts',(-19.4163295466324,-11.4846537135043,
0.));
#34133=CARTESIAN_POINT('Ctrl Pts',(-19.4163295466324,-11.4846537135043,
18.));
#34134=CARTESIAN_POINT('Ctrl Pts',(-19.4542063779876,-11.5636565297382,
0.));
#34135=CARTESIAN_POINT('Ctrl Pts',(-19.4542063779876,-11.5636565297382,
18.));
#34136=CARTESIAN_POINT('Ctrl Pts',(-19.4916082541529,-11.6430819099846,
0.));
#34137=CARTESIAN_POINT('Ctrl Pts',(-19.4916082541529,-11.6430819099846,
18.));
#34138=CARTESIAN_POINT('Ctrl Pts',(-19.5285354853626,-11.722924244195,0.));
#34139=CARTESIAN_POINT('Ctrl Pts',(-19.5285354853626,-11.722924244195,18.));
#34140=CARTESIAN_POINT('Ctrl Pts',(-19.5649883985826,-11.8031780389346,
0.));
#34141=CARTESIAN_POINT('Ctrl Pts',(-19.5649883985826,-11.8031780389346,
18.));
#34142=CARTESIAN_POINT('Ctrl Pts',(-19.6009673241771,-11.8838380136222,
0.));
#34143=CARTESIAN_POINT('Ctrl Pts',(-19.6009673241771,-11.8838380136222,
18.));
#34144=CARTESIAN_POINT('Ctrl Pts',(-19.6364725931695,-11.9648992312094,
0.));
#34145=CARTESIAN_POINT('Ctrl Pts',(-19.6364725931695,-11.9648992312094,
18.));
#34146=CARTESIAN_POINT('Ctrl Pts',(-19.6715045149944,-12.0463570680308,
0.));
#34147=CARTESIAN_POINT('Ctrl Pts',(-19.6715045149944,-12.0463570680308,
18.));
#34148=CARTESIAN_POINT('Ctrl Pts',(-19.7060633406705,-12.1282070378972,
0.));
#34149=CARTESIAN_POINT('Ctrl Pts',(-19.7060633406705,-12.1282070378972,
18.));
#34150=CARTESIAN_POINT('Ctrl Pts',(-19.7401492304335,-12.2104446447874,
0.));
#34151=CARTESIAN_POINT('Ctrl Pts',(-19.7401492304335,-12.2104446447874,
18.));
#34152=CARTESIAN_POINT('Ctrl Pts',(-19.7737622285562,-12.2930652417986,
0.));
#34153=CARTESIAN_POINT('Ctrl Pts',(-19.7737622285562,-12.2930652417986,
18.));
#34154=CARTESIAN_POINT('Ctrl Pts',(-19.8069022248387,-12.3760638341708,
0.));
#34155=CARTESIAN_POINT('Ctrl Pts',(-19.8069022248387,-12.3760638341708,
18.));
#34156=CARTESIAN_POINT('Ctrl Pts',(-19.839568972011,-12.4594350764989,0.));
#34157=CARTESIAN_POINT('Ctrl Pts',(-19.839568972011,-12.4594350764989,18.));
#34158=CARTESIAN_POINT('Ctrl Pts',(-19.8717621942733,-12.5431736030595,
0.));
#34159=CARTESIAN_POINT('Ctrl Pts',(-19.8717621942733,-12.5431736030595,
18.));
#34160=CARTESIAN_POINT('Ctrl Pts',(-19.9034816813503,-12.6272742843372,
0.));
#34161=CARTESIAN_POINT('Ctrl Pts',(-19.9034816813503,-12.6272742843372,
18.));
#34162=CARTESIAN_POINT('Ctrl Pts',(-19.9347273847264,-12.7117325003719,
0.));
#34163=CARTESIAN_POINT('Ctrl Pts',(-19.9347273847264,-12.7117325003719,
18.));
#34164=CARTESIAN_POINT('Ctrl Pts',(-19.9654995335894,-12.7965444294443,
0.));
#34165=CARTESIAN_POINT('Ctrl Pts',(-19.9654995335894,-12.7965444294443,
18.));
#34166=CARTESIAN_POINT('Ctrl Pts',(-19.9957986945787,-12.8817072534696,
0.));
#34167=CARTESIAN_POINT('Ctrl Pts',(-19.9957986945787,-12.8817072534696,
18.));
#34168=CARTESIAN_POINT('Ctrl Pts',(-20.0256255826397,-12.9672189949731,
0.));
#34169=CARTESIAN_POINT('Ctrl Pts',(-20.0256255826397,-12.9672189949731,
18.));
#34170=CARTESIAN_POINT('Ctrl Pts',(-20.0491098457044,-13.0359065249991,
0.));
#34171=CARTESIAN_POINT('Ctrl Pts',(-20.0491098457044,-13.0359065249991,
18.));
#34172=CARTESIAN_POINT('Ctrl Pts',(-20.0665110891946,-13.0875783330728,
0.));
#34173=CARTESIAN_POINT('Ctrl Pts',(-20.0665110891946,-13.0875783330728,
18.));
#34174=CARTESIAN_POINT('Ctrl Pts',(-20.0780177478283,-13.1220955868173,
0.));
#34175=CARTESIAN_POINT('Ctrl Pts',(-20.0780177478283,-13.1220955868173,
18.));
#34176=CARTESIAN_POINT('Ctrl Pts',(-20.0837475345526,-13.1393715591102,
0.));
#34177=CARTESIAN_POINT('Ctrl Pts',(-20.0837475345526,-13.1393715591102,
18.));
#34178=CARTESIAN_POINT('Ctrl Pts',(-16.8707481591095,-8.28171148831561,
0.));
#34179=CARTESIAN_POINT('Ctrl Pts',(-16.8848228151885,-8.28862062120314,
0.));
#34180=CARTESIAN_POINT('Ctrl Pts',(-16.9126979078877,-8.30290517019115,
0.));
#34181=CARTESIAN_POINT('Ctrl Pts',(-16.9536879065132,-8.32573081382562,
0.));
#34182=CARTESIAN_POINT('Ctrl Pts',(-17.0067806259695,-8.35882146841243,
0.));
#34183=CARTESIAN_POINT('Ctrl Pts',(-17.071033847921,-8.40379607744265,0.));
#34184=CARTESIAN_POINT('Ctrl Pts',(-17.1337886602855,-8.45135198307876,
0.));
#34185=CARTESIAN_POINT('Ctrl Pts',(-17.1956428575086,-8.50048099003882,
0.));
#34186=CARTESIAN_POINT('Ctrl Pts',(-17.2570167183611,-8.55046295192433,
0.));
#34187=CARTESIAN_POINT('Ctrl Pts',(-17.3180459442745,-8.60104338529165,
0.));
#34188=CARTESIAN_POINT('Ctrl Pts',(-17.3786861166843,-8.65226368112815,
0.));
#34189=CARTESIAN_POINT('Ctrl Pts',(-17.438788019753,-8.70433925112174,0.));
#34190=CARTESIAN_POINT('Ctrl Pts',(-17.4981785296199,-8.75752832625954,
0.));
#34191=CARTESIAN_POINT('Ctrl Pts',(-17.5567525798882,-8.8119830723955,0.));
#34192=CARTESIAN_POINT('Ctrl Pts',(-17.614513388992,-8.86768402115343,0.));
#34193=CARTESIAN_POINT('Ctrl Pts',(-17.6715250120654,-8.92451585185175,
0.));
#34194=CARTESIAN_POINT('Ctrl Pts',(-17.7278841963319,-8.98231202490685,
0.));
#34195=CARTESIAN_POINT('Ctrl Pts',(-17.7836872744016,-9.04090748239097,
0.));
#34196=CARTESIAN_POINT('Ctrl Pts',(-17.8389924349283,-9.10019864472208,
0.));
#34197=CARTESIAN_POINT('Ctrl Pts',(-17.8938116696237,-9.16015616361609,
0.));
#34198=CARTESIAN_POINT('Ctrl Pts',(-17.9481305624284,-9.22079331175917,
0.));
#34199=CARTESIAN_POINT('Ctrl Pts',(-18.0019206847747,-9.2821461557447,0.));
#34200=CARTESIAN_POINT('Ctrl Pts',(-18.0551538338035,-9.34425079614395,
0.));
#34201=CARTESIAN_POINT('Ctrl Pts',(-18.1078184146735,-9.40711718355464,
0.));
#34202=CARTESIAN_POINT('Ctrl Pts',(-18.1599204445014,-9.47072748065831,
0.));
#34203=CARTESIAN_POINT('Ctrl Pts',(-18.2114756946126,-9.53504856811685,
0.));
#34204=CARTESIAN_POINT('Ctrl Pts',(-18.2625044208165,-9.60004042085346,
0.));
#34205=CARTESIAN_POINT('Ctrl Pts',(-18.3130254811852,-9.66566546403259,
0.));
#34206=CARTESIAN_POINT('Ctrl Pts',(-18.3630495772677,-9.73189932619939,
0.));
#34207=CARTESIAN_POINT('Ctrl Pts',(-18.4125796444662,-9.79873019947433,
0.));
#34208=CARTESIAN_POINT('Ctrl Pts',(-18.461614050347,-9.86615372541684,0.));
#34209=CARTESIAN_POINT('Ctrl Pts',(-18.5101489409161,-9.93416923996828,
0.));
#34210=CARTESIAN_POINT('Ctrl Pts',(-18.5581807679204,-10.0027757313807,
0.));
#34211=CARTESIAN_POINT('Ctrl Pts',(-18.605709190442,-10.0719672018851,0.));
#34212=CARTESIAN_POINT('Ctrl Pts',(-18.6527367592664,-10.1417331637795,
0.));
#34213=CARTESIAN_POINT('Ctrl Pts',(-18.699267629819,-10.2120606864872,0.));
#34214=CARTESIAN_POINT('Ctrl Pts',(-18.7453065790062,-10.2829359603685,
0.));
#34215=CARTESIAN_POINT('Ctrl Pts',(-18.7908579693851,-10.3543459451258,
0.));
#34216=CARTESIAN_POINT('Ctrl Pts',(-18.8359245594214,-10.4262802670211,
0.));
#34217=CARTESIAN_POINT('Ctrl Pts',(-18.8805076729356,-10.4987309368494,
0.));
#34218=CARTESIAN_POINT('Ctrl Pts',(-18.9246077453188,-10.5716914651544,
0.));
#34219=CARTESIAN_POINT('Ctrl Pts',(-18.9682247574834,-10.6451561585969,
0.));
#34220=CARTESIAN_POINT('Ctrl Pts',(-19.0113586878152,-10.7191193896586,
0.));
#34221=CARTESIAN_POINT('Ctrl Pts',(-19.0540100416943,-10.7935747414879,
0.));
#34222=CARTESIAN_POINT('Ctrl Pts',(-19.0961797996403,-10.868515097783,0.));
#34223=CARTESIAN_POINT('Ctrl Pts',(-19.1378691901023,-10.9439330179206,
0.));
#34224=CARTESIAN_POINT('Ctrl Pts',(-19.1790795192393,-11.0198210228993,
0.));
#34225=CARTESIAN_POINT('Ctrl Pts',(-19.2198119937835,-11.0961718903994,
0.));
#34226=CARTESIAN_POINT('Ctrl Pts',(-19.2600675167206,-11.1729790050543,
0.));
#34227=CARTESIAN_POINT('Ctrl Pts',(-19.2998466936739,-11.2502363198588,
0.));
#34228=CARTESIAN_POINT('Ctrl Pts',(-19.3391499248083,-11.3279381634523,
0.));
#34229=CARTESIAN_POINT('Ctrl Pts',(-19.3779774742876,-11.4060790880015,
0.));
#34230=CARTESIAN_POINT('Ctrl Pts',(-19.4163295466324,-11.4846537135043,
0.));
#34231=CARTESIAN_POINT('Ctrl Pts',(-19.4542063779876,-11.5636565297382,
0.));
#34232=CARTESIAN_POINT('Ctrl Pts',(-19.4916082541529,-11.6430819099846,
0.));
#34233=CARTESIAN_POINT('Ctrl Pts',(-19.5285354853626,-11.722924244195,0.));
#34234=CARTESIAN_POINT('Ctrl Pts',(-19.5649883985826,-11.8031780389346,
0.));
#34235=CARTESIAN_POINT('Ctrl Pts',(-19.6009673241771,-11.8838380136222,
0.));
#34236=CARTESIAN_POINT('Ctrl Pts',(-19.6364725931695,-11.9648992312094,
0.));
#34237=CARTESIAN_POINT('Ctrl Pts',(-19.6715045149944,-12.0463570680308,
0.));
#34238=CARTESIAN_POINT('Ctrl Pts',(-19.7060633406705,-12.1282070378972,
0.));
#34239=CARTESIAN_POINT('Ctrl Pts',(-19.7401492304335,-12.2104446447874,
0.));
#34240=CARTESIAN_POINT('Ctrl Pts',(-19.7737622285562,-12.2930652417986,
0.));
#34241=CARTESIAN_POINT('Ctrl Pts',(-19.8069022248387,-12.3760638341708,
0.));
#34242=CARTESIAN_POINT('Ctrl Pts',(-19.839568972011,-12.4594350764989,0.));
#34243=CARTESIAN_POINT('Ctrl Pts',(-19.8717621942733,-12.5431736030595,
0.));
#34244=CARTESIAN_POINT('Ctrl Pts',(-19.9034816813503,-12.6272742843372,
0.));
#34245=CARTESIAN_POINT('Ctrl Pts',(-19.9347273847264,-12.7117325003719,
0.));
#34246=CARTESIAN_POINT('Ctrl Pts',(-19.9654995335894,-12.7965444294443,
0.));
#34247=CARTESIAN_POINT('Ctrl Pts',(-20.0018585267766,-12.8987398182747,
0.));
#34248=CARTESIAN_POINT('Ctrl Pts',(-20.0315673466055,-12.9843387891477,
0.));
#34249=CARTESIAN_POINT('Ctrl Pts',(-20.054957345404,-13.0530957702829,0.));
#34250=CARTESIAN_POINT('Ctrl Pts',(-20.0722879610899,-13.1048196144678,
0.));
#34251=CARTESIAN_POINT('Ctrl Pts',(-20.0837475345526,-13.1393715591102,
0.));
#34252=CARTESIAN_POINT('Ctrl Pts',(-16.8707481591095,-8.28171148831561,
15.));
#34253=CARTESIAN_POINT('Ctrl Pts',(-16.8848228151885,-8.28862062120314,
15.));
#34254=CARTESIAN_POINT('Ctrl Pts',(-16.9126979078877,-8.30290517019115,
15.));
#34255=CARTESIAN_POINT('Ctrl Pts',(-16.9536879065132,-8.32573081382562,
15.));
#34256=CARTESIAN_POINT('Ctrl Pts',(-17.0067806259695,-8.35882146841243,
15.));
#34257=CARTESIAN_POINT('Ctrl Pts',(-17.071033847921,-8.40379607744265,15.));
#34258=CARTESIAN_POINT('Ctrl Pts',(-17.1337886602855,-8.45135198307876,
15.));
#34259=CARTESIAN_POINT('Ctrl Pts',(-17.1956428575086,-8.50048099003882,
15.));
#34260=CARTESIAN_POINT('Ctrl Pts',(-17.2570167183611,-8.55046295192433,
15.));
#34261=CARTESIAN_POINT('Ctrl Pts',(-17.3180459442745,-8.60104338529165,
15.));
#34262=CARTESIAN_POINT('Ctrl Pts',(-17.3786861166843,-8.65226368112815,
15.));
#34263=CARTESIAN_POINT('Ctrl Pts',(-17.438788019753,-8.70433925112174,15.));
#34264=CARTESIAN_POINT('Ctrl Pts',(-17.4981785296199,-8.75752832625954,
15.));
#34265=CARTESIAN_POINT('Ctrl Pts',(-17.5567525798882,-8.8119830723955,15.));
#34266=CARTESIAN_POINT('Ctrl Pts',(-17.614513388992,-8.86768402115343,15.));
#34267=CARTESIAN_POINT('Ctrl Pts',(-17.6715250120654,-8.92451585185175,
15.));
#34268=CARTESIAN_POINT('Ctrl Pts',(-17.7278841963319,-8.98231202490685,
15.));
#34269=CARTESIAN_POINT('Ctrl Pts',(-17.7836872744016,-9.04090748239097,
15.));
#34270=CARTESIAN_POINT('Ctrl Pts',(-17.8389924349283,-9.10019864472208,
15.));
#34271=CARTESIAN_POINT('Ctrl Pts',(-17.8938116696237,-9.16015616361609,
15.));
#34272=CARTESIAN_POINT('Ctrl Pts',(-17.9481305624284,-9.22079331175917,
15.));
#34273=CARTESIAN_POINT('Ctrl Pts',(-18.0019206847747,-9.2821461557447,15.));
#34274=CARTESIAN_POINT('Ctrl Pts',(-18.0551538338035,-9.34425079614395,
15.));
#34275=CARTESIAN_POINT('Ctrl Pts',(-18.1078184146735,-9.40711718355464,
15.));
#34276=CARTESIAN_POINT('Ctrl Pts',(-18.1599204445014,-9.47072748065831,
15.));
#34277=CARTESIAN_POINT('Ctrl Pts',(-18.2114756946126,-9.53504856811685,
15.));
#34278=CARTESIAN_POINT('Ctrl Pts',(-18.2625044208165,-9.60004042085346,
15.));
#34279=CARTESIAN_POINT('Ctrl Pts',(-18.3130254811852,-9.66566546403259,
15.));
#34280=CARTESIAN_POINT('Ctrl Pts',(-18.3630495772677,-9.73189932619939,
15.));
#34281=CARTESIAN_POINT('Ctrl Pts',(-18.4125796444662,-9.79873019947433,
15.));
#34282=CARTESIAN_POINT('Ctrl Pts',(-18.461614050347,-9.86615372541684,15.));
#34283=CARTESIAN_POINT('Ctrl Pts',(-18.5101489409161,-9.93416923996828,
15.));
#34284=CARTESIAN_POINT('Ctrl Pts',(-18.5581807679204,-10.0027757313807,
15.));
#34285=CARTESIAN_POINT('Ctrl Pts',(-18.605709190442,-10.0719672018851,15.));
#34286=CARTESIAN_POINT('Ctrl Pts',(-18.6527367592664,-10.1417331637795,
15.));
#34287=CARTESIAN_POINT('Ctrl Pts',(-18.699267629819,-10.2120606864872,15.));
#34288=CARTESIAN_POINT('Ctrl Pts',(-18.7453065790062,-10.2829359603685,
15.));
#34289=CARTESIAN_POINT('Ctrl Pts',(-18.7908579693851,-10.3543459451258,
15.));
#34290=CARTESIAN_POINT('Ctrl Pts',(-18.8359245594214,-10.4262802670211,
15.));
#34291=CARTESIAN_POINT('Ctrl Pts',(-18.8805076729356,-10.4987309368494,
15.));
#34292=CARTESIAN_POINT('Ctrl Pts',(-18.9246077453188,-10.5716914651544,
15.));
#34293=CARTESIAN_POINT('Ctrl Pts',(-18.9682247574834,-10.6451561585969,
15.));
#34294=CARTESIAN_POINT('Ctrl Pts',(-19.0113586878152,-10.7191193896586,
15.));
#34295=CARTESIAN_POINT('Ctrl Pts',(-19.0540100416943,-10.7935747414879,
15.));
#34296=CARTESIAN_POINT('Ctrl Pts',(-19.0961797996403,-10.868515097783,15.));
#34297=CARTESIAN_POINT('Ctrl Pts',(-19.1378691901023,-10.9439330179206,
15.));
#34298=CARTESIAN_POINT('Ctrl Pts',(-19.1790795192393,-11.0198210228993,
15.));
#34299=CARTESIAN_POINT('Ctrl Pts',(-19.2198119937835,-11.0961718903994,
15.));
#34300=CARTESIAN_POINT('Ctrl Pts',(-19.2600675167206,-11.1729790050543,
15.));
#34301=CARTESIAN_POINT('Ctrl Pts',(-19.2998466936739,-11.2502363198588,
15.));
#34302=CARTESIAN_POINT('Ctrl Pts',(-19.3391499248083,-11.3279381634523,
15.));
#34303=CARTESIAN_POINT('Ctrl Pts',(-19.3779774742876,-11.4060790880015,
15.));
#34304=CARTESIAN_POINT('Ctrl Pts',(-19.4163295466324,-11.4846537135043,
15.));
#34305=CARTESIAN_POINT('Ctrl Pts',(-19.4542063779876,-11.5636565297382,
15.));
#34306=CARTESIAN_POINT('Ctrl Pts',(-19.4916082541529,-11.6430819099846,
15.));
#34307=CARTESIAN_POINT('Ctrl Pts',(-19.5285354853626,-11.722924244195,15.));
#34308=CARTESIAN_POINT('Ctrl Pts',(-19.5649883985826,-11.8031780389346,
15.));
#34309=CARTESIAN_POINT('Ctrl Pts',(-19.6009673241771,-11.8838380136222,
15.));
#34310=CARTESIAN_POINT('Ctrl Pts',(-19.6364725931695,-11.9648992312094,
15.));
#34311=CARTESIAN_POINT('Ctrl Pts',(-19.6715045149944,-12.0463570680308,
15.));
#34312=CARTESIAN_POINT('Ctrl Pts',(-19.7060633406705,-12.1282070378972,
15.));
#34313=CARTESIAN_POINT('Ctrl Pts',(-19.7401492304335,-12.2104446447874,
15.));
#34314=CARTESIAN_POINT('Ctrl Pts',(-19.7737622285562,-12.2930652417986,
15.));
#34315=CARTESIAN_POINT('Ctrl Pts',(-19.8069022248387,-12.3760638341708,
15.));
#34316=CARTESIAN_POINT('Ctrl Pts',(-19.839568972011,-12.4594350764989,15.));
#34317=CARTESIAN_POINT('Ctrl Pts',(-19.8717621942733,-12.5431736030595,
15.));
#34318=CARTESIAN_POINT('Ctrl Pts',(-19.9034816813503,-12.6272742843372,
15.));
#34319=CARTESIAN_POINT('Ctrl Pts',(-19.9347273847264,-12.7117325003719,
15.));
#34320=CARTESIAN_POINT('Ctrl Pts',(-19.9654995335894,-12.7965444294443,
15.));
#34321=CARTESIAN_POINT('Ctrl Pts',(-20.0018585267766,-12.8987398182747,
15.));
#34322=CARTESIAN_POINT('Ctrl Pts',(-20.0315673466055,-12.9843387891477,
15.));
#34323=CARTESIAN_POINT('Ctrl Pts',(-20.054957345404,-13.0530957702829,15.));
#34324=CARTESIAN_POINT('Ctrl Pts',(-20.0722879610899,-13.1048196144678,
15.));
#34325=CARTESIAN_POINT('Ctrl Pts',(-20.0837475345526,-13.1393715591102,
15.));
#34326=CARTESIAN_POINT('Ctrl Pts',(-23.9712218930251,-1.17495572484831,
0.));
#34327=CARTESIAN_POINT('Ctrl Pts',(-23.9712218930251,-1.17495572484831,
18.));
#34328=CARTESIAN_POINT('Ctrl Pts',(-23.9564318364582,-1.18556439589231,
0.));
#34329=CARTESIAN_POINT('Ctrl Pts',(-23.9564318364582,-1.18556439589231,
18.));
#34330=CARTESIAN_POINT('Ctrl Pts',(-23.9268340213745,-1.20672599652272,
0.));
#34331=CARTESIAN_POINT('Ctrl Pts',(-23.9268340213745,-1.20672599652272,
18.));
#34332=CARTESIAN_POINT('Ctrl Pts',(-23.8823841929226,-1.2383011730893,0.));
#34333=CARTESIAN_POINT('Ctrl Pts',(-23.8823841929226,-1.2383011730893,18.));
#34334=CARTESIAN_POINT('Ctrl Pts',(-23.8230115078373,-1.28006684869166,
0.));
#34335=CARTESIAN_POINT('Ctrl Pts',(-23.8230115078373,-1.28006684869166,
18.));
#34336=CARTESIAN_POINT('Ctrl Pts',(-23.748618507953,-1.33171549586249,0.));
#34337=CARTESIAN_POINT('Ctrl Pts',(-23.748618507953,-1.33171549586249,18.));
#34338=CARTESIAN_POINT('Ctrl Pts',(-23.6740485197917,-1.38280426780156,
0.));
#34339=CARTESIAN_POINT('Ctrl Pts',(-23.6740485197917,-1.38280426780156,
18.));
#34340=CARTESIAN_POINT('Ctrl Pts',(-23.5993021272808,-1.43333114446389,
0.));
#34341=CARTESIAN_POINT('Ctrl Pts',(-23.5993021272808,-1.43333114446389,
18.));
#34342=CARTESIAN_POINT('Ctrl Pts',(-23.5243805284282,-1.4832935129085,0.));
#34343=CARTESIAN_POINT('Ctrl Pts',(-23.5243805284282,-1.4832935129085,18.));
#34344=CARTESIAN_POINT('Ctrl Pts',(-23.4492857841673,-1.53268814658653,
0.));
#34345=CARTESIAN_POINT('Ctrl Pts',(-23.4492857841673,-1.53268814658653,
18.));
#34346=CARTESIAN_POINT('Ctrl Pts',(-23.3740206492924,-1.58151133638847,
0.));
#34347=CARTESIAN_POINT('Ctrl Pts',(-23.3740206492924,-1.58151133638847,
18.));
#34348=CARTESIAN_POINT('Ctrl Pts',(-23.2985883089733,-1.62975905604583,
0.));
#34349=CARTESIAN_POINT('Ctrl Pts',(-23.2985883089733,-1.62975905604583,
18.));
#34350=CARTESIAN_POINT('Ctrl Pts',(-23.2229921402299,-1.67742712670823,
0.));
#34351=CARTESIAN_POINT('Ctrl Pts',(-23.2229921402299,-1.67742712670823,
18.));
#34352=CARTESIAN_POINT('Ctrl Pts',(-23.1472354850579,-1.72451136919382,
0.));
#34353=CARTESIAN_POINT('Ctrl Pts',(-23.1472354850579,-1.72451136919382,
18.));
#34354=CARTESIAN_POINT('Ctrl Pts',(-23.0713213684573,-1.77100780743078,
0.));
#34355=CARTESIAN_POINT('Ctrl Pts',(-23.0713213684573,-1.77100780743078,
18.));
#34356=CARTESIAN_POINT('Ctrl Pts',(-22.9952524859917,-1.81691265597281,
0.));
#34357=CARTESIAN_POINT('Ctrl Pts',(-22.9952524859917,-1.81691265597281,
18.));
#34358=CARTESIAN_POINT('Ctrl Pts',(-22.9190313507225,-1.86222218327818,
0.));
#34359=CARTESIAN_POINT('Ctrl Pts',(-22.9190313507225,-1.86222218327818,
18.));
#34360=CARTESIAN_POINT('Ctrl Pts',(-22.8426603964871,-1.90693261239855,
0.));
#34361=CARTESIAN_POINT('Ctrl Pts',(-22.8426603964871,-1.90693261239855,
18.));
#34362=CARTESIAN_POINT('Ctrl Pts',(-22.7661420906702,-1.9510400208289,0.));
#34363=CARTESIAN_POINT('Ctrl Pts',(-22.7661420906702,-1.9510400208289,18.));
#34364=CARTESIAN_POINT('Ctrl Pts',(-22.6894790673923,-1.99454021984253,
0.));
#34365=CARTESIAN_POINT('Ctrl Pts',(-22.6894790673923,-1.99454021984253,
18.));
#34366=CARTESIAN_POINT('Ctrl Pts',(-22.6126741632309,-2.03742874317627,
0.));
#34367=CARTESIAN_POINT('Ctrl Pts',(-22.6126741632309,-2.03742874317627,
18.));
#34368=CARTESIAN_POINT('Ctrl Pts',(-22.5357303426251,-2.07970095436223,
0.));
#34369=CARTESIAN_POINT('Ctrl Pts',(-22.5357303426251,-2.07970095436223,
18.));
#34370=CARTESIAN_POINT('Ctrl Pts',(-22.4586506520939,-2.1213521324248,0.));
#34371=CARTESIAN_POINT('Ctrl Pts',(-22.4586506520939,-2.1213521324248,18.));
#34372=CARTESIAN_POINT('Ctrl Pts',(-22.3814381677224,-2.16237755726403,
0.));
#34373=CARTESIAN_POINT('Ctrl Pts',(-22.3814381677224,-2.16237755726403,
18.));
#34374=CARTESIAN_POINT('Ctrl Pts',(-22.3040959372933,-2.20277263221399,
0.));
#34375=CARTESIAN_POINT('Ctrl Pts',(-22.3040959372933,-2.20277263221399,
18.));
#34376=CARTESIAN_POINT('Ctrl Pts',(-22.2266269576315,-2.24253288454712,
0.));
#34377=CARTESIAN_POINT('Ctrl Pts',(-22.2266269576315,-2.24253288454712,
18.));
#34378=CARTESIAN_POINT('Ctrl Pts',(-22.1490342171802,-2.2816537516023,0.));
#34379=CARTESIAN_POINT('Ctrl Pts',(-22.1490342171802,-2.2816537516023,18.));
#34380=CARTESIAN_POINT('Ctrl Pts',(-22.0713207257413,-2.32013040994124,
0.));
#34381=CARTESIAN_POINT('Ctrl Pts',(-22.0713207257413,-2.32013040994124,
18.));
#34382=CARTESIAN_POINT('Ctrl Pts',(-21.9934895476958,-2.35795761145761,
0.));
#34383=CARTESIAN_POINT('Ctrl Pts',(-21.9934895476958,-2.35795761145761,
18.));
#34384=CARTESIAN_POINT('Ctrl Pts',(-21.9155438409279,-2.39512947344577,
0.));
#34385=CARTESIAN_POINT('Ctrl Pts',(-21.9155438409279,-2.39512947344577,
18.));
#34386=CARTESIAN_POINT('Ctrl Pts',(-21.8374868743435,-2.43163944362692,
0.));
#34387=CARTESIAN_POINT('Ctrl Pts',(-21.8374868743435,-2.43163944362692,
18.));
#34388=CARTESIAN_POINT('Ctrl Pts',(-21.7593219872847,-2.46748070362075,
0.));
#34389=CARTESIAN_POINT('Ctrl Pts',(-21.7593219872847,-2.46748070362075,
18.));
#34390=CARTESIAN_POINT('Ctrl Pts',(-21.6810525594039,-2.50264651177234,
0.));
#34391=CARTESIAN_POINT('Ctrl Pts',(-21.6810525594039,-2.50264651177234,
18.));
#34392=CARTESIAN_POINT('Ctrl Pts',(-21.6026819803014,-2.53713053453766,
0.));
#34393=CARTESIAN_POINT('Ctrl Pts',(-21.6026819803014,-2.53713053453766,
18.));
#34394=CARTESIAN_POINT('Ctrl Pts',(-21.5242136128466,-2.5709272835198,0.));
#34395=CARTESIAN_POINT('Ctrl Pts',(-21.5242136128466,-2.5709272835198,18.));
#34396=CARTESIAN_POINT('Ctrl Pts',(-21.4456507822983,-2.60403221866523,
0.));
#34397=CARTESIAN_POINT('Ctrl Pts',(-21.4456507822983,-2.60403221866523,
18.));
#34398=CARTESIAN_POINT('Ctrl Pts',(-21.3669968505594,-2.6364407451853,0.));
#34399=CARTESIAN_POINT('Ctrl Pts',(-21.3669968505594,-2.6364407451853,18.));
#34400=CARTESIAN_POINT('Ctrl Pts',(-21.2882552797978,-2.668147357083,0.));
#34401=CARTESIAN_POINT('Ctrl Pts',(-21.2882552797978,-2.668147357083,18.));
#34402=CARTESIAN_POINT('Ctrl Pts',(-21.2094296949571,-2.69914481283353,
0.));
#34403=CARTESIAN_POINT('Ctrl Pts',(-21.2094296949571,-2.69914481283353,
18.));
#34404=CARTESIAN_POINT('Ctrl Pts',(-21.1305239619219,-2.72942309852119,
0.));
#34405=CARTESIAN_POINT('Ctrl Pts',(-21.1305239619219,-2.72942309852119,
18.));
#34406=CARTESIAN_POINT('Ctrl Pts',(-21.0515422162039,-2.75896910007689,
0.));
#34407=CARTESIAN_POINT('Ctrl Pts',(-21.0515422162039,-2.75896910007689,
18.));
#34408=CARTESIAN_POINT('Ctrl Pts',(-20.9724887103073,-2.78776883747221,
0.));
#34409=CARTESIAN_POINT('Ctrl Pts',(-20.9724887103073,-2.78776883747221,
18.));
#34410=CARTESIAN_POINT('Ctrl Pts',(-20.8933676828246,-2.81580940715317,
0.));
#34411=CARTESIAN_POINT('Ctrl Pts',(-20.8933676828246,-2.81580940715317,
18.));
#34412=CARTESIAN_POINT('Ctrl Pts',(-20.8141832346435,-2.84308082507643,
0.));
#34413=CARTESIAN_POINT('Ctrl Pts',(-20.8141832346435,-2.84308082507643,
18.));
#34414=CARTESIAN_POINT('Ctrl Pts',(-20.7349391669725,-2.86957843933153,
0.));
#34415=CARTESIAN_POINT('Ctrl Pts',(-20.7349391669725,-2.86957843933153,
18.));
#34416=CARTESIAN_POINT('Ctrl Pts',(-20.6556389450993,-2.89530351700805,
0.));
#34417=CARTESIAN_POINT('Ctrl Pts',(-20.6556389450993,-2.89530351700805,
18.));
#34418=CARTESIAN_POINT('Ctrl Pts',(-20.5762860772943,-2.92025778619206,
0.));
#34419=CARTESIAN_POINT('Ctrl Pts',(-20.5762860772943,-2.92025778619206,
18.));
#34420=CARTESIAN_POINT('Ctrl Pts',(-20.4968844460513,-2.94443868035154,
0.));
#34421=CARTESIAN_POINT('Ctrl Pts',(-20.4968844460513,-2.94443868035154,
18.));
#34422=CARTESIAN_POINT('Ctrl Pts',(-20.4174386170774,-2.96783492132513,
0.));
#34423=CARTESIAN_POINT('Ctrl Pts',(-20.4174386170774,-2.96783492132513,
18.));
#34424=CARTESIAN_POINT('Ctrl Pts',(-20.3379542578194,-2.99042050197904,
0.));
#34425=CARTESIAN_POINT('Ctrl Pts',(-20.3379542578194,-2.99042050197904,
18.));
#34426=CARTESIAN_POINT('Ctrl Pts',(-20.2584381977107,-3.01215393913612,
0.));
#34427=CARTESIAN_POINT('Ctrl Pts',(-20.2584381977107,-3.01215393913612,
18.));
#34428=CARTESIAN_POINT('Ctrl Pts',(-20.178897575607,-3.03299094576288,0.));
#34429=CARTESIAN_POINT('Ctrl Pts',(-20.178897575607,-3.03299094576288,18.));
#34430=CARTESIAN_POINT('Ctrl Pts',(-20.0993390992966,-3.0528954575995,0.));
#34431=CARTESIAN_POINT('Ctrl Pts',(-20.0993390992966,-3.0528954575995,18.));
#34432=CARTESIAN_POINT('Ctrl Pts',(-20.0197683853426,-3.07184950717982,
0.));
#34433=CARTESIAN_POINT('Ctrl Pts',(-20.0197683853426,-3.07184950717982,
18.));
#34434=CARTESIAN_POINT('Ctrl Pts',(-19.9401889653541,-3.08986795998319,
0.));
#34435=CARTESIAN_POINT('Ctrl Pts',(-19.9401889653541,-3.08986795998319,
18.));
#34436=CARTESIAN_POINT('Ctrl Pts',(-19.8606024365399,-3.10699659920993,
0.));
#34437=CARTESIAN_POINT('Ctrl Pts',(-19.8606024365399,-3.10699659920993,
18.));
#34438=CARTESIAN_POINT('Ctrl Pts',(-19.7810105986827,-3.12328131323979,
0.));
#34439=CARTESIAN_POINT('Ctrl Pts',(-19.7810105986827,-3.12328131323979,
18.));
#34440=CARTESIAN_POINT('Ctrl Pts',(-19.7014173131304,-3.13874131344865,
0.));
#34441=CARTESIAN_POINT('Ctrl Pts',(-19.7014173131304,-3.13874131344865,
18.));
#34442=CARTESIAN_POINT('Ctrl Pts',(-19.6218301288731,-3.15334580802458,
0.));
#34443=CARTESIAN_POINT('Ctrl Pts',(-19.6218301288731,-3.15334580802458,
18.));
#34444=CARTESIAN_POINT('Ctrl Pts',(-19.5422628528517,-3.16697679689294,
0.));
#34445=CARTESIAN_POINT('Ctrl Pts',(-19.5422628528517,-3.16697679689294,
18.));
#34446=CARTESIAN_POINT('Ctrl Pts',(-19.4627345689632,-3.17944412249753,
0.));
#34447=CARTESIAN_POINT('Ctrl Pts',(-19.4627345689632,-3.17944412249753,
18.));
#34448=CARTESIAN_POINT('Ctrl Pts',(-19.3832648965708,-3.19055618489382,
0.));
#34449=CARTESIAN_POINT('Ctrl Pts',(-19.3832648965708,-3.19055618489382,
18.));
#34450=CARTESIAN_POINT('Ctrl Pts',(-19.3038697977783,-3.20018203702739,
0.));
#34451=CARTESIAN_POINT('Ctrl Pts',(-19.3038697977783,-3.20018203702739,
18.));
#34452=CARTESIAN_POINT('Ctrl Pts',(-19.2245581120423,-3.2083040369031,0.));
#34453=CARTESIAN_POINT('Ctrl Pts',(-19.2245581120423,-3.2083040369031,18.));
#34454=CARTESIAN_POINT('Ctrl Pts',(-19.1453253990185,-3.21510704576116,
0.));
#34455=CARTESIAN_POINT('Ctrl Pts',(-19.1453253990185,-3.21510704576116,
18.));
#34456=CARTESIAN_POINT('Ctrl Pts',(-19.0661599344864,-3.22090173651084,
0.));
#34457=CARTESIAN_POINT('Ctrl Pts',(-19.0661599344864,-3.22090173651084,
18.));
#34458=CARTESIAN_POINT('Ctrl Pts',(-18.987055820781,-3.22595008773714,0.));
#34459=CARTESIAN_POINT('Ctrl Pts',(-18.987055820781,-3.22595008773714,18.));
#34460=CARTESIAN_POINT('Ctrl Pts',(-18.908024664264,-3.23031169402938,0.));
#34461=CARTESIAN_POINT('Ctrl Pts',(-18.908024664264,-3.23031169402938,18.));
#34462=CARTESIAN_POINT('Ctrl Pts',(-18.8291062617862,-3.23370091065669,
0.));
#34463=CARTESIAN_POINT('Ctrl Pts',(-18.8291062617862,-3.23370091065669,
18.));
#34464=CARTESIAN_POINT('Ctrl Pts',(-18.7503838921122,-3.23528809328096,
0.));
#34465=CARTESIAN_POINT('Ctrl Pts',(-18.7503838921122,-3.23528809328096,
18.));
#34466=CARTESIAN_POINT('Ctrl Pts',(-18.6719665316945,-3.23390622002644,
0.));
#34467=CARTESIAN_POINT('Ctrl Pts',(-18.6719665316945,-3.23390622002644,
18.));
#34468=CARTESIAN_POINT('Ctrl Pts',(-18.6095634206219,-3.2294700044416,0.));
#34469=CARTESIAN_POINT('Ctrl Pts',(-18.6095634206219,-3.2294700044416,18.));
#34470=CARTESIAN_POINT('Ctrl Pts',(-18.5629852384321,-3.22384302136591,
0.));
#34471=CARTESIAN_POINT('Ctrl Pts',(-18.5629852384321,-3.22384302136591,
18.));
#34472=CARTESIAN_POINT('Ctrl Pts',(-18.5320375674878,-3.2190148958593,0.));
#34473=CARTESIAN_POINT('Ctrl Pts',(-18.5320375674878,-3.2190148958593,18.));
#34474=CARTESIAN_POINT('Ctrl Pts',(-18.5165898451125,-3.21633162650739,
0.));
#34475=CARTESIAN_POINT('Ctrl Pts',(-18.5165898451125,-3.21633162650739,
18.));
#34476=CARTESIAN_POINT('',(-23.9712218930251,-1.17495572484826,0.));
#34477=CARTESIAN_POINT('Ctrl Pts',(-18.5165898451125,-3.21633162650739,
0.));
#34478=CARTESIAN_POINT('Ctrl Pts',(-18.5320375674878,-3.2190148958593,0.));
#34479=CARTESIAN_POINT('Ctrl Pts',(-18.5629852384321,-3.22384302136591,
0.));
#34480=CARTESIAN_POINT('Ctrl Pts',(-18.6095634206219,-3.2294700044416,0.));
#34481=CARTESIAN_POINT('Ctrl Pts',(-18.6719665316945,-3.23390622002644,
0.));
#34482=CARTESIAN_POINT('Ctrl Pts',(-18.7503838921122,-3.23528809328096,
0.));
#34483=CARTESIAN_POINT('Ctrl Pts',(-18.8291062617862,-3.23370091065669,
0.));
#34484=CARTESIAN_POINT('Ctrl Pts',(-18.908024664264,-3.23031169402938,0.));
#34485=CARTESIAN_POINT('Ctrl Pts',(-18.987055820781,-3.22595008773714,0.));
#34486=CARTESIAN_POINT('Ctrl Pts',(-19.0661599344864,-3.22090173651084,
0.));
#34487=CARTESIAN_POINT('Ctrl Pts',(-19.1453253990185,-3.21510704576116,
0.));
#34488=CARTESIAN_POINT('Ctrl Pts',(-19.2245581120423,-3.2083040369031,0.));
#34489=CARTESIAN_POINT('Ctrl Pts',(-19.3038697977783,-3.20018203702739,
0.));
#34490=CARTESIAN_POINT('Ctrl Pts',(-19.3832648965708,-3.19055618489382,
0.));
#34491=CARTESIAN_POINT('Ctrl Pts',(-19.4627345689632,-3.17944412249753,
0.));
#34492=CARTESIAN_POINT('Ctrl Pts',(-19.5422628528517,-3.16697679689294,
0.));
#34493=CARTESIAN_POINT('Ctrl Pts',(-19.6218301288731,-3.15334580802458,
0.));
#34494=CARTESIAN_POINT('Ctrl Pts',(-19.7014173131304,-3.13874131344865,
0.));
#34495=CARTESIAN_POINT('Ctrl Pts',(-19.7810105986827,-3.12328131323979,
0.));
#34496=CARTESIAN_POINT('Ctrl Pts',(-19.8606024365399,-3.10699659920993,
0.));
#34497=CARTESIAN_POINT('Ctrl Pts',(-19.9401889653541,-3.08986795998319,
0.));
#34498=CARTESIAN_POINT('Ctrl Pts',(-20.0197683853426,-3.07184950717982,
0.));
#34499=CARTESIAN_POINT('Ctrl Pts',(-20.0993390992966,-3.0528954575995,0.));
#34500=CARTESIAN_POINT('Ctrl Pts',(-20.178897575607,-3.03299094576288,0.));
#34501=CARTESIAN_POINT('Ctrl Pts',(-20.2584381977107,-3.01215393913612,
0.));
#34502=CARTESIAN_POINT('Ctrl Pts',(-20.3379542578194,-2.99042050197904,
0.));
#34503=CARTESIAN_POINT('Ctrl Pts',(-20.4174386170774,-2.96783492132513,
0.));
#34504=CARTESIAN_POINT('Ctrl Pts',(-20.4968844460513,-2.94443868035154,
0.));
#34505=CARTESIAN_POINT('Ctrl Pts',(-20.5762860772943,-2.92025778619206,
0.));
#34506=CARTESIAN_POINT('Ctrl Pts',(-20.6556389450993,-2.89530351700805,
0.));
#34507=CARTESIAN_POINT('Ctrl Pts',(-20.7349391669725,-2.86957843933153,
0.));
#34508=CARTESIAN_POINT('Ctrl Pts',(-20.8141832346435,-2.84308082507643,
0.));
#34509=CARTESIAN_POINT('Ctrl Pts',(-20.8933676828246,-2.81580940715317,
0.));
#34510=CARTESIAN_POINT('Ctrl Pts',(-20.9724887103073,-2.78776883747221,
0.));
#34511=CARTESIAN_POINT('Ctrl Pts',(-21.0515422162039,-2.75896910007689,
0.));
#34512=CARTESIAN_POINT('Ctrl Pts',(-21.1305239619219,-2.72942309852119,
0.));
#34513=CARTESIAN_POINT('Ctrl Pts',(-21.2094296949571,-2.69914481283353,
0.));
#34514=CARTESIAN_POINT('Ctrl Pts',(-21.2882552797978,-2.668147357083,0.));
#34515=CARTESIAN_POINT('Ctrl Pts',(-21.3669968505594,-2.6364407451853,0.));
#34516=CARTESIAN_POINT('Ctrl Pts',(-21.4456507822983,-2.60403221866523,
0.));
#34517=CARTESIAN_POINT('Ctrl Pts',(-21.5242136128466,-2.5709272835198,0.));
#34518=CARTESIAN_POINT('Ctrl Pts',(-21.6026819803014,-2.53713053453766,
0.));
#34519=CARTESIAN_POINT('Ctrl Pts',(-21.6810525594039,-2.50264651177234,
0.));
#34520=CARTESIAN_POINT('Ctrl Pts',(-21.7593219872847,-2.46748070362075,
0.));
#34521=CARTESIAN_POINT('Ctrl Pts',(-21.8374868743435,-2.43163944362692,
0.));
#34522=CARTESIAN_POINT('Ctrl Pts',(-21.9155438409279,-2.39512947344577,
0.));
#34523=CARTESIAN_POINT('Ctrl Pts',(-21.9934895476958,-2.35795761145761,
0.));
#34524=CARTESIAN_POINT('Ctrl Pts',(-22.0713207257413,-2.32013040994124,
0.));
#34525=CARTESIAN_POINT('Ctrl Pts',(-22.1490342171802,-2.2816537516023,0.));
#34526=CARTESIAN_POINT('Ctrl Pts',(-22.2266269576315,-2.24253288454712,
0.));
#34527=CARTESIAN_POINT('Ctrl Pts',(-22.3040959372933,-2.20277263221399,
0.));
#34528=CARTESIAN_POINT('Ctrl Pts',(-22.3814381677224,-2.16237755726403,
0.));
#34529=CARTESIAN_POINT('Ctrl Pts',(-22.4586506520939,-2.1213521324248,0.));
#34530=CARTESIAN_POINT('Ctrl Pts',(-22.5357303426251,-2.07970095436223,
0.));
#34531=CARTESIAN_POINT('Ctrl Pts',(-22.6126741632309,-2.03742874317627,
0.));
#34532=CARTESIAN_POINT('Ctrl Pts',(-22.6894790673923,-1.99454021984253,
0.));
#34533=CARTESIAN_POINT('Ctrl Pts',(-22.7661420906702,-1.9510400208289,0.));
#34534=CARTESIAN_POINT('Ctrl Pts',(-22.8426603964871,-1.90693261239855,
0.));
#34535=CARTESIAN_POINT('Ctrl Pts',(-22.9190313507225,-1.86222218327818,
0.));
#34536=CARTESIAN_POINT('Ctrl Pts',(-22.9952524859917,-1.81691265597281,
0.));
#34537=CARTESIAN_POINT('Ctrl Pts',(-23.0713213684573,-1.77100780743078,
0.));
#34538=CARTESIAN_POINT('Ctrl Pts',(-23.1472354850579,-1.72451136919382,
0.));
#34539=CARTESIAN_POINT('Ctrl Pts',(-23.2229921402299,-1.67742712670823,
0.));
#34540=CARTESIAN_POINT('Ctrl Pts',(-23.2985883089733,-1.62975905604583,
0.));
#34541=CARTESIAN_POINT('Ctrl Pts',(-23.3740206492924,-1.58151133638847,
0.));
#34542=CARTESIAN_POINT('Ctrl Pts',(-23.4492857841673,-1.53268814658653,
0.));
#34543=CARTESIAN_POINT('Ctrl Pts',(-23.5243805284282,-1.4832935129085,0.));
#34544=CARTESIAN_POINT('Ctrl Pts',(-23.5993021272808,-1.43333114446389,
0.));
#34545=CARTESIAN_POINT('Ctrl Pts',(-23.6740485197917,-1.38280426780156,
0.));
#34546=CARTESIAN_POINT('Ctrl Pts',(-23.7635325055853,-1.32149774147467,
0.));
#34547=CARTESIAN_POINT('Ctrl Pts',(-23.8378812584003,-1.2697091254959,0.));
#34548=CARTESIAN_POINT('Ctrl Pts',(-23.89721850443,-1.22783185562043,0.));
#34549=CARTESIAN_POINT('Ctrl Pts',(-23.9416417798467,-1.19617306697386,
0.));
#34550=CARTESIAN_POINT('Ctrl Pts',(-23.9712218930251,-1.17495572484831,
0.));
#34551=CARTESIAN_POINT('',(-23.9712218930251,-1.17495572484826,15.));
#34552=CARTESIAN_POINT('Ctrl Pts',(-23.9712218930251,-1.17495572484831,
15.));
#34553=CARTESIAN_POINT('Ctrl Pts',(-23.9564318364582,-1.18556439589231,
15.));
#34554=CARTESIAN_POINT('Ctrl Pts',(-23.9268340213745,-1.20672599652272,
15.));
#34555=CARTESIAN_POINT('Ctrl Pts',(-23.8823841929226,-1.2383011730893,15.));
#34556=CARTESIAN_POINT('Ctrl Pts',(-23.8230115078373,-1.28006684869166,
15.));
#34557=CARTESIAN_POINT('Ctrl Pts',(-23.748618507953,-1.33171549586249,15.));
#34558=CARTESIAN_POINT('Ctrl Pts',(-23.6740485197917,-1.38280426780156,
15.));
#34559=CARTESIAN_POINT('Ctrl Pts',(-23.5993021272808,-1.43333114446389,
15.));
#34560=CARTESIAN_POINT('Ctrl Pts',(-23.5243805284282,-1.4832935129085,15.));
#34561=CARTESIAN_POINT('Ctrl Pts',(-23.4492857841673,-1.53268814658653,
15.));
#34562=CARTESIAN_POINT('Ctrl Pts',(-23.3740206492924,-1.58151133638847,
15.));
#34563=CARTESIAN_POINT('Ctrl Pts',(-23.2985883089733,-1.62975905604583,
15.));
#34564=CARTESIAN_POINT('Ctrl Pts',(-23.2229921402299,-1.67742712670823,
15.));
#34565=CARTESIAN_POINT('Ctrl Pts',(-23.1472354850579,-1.72451136919382,
15.));
#34566=CARTESIAN_POINT('Ctrl Pts',(-23.0713213684573,-1.77100780743078,
15.));
#34567=CARTESIAN_POINT('Ctrl Pts',(-22.9952524859917,-1.81691265597281,
15.));
#34568=CARTESIAN_POINT('Ctrl Pts',(-22.9190313507225,-1.86222218327818,
15.));
#34569=CARTESIAN_POINT('Ctrl Pts',(-22.8426603964871,-1.90693261239855,
15.));
#34570=CARTESIAN_POINT('Ctrl Pts',(-22.7661420906702,-1.9510400208289,15.));
#34571=CARTESIAN_POINT('Ctrl Pts',(-22.6894790673923,-1.99454021984253,
15.));
#34572=CARTESIAN_POINT('Ctrl Pts',(-22.6126741632309,-2.03742874317627,
15.));
#34573=CARTESIAN_POINT('Ctrl Pts',(-22.5357303426251,-2.07970095436223,
15.));
#34574=CARTESIAN_POINT('Ctrl Pts',(-22.4586506520939,-2.1213521324248,15.));
#34575=CARTESIAN_POINT('Ctrl Pts',(-22.3814381677224,-2.16237755726403,
15.));
#34576=CARTESIAN_POINT('Ctrl Pts',(-22.3040959372933,-2.20277263221399,
15.));
#34577=CARTESIAN_POINT('Ctrl Pts',(-22.2266269576315,-2.24253288454712,
15.));
#34578=CARTESIAN_POINT('Ctrl Pts',(-22.1490342171802,-2.2816537516023,15.));
#34579=CARTESIAN_POINT('Ctrl Pts',(-22.0713207257413,-2.32013040994124,
15.));
#34580=CARTESIAN_POINT('Ctrl Pts',(-21.9934895476958,-2.35795761145761,
15.));
#34581=CARTESIAN_POINT('Ctrl Pts',(-21.9155438409279,-2.39512947344577,
15.));
#34582=CARTESIAN_POINT('Ctrl Pts',(-21.8374868743435,-2.43163944362692,
15.));
#34583=CARTESIAN_POINT('Ctrl Pts',(-21.7593219872847,-2.46748070362075,
15.));
#34584=CARTESIAN_POINT('Ctrl Pts',(-21.6810525594039,-2.50264651177234,
15.));
#34585=CARTESIAN_POINT('Ctrl Pts',(-21.6026819803014,-2.53713053453766,
15.));
#34586=CARTESIAN_POINT('Ctrl Pts',(-21.5242136128466,-2.5709272835198,15.));
#34587=CARTESIAN_POINT('Ctrl Pts',(-21.4456507822983,-2.60403221866523,
15.));
#34588=CARTESIAN_POINT('Ctrl Pts',(-21.3669968505594,-2.6364407451853,15.));
#34589=CARTESIAN_POINT('Ctrl Pts',(-21.2882552797978,-2.668147357083,15.));
#34590=CARTESIAN_POINT('Ctrl Pts',(-21.2094296949571,-2.69914481283353,
15.));
#34591=CARTESIAN_POINT('Ctrl Pts',(-21.1305239619219,-2.72942309852119,
15.));
#34592=CARTESIAN_POINT('Ctrl Pts',(-21.0515422162039,-2.75896910007689,
15.));
#34593=CARTESIAN_POINT('Ctrl Pts',(-20.9724887103073,-2.78776883747221,
15.));
#34594=CARTESIAN_POINT('Ctrl Pts',(-20.8933676828246,-2.81580940715317,
15.));
#34595=CARTESIAN_POINT('Ctrl Pts',(-20.8141832346435,-2.84308082507643,
15.));
#34596=CARTESIAN_POINT('Ctrl Pts',(-20.7349391669725,-2.86957843933153,
15.));
#34597=CARTESIAN_POINT('Ctrl Pts',(-20.6556389450993,-2.89530351700805,
15.));
#34598=CARTESIAN_POINT('Ctrl Pts',(-20.5762860772943,-2.92025778619206,
15.));
#34599=CARTESIAN_POINT('Ctrl Pts',(-20.4968844460513,-2.94443868035154,
15.));
#34600=CARTESIAN_POINT('Ctrl Pts',(-20.4174386170774,-2.96783492132513,
15.));
#34601=CARTESIAN_POINT('Ctrl Pts',(-20.3379542578194,-2.99042050197904,
15.));
#34602=CARTESIAN_POINT('Ctrl Pts',(-20.2584381977107,-3.01215393913612,
15.));
#34603=CARTESIAN_POINT('Ctrl Pts',(-20.178897575607,-3.03299094576288,15.));
#34604=CARTESIAN_POINT('Ctrl Pts',(-20.0993390992966,-3.0528954575995,15.));
#34605=CARTESIAN_POINT('Ctrl Pts',(-20.0197683853426,-3.07184950717982,
15.));
#34606=CARTESIAN_POINT('Ctrl Pts',(-19.9401889653541,-3.08986795998319,
15.));
#34607=CARTESIAN_POINT('Ctrl Pts',(-19.8606024365399,-3.10699659920993,
15.));
#34608=CARTESIAN_POINT('Ctrl Pts',(-19.7810105986827,-3.12328131323979,
15.));
#34609=CARTESIAN_POINT('Ctrl Pts',(-19.7014173131304,-3.13874131344865,
15.));
#34610=CARTESIAN_POINT('Ctrl Pts',(-19.6218301288731,-3.15334580802458,
15.));
#34611=CARTESIAN_POINT('Ctrl Pts',(-19.5422628528517,-3.16697679689294,
15.));
#34612=CARTESIAN_POINT('Ctrl Pts',(-19.4627345689632,-3.17944412249753,
15.));
#34613=CARTESIAN_POINT('Ctrl Pts',(-19.3832648965708,-3.19055618489382,
15.));
#34614=CARTESIAN_POINT('Ctrl Pts',(-19.3038697977783,-3.20018203702739,
15.));
#34615=CARTESIAN_POINT('Ctrl Pts',(-19.2245581120423,-3.2083040369031,15.));
#34616=CARTESIAN_POINT('Ctrl Pts',(-19.1453253990185,-3.21510704576116,
15.));
#34617=CARTESIAN_POINT('Ctrl Pts',(-19.0661599344864,-3.22090173651084,
15.));
#34618=CARTESIAN_POINT('Ctrl Pts',(-18.987055820781,-3.22595008773714,15.));
#34619=CARTESIAN_POINT('Ctrl Pts',(-18.908024664264,-3.23031169402938,15.));
#34620=CARTESIAN_POINT('Ctrl Pts',(-18.8291062617862,-3.23370091065669,
15.));
#34621=CARTESIAN_POINT('Ctrl Pts',(-18.7503838921122,-3.23528809328096,
15.));
#34622=CARTESIAN_POINT('Ctrl Pts',(-18.6719665316945,-3.23390622002644,
15.));
#34623=CARTESIAN_POINT('Ctrl Pts',(-18.6095634206219,-3.2294700044416,15.));
#34624=CARTESIAN_POINT('Ctrl Pts',(-18.5629852384321,-3.22384302136591,
15.));
#34625=CARTESIAN_POINT('Ctrl Pts',(-18.5320375674878,-3.2190148958593,15.));
#34626=CARTESIAN_POINT('Ctrl Pts',(-18.5165898451125,-3.21633162650739,
15.));
#34627=CARTESIAN_POINT('',(-23.9712218930251,-1.17495572484826,0.));
#34628=CARTESIAN_POINT('Origin',(-1.15463194561016E-13,6.93889390390802E-17,
0.));
#34629=CARTESIAN_POINT('',(-23.9712218930251,1.17495572484832,0.));
#34630=CARTESIAN_POINT('Origin',(-1.15463194561016E-13,6.93889390390802E-17,
0.));
#34631=CARTESIAN_POINT('',(-23.9712218930251,1.17495572484832,15.));
#34632=CARTESIAN_POINT('Origin',(-1.15463194561016E-13,6.93889390390802E-17,
15.));
#34633=CARTESIAN_POINT('',(-23.9712218930251,1.17495572484832,0.));
#34634=CARTESIAN_POINT('Ctrl Pts',(-18.5165898451125,3.2163316265074,0.));
#34635=CARTESIAN_POINT('Ctrl Pts',(-18.5165898451125,3.2163316265074,18.));
#34636=CARTESIAN_POINT('Ctrl Pts',(-18.5320375674878,3.21901489585931,0.));
#34637=CARTESIAN_POINT('Ctrl Pts',(-18.5320375674878,3.21901489585931,18.));
#34638=CARTESIAN_POINT('Ctrl Pts',(-18.5629852384321,3.22384302136592,0.));
#34639=CARTESIAN_POINT('Ctrl Pts',(-18.5629852384321,3.22384302136592,18.));
#34640=CARTESIAN_POINT('Ctrl Pts',(-18.6095634206219,3.22947000444161,0.));
#34641=CARTESIAN_POINT('Ctrl Pts',(-18.6095634206219,3.22947000444161,18.));
#34642=CARTESIAN_POINT('Ctrl Pts',(-18.6719665316945,3.23390622002644,0.));
#34643=CARTESIAN_POINT('Ctrl Pts',(-18.6719665316945,3.23390622002644,18.));
#34644=CARTESIAN_POINT('Ctrl Pts',(-18.7503838921122,3.23528809328097,0.));
#34645=CARTESIAN_POINT('Ctrl Pts',(-18.7503838921122,3.23528809328097,18.));
#34646=CARTESIAN_POINT('Ctrl Pts',(-18.8291062617862,3.2337009106567,0.));
#34647=CARTESIAN_POINT('Ctrl Pts',(-18.8291062617862,3.2337009106567,18.));
#34648=CARTESIAN_POINT('Ctrl Pts',(-18.908024664264,3.23031169402939,0.));
#34649=CARTESIAN_POINT('Ctrl Pts',(-18.908024664264,3.23031169402939,18.));
#34650=CARTESIAN_POINT('Ctrl Pts',(-18.987055820781,3.22595008773715,0.));
#34651=CARTESIAN_POINT('Ctrl Pts',(-18.987055820781,3.22595008773715,18.));
#34652=CARTESIAN_POINT('Ctrl Pts',(-19.0661599344864,3.22090173651085,0.));
#34653=CARTESIAN_POINT('Ctrl Pts',(-19.0661599344864,3.22090173651085,18.));
#34654=CARTESIAN_POINT('Ctrl Pts',(-19.1453253990185,3.21510704576117,0.));
#34655=CARTESIAN_POINT('Ctrl Pts',(-19.1453253990185,3.21510704576117,18.));
#34656=CARTESIAN_POINT('Ctrl Pts',(-19.2245581120423,3.2083040369031,0.));
#34657=CARTESIAN_POINT('Ctrl Pts',(-19.2245581120423,3.2083040369031,18.));
#34658=CARTESIAN_POINT('Ctrl Pts',(-19.3038697977783,3.2001820370274,0.));
#34659=CARTESIAN_POINT('Ctrl Pts',(-19.3038697977783,3.2001820370274,18.));
#34660=CARTESIAN_POINT('Ctrl Pts',(-19.3832648965708,3.19055618489382,0.));
#34661=CARTESIAN_POINT('Ctrl Pts',(-19.3832648965708,3.19055618489382,18.));
#34662=CARTESIAN_POINT('Ctrl Pts',(-19.4627345689632,3.17944412249754,0.));
#34663=CARTESIAN_POINT('Ctrl Pts',(-19.4627345689632,3.17944412249754,18.));
#34664=CARTESIAN_POINT('Ctrl Pts',(-19.5422628528517,3.16697679689295,0.));
#34665=CARTESIAN_POINT('Ctrl Pts',(-19.5422628528517,3.16697679689295,18.));
#34666=CARTESIAN_POINT('Ctrl Pts',(-19.6218301288731,3.15334580802458,0.));
#34667=CARTESIAN_POINT('Ctrl Pts',(-19.6218301288731,3.15334580802458,18.));
#34668=CARTESIAN_POINT('Ctrl Pts',(-19.7014173131304,3.13874131344865,0.));
#34669=CARTESIAN_POINT('Ctrl Pts',(-19.7014173131304,3.13874131344865,18.));
#34670=CARTESIAN_POINT('Ctrl Pts',(-19.7810105986827,3.1232813132398,0.));
#34671=CARTESIAN_POINT('Ctrl Pts',(-19.7810105986827,3.1232813132398,18.));
#34672=CARTESIAN_POINT('Ctrl Pts',(-19.8606024365399,3.10699659920993,0.));
#34673=CARTESIAN_POINT('Ctrl Pts',(-19.8606024365399,3.10699659920993,18.));
#34674=CARTESIAN_POINT('Ctrl Pts',(-19.940188965354,3.08986795998319,0.));
#34675=CARTESIAN_POINT('Ctrl Pts',(-19.940188965354,3.08986795998319,18.));
#34676=CARTESIAN_POINT('Ctrl Pts',(-20.0197683853426,3.07184950717982,0.));
#34677=CARTESIAN_POINT('Ctrl Pts',(-20.0197683853426,3.07184950717982,18.));
#34678=CARTESIAN_POINT('Ctrl Pts',(-20.0993390992966,3.05289545759951,0.));
#34679=CARTESIAN_POINT('Ctrl Pts',(-20.0993390992966,3.05289545759951,18.));
#34680=CARTESIAN_POINT('Ctrl Pts',(-20.178897575607,3.03299094576289,0.));
#34681=CARTESIAN_POINT('Ctrl Pts',(-20.178897575607,3.03299094576289,18.));
#34682=CARTESIAN_POINT('Ctrl Pts',(-20.2584381977107,3.01215393913612,0.));
#34683=CARTESIAN_POINT('Ctrl Pts',(-20.2584381977107,3.01215393913612,18.));
#34684=CARTESIAN_POINT('Ctrl Pts',(-20.3379542578194,2.99042050197905,0.));
#34685=CARTESIAN_POINT('Ctrl Pts',(-20.3379542578194,2.99042050197905,18.));
#34686=CARTESIAN_POINT('Ctrl Pts',(-20.4174386170774,2.96783492132513,0.));
#34687=CARTESIAN_POINT('Ctrl Pts',(-20.4174386170774,2.96783492132513,18.));
#34688=CARTESIAN_POINT('Ctrl Pts',(-20.4968844460513,2.94443868035155,0.));
#34689=CARTESIAN_POINT('Ctrl Pts',(-20.4968844460513,2.94443868035155,18.));
#34690=CARTESIAN_POINT('Ctrl Pts',(-20.5762860772943,2.92025778619207,0.));
#34691=CARTESIAN_POINT('Ctrl Pts',(-20.5762860772943,2.92025778619207,18.));
#34692=CARTESIAN_POINT('Ctrl Pts',(-20.6556389450993,2.89530351700806,0.));
#34693=CARTESIAN_POINT('Ctrl Pts',(-20.6556389450993,2.89530351700806,18.));
#34694=CARTESIAN_POINT('Ctrl Pts',(-20.7349391669725,2.86957843933153,0.));
#34695=CARTESIAN_POINT('Ctrl Pts',(-20.7349391669725,2.86957843933153,18.));
#34696=CARTESIAN_POINT('Ctrl Pts',(-20.8141832346435,2.84308082507644,0.));
#34697=CARTESIAN_POINT('Ctrl Pts',(-20.8141832346435,2.84308082507644,18.));
#34698=CARTESIAN_POINT('Ctrl Pts',(-20.8933676828246,2.81580940715318,0.));
#34699=CARTESIAN_POINT('Ctrl Pts',(-20.8933676828246,2.81580940715318,18.));
#34700=CARTESIAN_POINT('Ctrl Pts',(-20.9724887103073,2.78776883747222,0.));
#34701=CARTESIAN_POINT('Ctrl Pts',(-20.9724887103073,2.78776883747222,18.));
#34702=CARTESIAN_POINT('Ctrl Pts',(-21.0515422162039,2.7589691000769,0.));
#34703=CARTESIAN_POINT('Ctrl Pts',(-21.0515422162039,2.7589691000769,18.));
#34704=CARTESIAN_POINT('Ctrl Pts',(-21.1305239619219,2.72942309852119,0.));
#34705=CARTESIAN_POINT('Ctrl Pts',(-21.1305239619219,2.72942309852119,18.));
#34706=CARTESIAN_POINT('Ctrl Pts',(-21.2094296949571,2.69914481283353,0.));
#34707=CARTESIAN_POINT('Ctrl Pts',(-21.2094296949571,2.69914481283353,18.));
#34708=CARTESIAN_POINT('Ctrl Pts',(-21.2882552797978,2.66814735708301,0.));
#34709=CARTESIAN_POINT('Ctrl Pts',(-21.2882552797978,2.66814735708301,18.));
#34710=CARTESIAN_POINT('Ctrl Pts',(-21.3669968505594,2.6364407451853,0.));
#34711=CARTESIAN_POINT('Ctrl Pts',(-21.3669968505594,2.6364407451853,18.));
#34712=CARTESIAN_POINT('Ctrl Pts',(-21.4456507822983,2.60403221866524,0.));
#34713=CARTESIAN_POINT('Ctrl Pts',(-21.4456507822983,2.60403221866524,18.));
#34714=CARTESIAN_POINT('Ctrl Pts',(-21.5242136128466,2.57092728351981,0.));
#34715=CARTESIAN_POINT('Ctrl Pts',(-21.5242136128466,2.57092728351981,18.));
#34716=CARTESIAN_POINT('Ctrl Pts',(-21.6026819803014,2.53713053453767,0.));
#34717=CARTESIAN_POINT('Ctrl Pts',(-21.6026819803014,2.53713053453767,18.));
#34718=CARTESIAN_POINT('Ctrl Pts',(-21.6810525594039,2.50264651177235,0.));
#34719=CARTESIAN_POINT('Ctrl Pts',(-21.6810525594039,2.50264651177235,18.));
#34720=CARTESIAN_POINT('Ctrl Pts',(-21.7593219872847,2.46748070362076,0.));
#34721=CARTESIAN_POINT('Ctrl Pts',(-21.7593219872847,2.46748070362076,18.));
#34722=CARTESIAN_POINT('Ctrl Pts',(-21.8374868743435,2.43163944362692,0.));
#34723=CARTESIAN_POINT('Ctrl Pts',(-21.8374868743435,2.43163944362692,18.));
#34724=CARTESIAN_POINT('Ctrl Pts',(-21.9155438409279,2.39512947344577,0.));
#34725=CARTESIAN_POINT('Ctrl Pts',(-21.9155438409279,2.39512947344577,18.));
#34726=CARTESIAN_POINT('Ctrl Pts',(-21.9934895476958,2.35795761145762,0.));
#34727=CARTESIAN_POINT('Ctrl Pts',(-21.9934895476958,2.35795761145762,18.));
#34728=CARTESIAN_POINT('Ctrl Pts',(-22.0713207257413,2.32013040994125,0.));
#34729=CARTESIAN_POINT('Ctrl Pts',(-22.0713207257413,2.32013040994125,18.));
#34730=CARTESIAN_POINT('Ctrl Pts',(-22.1490342171802,2.28165375160231,0.));
#34731=CARTESIAN_POINT('Ctrl Pts',(-22.1490342171802,2.28165375160231,18.));
#34732=CARTESIAN_POINT('Ctrl Pts',(-22.2266269576315,2.24253288454712,0.));
#34733=CARTESIAN_POINT('Ctrl Pts',(-22.2266269576315,2.24253288454712,18.));
#34734=CARTESIAN_POINT('Ctrl Pts',(-22.3040959372933,2.202772632214,0.));
#34735=CARTESIAN_POINT('Ctrl Pts',(-22.3040959372933,2.202772632214,18.));
#34736=CARTESIAN_POINT('Ctrl Pts',(-22.3814381677224,2.16237755726405,0.));
#34737=CARTESIAN_POINT('Ctrl Pts',(-22.3814381677224,2.16237755726405,18.));
#34738=CARTESIAN_POINT('Ctrl Pts',(-22.4586506520939,2.1213521324248,0.));
#34739=CARTESIAN_POINT('Ctrl Pts',(-22.4586506520939,2.1213521324248,18.));
#34740=CARTESIAN_POINT('Ctrl Pts',(-22.5357303426251,2.07970095436224,0.));
#34741=CARTESIAN_POINT('Ctrl Pts',(-22.5357303426251,2.07970095436224,18.));
#34742=CARTESIAN_POINT('Ctrl Pts',(-22.6126741632309,2.03742874317627,0.));
#34743=CARTESIAN_POINT('Ctrl Pts',(-22.6126741632309,2.03742874317627,18.));
#34744=CARTESIAN_POINT('Ctrl Pts',(-22.6894790673923,1.99454021984253,0.));
#34745=CARTESIAN_POINT('Ctrl Pts',(-22.6894790673923,1.99454021984253,18.));
#34746=CARTESIAN_POINT('Ctrl Pts',(-22.7661420906702,1.95104002082891,0.));
#34747=CARTESIAN_POINT('Ctrl Pts',(-22.7661420906702,1.95104002082891,18.));
#34748=CARTESIAN_POINT('Ctrl Pts',(-22.8426603964871,1.90693261239855,0.));
#34749=CARTESIAN_POINT('Ctrl Pts',(-22.8426603964871,1.90693261239855,18.));
#34750=CARTESIAN_POINT('Ctrl Pts',(-22.9190313507225,1.86222218327819,0.));
#34751=CARTESIAN_POINT('Ctrl Pts',(-22.9190313507225,1.86222218327819,18.));
#34752=CARTESIAN_POINT('Ctrl Pts',(-22.9952524859917,1.81691265597282,0.));
#34753=CARTESIAN_POINT('Ctrl Pts',(-22.9952524859917,1.81691265597282,18.));
#34754=CARTESIAN_POINT('Ctrl Pts',(-23.0713213684573,1.77100780743078,0.));
#34755=CARTESIAN_POINT('Ctrl Pts',(-23.0713213684573,1.77100780743078,18.));
#34756=CARTESIAN_POINT('Ctrl Pts',(-23.1472354850579,1.72451136919382,0.));
#34757=CARTESIAN_POINT('Ctrl Pts',(-23.1472354850579,1.72451136919382,18.));
#34758=CARTESIAN_POINT('Ctrl Pts',(-23.2229921402299,1.67742712670823,0.));
#34759=CARTESIAN_POINT('Ctrl Pts',(-23.2229921402299,1.67742712670823,18.));
#34760=CARTESIAN_POINT('Ctrl Pts',(-23.2985883089733,1.62975905604583,0.));
#34761=CARTESIAN_POINT('Ctrl Pts',(-23.2985883089733,1.62975905604583,18.));
#34762=CARTESIAN_POINT('Ctrl Pts',(-23.3740206492924,1.58151133638848,0.));
#34763=CARTESIAN_POINT('Ctrl Pts',(-23.3740206492924,1.58151133638848,18.));
#34764=CARTESIAN_POINT('Ctrl Pts',(-23.4492857841673,1.53268814658653,0.));
#34765=CARTESIAN_POINT('Ctrl Pts',(-23.4492857841673,1.53268814658653,18.));
#34766=CARTESIAN_POINT('Ctrl Pts',(-23.5243805284282,1.48329351290851,0.));
#34767=CARTESIAN_POINT('Ctrl Pts',(-23.5243805284282,1.48329351290851,18.));
#34768=CARTESIAN_POINT('Ctrl Pts',(-23.5993021272808,1.4333311444639,0.));
#34769=CARTESIAN_POINT('Ctrl Pts',(-23.5993021272808,1.4333311444639,18.));
#34770=CARTESIAN_POINT('Ctrl Pts',(-23.6740485197917,1.38280426780156,0.));
#34771=CARTESIAN_POINT('Ctrl Pts',(-23.6740485197917,1.38280426780156,18.));
#34772=CARTESIAN_POINT('Ctrl Pts',(-23.748618507953,1.3317154958625,0.));
#34773=CARTESIAN_POINT('Ctrl Pts',(-23.748618507953,1.3317154958625,18.));
#34774=CARTESIAN_POINT('Ctrl Pts',(-23.8230115078373,1.28006684869166,0.));
#34775=CARTESIAN_POINT('Ctrl Pts',(-23.8230115078373,1.28006684869166,18.));
#34776=CARTESIAN_POINT('Ctrl Pts',(-23.8823841929226,1.23830117308931,0.));
#34777=CARTESIAN_POINT('Ctrl Pts',(-23.8823841929226,1.23830117308931,18.));
#34778=CARTESIAN_POINT('Ctrl Pts',(-23.9268340213744,1.20672599652273,0.));
#34779=CARTESIAN_POINT('Ctrl Pts',(-23.9268340213744,1.20672599652273,18.));
#34780=CARTESIAN_POINT('Ctrl Pts',(-23.9564318364582,1.18556439589232,0.));
#34781=CARTESIAN_POINT('Ctrl Pts',(-23.9564318364582,1.18556439589232,18.));
#34782=CARTESIAN_POINT('Ctrl Pts',(-23.9712218930251,1.17495572484832,0.));
#34783=CARTESIAN_POINT('Ctrl Pts',(-23.9712218930251,1.17495572484832,18.));
#34784=CARTESIAN_POINT('Ctrl Pts',(-18.5165898451125,3.2163316265074,0.));
#34785=CARTESIAN_POINT('Ctrl Pts',(-18.5320375674878,3.21901489585931,0.));
#34786=CARTESIAN_POINT('Ctrl Pts',(-18.5629852384321,3.22384302136592,0.));
#34787=CARTESIAN_POINT('Ctrl Pts',(-18.6095634206219,3.22947000444161,0.));
#34788=CARTESIAN_POINT('Ctrl Pts',(-18.6719665316945,3.23390622002644,0.));
#34789=CARTESIAN_POINT('Ctrl Pts',(-18.7503838921122,3.23528809328097,0.));
#34790=CARTESIAN_POINT('Ctrl Pts',(-18.8291062617862,3.2337009106567,0.));
#34791=CARTESIAN_POINT('Ctrl Pts',(-18.908024664264,3.23031169402939,0.));
#34792=CARTESIAN_POINT('Ctrl Pts',(-18.987055820781,3.22595008773715,0.));
#34793=CARTESIAN_POINT('Ctrl Pts',(-19.0661599344864,3.22090173651085,0.));
#34794=CARTESIAN_POINT('Ctrl Pts',(-19.1453253990185,3.21510704576117,0.));
#34795=CARTESIAN_POINT('Ctrl Pts',(-19.2245581120423,3.2083040369031,0.));
#34796=CARTESIAN_POINT('Ctrl Pts',(-19.3038697977783,3.2001820370274,0.));
#34797=CARTESIAN_POINT('Ctrl Pts',(-19.3832648965708,3.19055618489382,0.));
#34798=CARTESIAN_POINT('Ctrl Pts',(-19.4627345689632,3.17944412249754,0.));
#34799=CARTESIAN_POINT('Ctrl Pts',(-19.5422628528517,3.16697679689295,0.));
#34800=CARTESIAN_POINT('Ctrl Pts',(-19.6218301288731,3.15334580802458,0.));
#34801=CARTESIAN_POINT('Ctrl Pts',(-19.7014173131304,3.13874131344865,0.));
#34802=CARTESIAN_POINT('Ctrl Pts',(-19.7810105986827,3.1232813132398,0.));
#34803=CARTESIAN_POINT('Ctrl Pts',(-19.8606024365399,3.10699659920993,0.));
#34804=CARTESIAN_POINT('Ctrl Pts',(-19.940188965354,3.08986795998319,0.));
#34805=CARTESIAN_POINT('Ctrl Pts',(-20.0197683853426,3.07184950717982,0.));
#34806=CARTESIAN_POINT('Ctrl Pts',(-20.0993390992966,3.05289545759951,0.));
#34807=CARTESIAN_POINT('Ctrl Pts',(-20.178897575607,3.03299094576289,0.));
#34808=CARTESIAN_POINT('Ctrl Pts',(-20.2584381977107,3.01215393913612,0.));
#34809=CARTESIAN_POINT('Ctrl Pts',(-20.3379542578194,2.99042050197905,0.));
#34810=CARTESIAN_POINT('Ctrl Pts',(-20.4174386170774,2.96783492132513,0.));
#34811=CARTESIAN_POINT('Ctrl Pts',(-20.4968844460513,2.94443868035155,0.));
#34812=CARTESIAN_POINT('Ctrl Pts',(-20.5762860772943,2.92025778619207,0.));
#34813=CARTESIAN_POINT('Ctrl Pts',(-20.6556389450993,2.89530351700806,0.));
#34814=CARTESIAN_POINT('Ctrl Pts',(-20.7349391669725,2.86957843933153,0.));
#34815=CARTESIAN_POINT('Ctrl Pts',(-20.8141832346435,2.84308082507644,0.));
#34816=CARTESIAN_POINT('Ctrl Pts',(-20.8933676828246,2.81580940715318,0.));
#34817=CARTESIAN_POINT('Ctrl Pts',(-20.9724887103073,2.78776883747222,0.));
#34818=CARTESIAN_POINT('Ctrl Pts',(-21.0515422162039,2.7589691000769,0.));
#34819=CARTESIAN_POINT('Ctrl Pts',(-21.1305239619219,2.72942309852119,0.));
#34820=CARTESIAN_POINT('Ctrl Pts',(-21.2094296949571,2.69914481283353,0.));
#34821=CARTESIAN_POINT('Ctrl Pts',(-21.2882552797978,2.66814735708301,0.));
#34822=CARTESIAN_POINT('Ctrl Pts',(-21.3669968505594,2.6364407451853,0.));
#34823=CARTESIAN_POINT('Ctrl Pts',(-21.4456507822983,2.60403221866524,0.));
#34824=CARTESIAN_POINT('Ctrl Pts',(-21.5242136128466,2.57092728351981,0.));
#34825=CARTESIAN_POINT('Ctrl Pts',(-21.6026819803014,2.53713053453767,0.));
#34826=CARTESIAN_POINT('Ctrl Pts',(-21.6810525594039,2.50264651177235,0.));
#34827=CARTESIAN_POINT('Ctrl Pts',(-21.7593219872847,2.46748070362076,0.));
#34828=CARTESIAN_POINT('Ctrl Pts',(-21.8374868743435,2.43163944362692,0.));
#34829=CARTESIAN_POINT('Ctrl Pts',(-21.9155438409279,2.39512947344577,0.));
#34830=CARTESIAN_POINT('Ctrl Pts',(-21.9934895476958,2.35795761145762,0.));
#34831=CARTESIAN_POINT('Ctrl Pts',(-22.0713207257413,2.32013040994125,0.));
#34832=CARTESIAN_POINT('Ctrl Pts',(-22.1490342171802,2.28165375160231,0.));
#34833=CARTESIAN_POINT('Ctrl Pts',(-22.2266269576315,2.24253288454712,0.));
#34834=CARTESIAN_POINT('Ctrl Pts',(-22.3040959372933,2.202772632214,0.));
#34835=CARTESIAN_POINT('Ctrl Pts',(-22.3814381677224,2.16237755726405,0.));
#34836=CARTESIAN_POINT('Ctrl Pts',(-22.4586506520939,2.1213521324248,0.));
#34837=CARTESIAN_POINT('Ctrl Pts',(-22.5357303426251,2.07970095436224,0.));
#34838=CARTESIAN_POINT('Ctrl Pts',(-22.6126741632309,2.03742874317627,0.));
#34839=CARTESIAN_POINT('Ctrl Pts',(-22.6894790673923,1.99454021984253,0.));
#34840=CARTESIAN_POINT('Ctrl Pts',(-22.7661420906702,1.95104002082891,0.));
#34841=CARTESIAN_POINT('Ctrl Pts',(-22.8426603964871,1.90693261239855,0.));
#34842=CARTESIAN_POINT('Ctrl Pts',(-22.9190313507225,1.86222218327819,0.));
#34843=CARTESIAN_POINT('Ctrl Pts',(-22.9952524859917,1.81691265597282,0.));
#34844=CARTESIAN_POINT('Ctrl Pts',(-23.0713213684573,1.77100780743078,0.));
#34845=CARTESIAN_POINT('Ctrl Pts',(-23.1472354850579,1.72451136919382,0.));
#34846=CARTESIAN_POINT('Ctrl Pts',(-23.2229921402299,1.67742712670823,0.));
#34847=CARTESIAN_POINT('Ctrl Pts',(-23.2985883089733,1.62975905604583,0.));
#34848=CARTESIAN_POINT('Ctrl Pts',(-23.3740206492924,1.58151133638848,0.));
#34849=CARTESIAN_POINT('Ctrl Pts',(-23.4492857841673,1.53268814658653,0.));
#34850=CARTESIAN_POINT('Ctrl Pts',(-23.5243805284282,1.48329351290851,0.));
#34851=CARTESIAN_POINT('Ctrl Pts',(-23.5993021272808,1.4333311444639,0.));
#34852=CARTESIAN_POINT('Ctrl Pts',(-23.6740485197917,1.38280426780156,0.));
#34853=CARTESIAN_POINT('Ctrl Pts',(-23.7635325055853,1.32149774147469,0.));
#34854=CARTESIAN_POINT('Ctrl Pts',(-23.8378812584003,1.2697091254959,0.));
#34855=CARTESIAN_POINT('Ctrl Pts',(-23.89721850443,1.22783185562045,0.));
#34856=CARTESIAN_POINT('Ctrl Pts',(-23.9416417798466,1.19617306697387,0.));
#34857=CARTESIAN_POINT('Ctrl Pts',(-23.9712218930251,1.17495572484832,0.));
#34858=CARTESIAN_POINT('Ctrl Pts',(-18.5165898451125,3.2163316265074,15.));
#34859=CARTESIAN_POINT('Ctrl Pts',(-18.5320375674878,3.21901489585931,15.));
#34860=CARTESIAN_POINT('Ctrl Pts',(-18.5629852384321,3.22384302136592,15.));
#34861=CARTESIAN_POINT('Ctrl Pts',(-18.6095634206219,3.22947000444161,15.));
#34862=CARTESIAN_POINT('Ctrl Pts',(-18.6719665316945,3.23390622002644,15.));
#34863=CARTESIAN_POINT('Ctrl Pts',(-18.7503838921122,3.23528809328097,15.));
#34864=CARTESIAN_POINT('Ctrl Pts',(-18.8291062617862,3.2337009106567,15.));
#34865=CARTESIAN_POINT('Ctrl Pts',(-18.908024664264,3.23031169402939,15.));
#34866=CARTESIAN_POINT('Ctrl Pts',(-18.987055820781,3.22595008773715,15.));
#34867=CARTESIAN_POINT('Ctrl Pts',(-19.0661599344864,3.22090173651085,15.));
#34868=CARTESIAN_POINT('Ctrl Pts',(-19.1453253990185,3.21510704576117,15.));
#34869=CARTESIAN_POINT('Ctrl Pts',(-19.2245581120423,3.2083040369031,15.));
#34870=CARTESIAN_POINT('Ctrl Pts',(-19.3038697977783,3.2001820370274,15.));
#34871=CARTESIAN_POINT('Ctrl Pts',(-19.3832648965708,3.19055618489382,15.));
#34872=CARTESIAN_POINT('Ctrl Pts',(-19.4627345689632,3.17944412249754,15.));
#34873=CARTESIAN_POINT('Ctrl Pts',(-19.5422628528517,3.16697679689295,15.));
#34874=CARTESIAN_POINT('Ctrl Pts',(-19.6218301288731,3.15334580802458,15.));
#34875=CARTESIAN_POINT('Ctrl Pts',(-19.7014173131304,3.13874131344865,15.));
#34876=CARTESIAN_POINT('Ctrl Pts',(-19.7810105986827,3.1232813132398,15.));
#34877=CARTESIAN_POINT('Ctrl Pts',(-19.8606024365399,3.10699659920993,15.));
#34878=CARTESIAN_POINT('Ctrl Pts',(-19.940188965354,3.08986795998319,15.));
#34879=CARTESIAN_POINT('Ctrl Pts',(-20.0197683853426,3.07184950717982,15.));
#34880=CARTESIAN_POINT('Ctrl Pts',(-20.0993390992966,3.05289545759951,15.));
#34881=CARTESIAN_POINT('Ctrl Pts',(-20.178897575607,3.03299094576289,15.));
#34882=CARTESIAN_POINT('Ctrl Pts',(-20.2584381977107,3.01215393913612,15.));
#34883=CARTESIAN_POINT('Ctrl Pts',(-20.3379542578194,2.99042050197905,15.));
#34884=CARTESIAN_POINT('Ctrl Pts',(-20.4174386170774,2.96783492132513,15.));
#34885=CARTESIAN_POINT('Ctrl Pts',(-20.4968844460513,2.94443868035155,15.));
#34886=CARTESIAN_POINT('Ctrl Pts',(-20.5762860772943,2.92025778619207,15.));
#34887=CARTESIAN_POINT('Ctrl Pts',(-20.6556389450993,2.89530351700806,15.));
#34888=CARTESIAN_POINT('Ctrl Pts',(-20.7349391669725,2.86957843933153,15.));
#34889=CARTESIAN_POINT('Ctrl Pts',(-20.8141832346435,2.84308082507644,15.));
#34890=CARTESIAN_POINT('Ctrl Pts',(-20.8933676828246,2.81580940715318,15.));
#34891=CARTESIAN_POINT('Ctrl Pts',(-20.9724887103073,2.78776883747222,15.));
#34892=CARTESIAN_POINT('Ctrl Pts',(-21.0515422162039,2.7589691000769,15.));
#34893=CARTESIAN_POINT('Ctrl Pts',(-21.1305239619219,2.72942309852119,15.));
#34894=CARTESIAN_POINT('Ctrl Pts',(-21.2094296949571,2.69914481283353,15.));
#34895=CARTESIAN_POINT('Ctrl Pts',(-21.2882552797978,2.66814735708301,15.));
#34896=CARTESIAN_POINT('Ctrl Pts',(-21.3669968505594,2.6364407451853,15.));
#34897=CARTESIAN_POINT('Ctrl Pts',(-21.4456507822983,2.60403221866524,15.));
#34898=CARTESIAN_POINT('Ctrl Pts',(-21.5242136128466,2.57092728351981,15.));
#34899=CARTESIAN_POINT('Ctrl Pts',(-21.6026819803014,2.53713053453767,15.));
#34900=CARTESIAN_POINT('Ctrl Pts',(-21.6810525594039,2.50264651177235,15.));
#34901=CARTESIAN_POINT('Ctrl Pts',(-21.7593219872847,2.46748070362076,15.));
#34902=CARTESIAN_POINT('Ctrl Pts',(-21.8374868743435,2.43163944362692,15.));
#34903=CARTESIAN_POINT('Ctrl Pts',(-21.9155438409279,2.39512947344577,15.));
#34904=CARTESIAN_POINT('Ctrl Pts',(-21.9934895476958,2.35795761145762,15.));
#34905=CARTESIAN_POINT('Ctrl Pts',(-22.0713207257413,2.32013040994125,15.));
#34906=CARTESIAN_POINT('Ctrl Pts',(-22.1490342171802,2.28165375160231,15.));
#34907=CARTESIAN_POINT('Ctrl Pts',(-22.2266269576315,2.24253288454712,15.));
#34908=CARTESIAN_POINT('Ctrl Pts',(-22.3040959372933,2.202772632214,15.));
#34909=CARTESIAN_POINT('Ctrl Pts',(-22.3814381677224,2.16237755726405,15.));
#34910=CARTESIAN_POINT('Ctrl Pts',(-22.4586506520939,2.1213521324248,15.));
#34911=CARTESIAN_POINT('Ctrl Pts',(-22.5357303426251,2.07970095436224,15.));
#34912=CARTESIAN_POINT('Ctrl Pts',(-22.6126741632309,2.03742874317627,15.));
#34913=CARTESIAN_POINT('Ctrl Pts',(-22.6894790673923,1.99454021984253,15.));
#34914=CARTESIAN_POINT('Ctrl Pts',(-22.7661420906702,1.95104002082891,15.));
#34915=CARTESIAN_POINT('Ctrl Pts',(-22.8426603964871,1.90693261239855,15.));
#34916=CARTESIAN_POINT('Ctrl Pts',(-22.9190313507225,1.86222218327819,15.));
#34917=CARTESIAN_POINT('Ctrl Pts',(-22.9952524859917,1.81691265597282,15.));
#34918=CARTESIAN_POINT('Ctrl Pts',(-23.0713213684573,1.77100780743078,15.));
#34919=CARTESIAN_POINT('Ctrl Pts',(-23.1472354850579,1.72451136919382,15.));
#34920=CARTESIAN_POINT('Ctrl Pts',(-23.2229921402299,1.67742712670823,15.));
#34921=CARTESIAN_POINT('Ctrl Pts',(-23.2985883089733,1.62975905604583,15.));
#34922=CARTESIAN_POINT('Ctrl Pts',(-23.3740206492924,1.58151133638848,15.));
#34923=CARTESIAN_POINT('Ctrl Pts',(-23.4492857841673,1.53268814658653,15.));
#34924=CARTESIAN_POINT('Ctrl Pts',(-23.5243805284282,1.48329351290851,15.));
#34925=CARTESIAN_POINT('Ctrl Pts',(-23.5993021272808,1.4333311444639,15.));
#34926=CARTESIAN_POINT('Ctrl Pts',(-23.6740485197917,1.38280426780156,15.));
#34927=CARTESIAN_POINT('Ctrl Pts',(-23.7635325055853,1.32149774147469,15.));
#34928=CARTESIAN_POINT('Ctrl Pts',(-23.8378812584003,1.2697091254959,15.));
#34929=CARTESIAN_POINT('Ctrl Pts',(-23.89721850443,1.22783185562045,15.));
#34930=CARTESIAN_POINT('Ctrl Pts',(-23.9416417798466,1.19617306697387,15.));
#34931=CARTESIAN_POINT('Ctrl Pts',(-23.9712218930251,1.17495572484832,15.));
#34932=CARTESIAN_POINT('Ctrl Pts',(-20.0837475345526,13.1393715591102,0.));
#34933=CARTESIAN_POINT('Ctrl Pts',(-20.0837475345526,13.1393715591102,18.));
#34934=CARTESIAN_POINT('Ctrl Pts',(-20.0780177478283,13.1220955868173,0.));
#34935=CARTESIAN_POINT('Ctrl Pts',(-20.0780177478283,13.1220955868173,18.));
#34936=CARTESIAN_POINT('Ctrl Pts',(-20.0665110891946,13.0875783330728,0.));
#34937=CARTESIAN_POINT('Ctrl Pts',(-20.0665110891946,13.0875783330728,18.));
#34938=CARTESIAN_POINT('Ctrl Pts',(-20.0491098457044,13.0359065249991,0.));
#34939=CARTESIAN_POINT('Ctrl Pts',(-20.0491098457044,13.0359065249991,18.));
#34940=CARTESIAN_POINT('Ctrl Pts',(-20.0256255826397,12.9672189949731,0.));
#34941=CARTESIAN_POINT('Ctrl Pts',(-20.0256255826397,12.9672189949731,18.));
#34942=CARTESIAN_POINT('Ctrl Pts',(-19.9957986945787,12.8817072534696,0.));
#34943=CARTESIAN_POINT('Ctrl Pts',(-19.9957986945787,12.8817072534696,18.));
#34944=CARTESIAN_POINT('Ctrl Pts',(-19.9654995335894,12.7965444294443,0.));
#34945=CARTESIAN_POINT('Ctrl Pts',(-19.9654995335894,12.7965444294443,18.));
#34946=CARTESIAN_POINT('Ctrl Pts',(-19.9347273847264,12.7117325003719,0.));
#34947=CARTESIAN_POINT('Ctrl Pts',(-19.9347273847264,12.7117325003719,18.));
#34948=CARTESIAN_POINT('Ctrl Pts',(-19.9034816813503,12.6272742843372,0.));
#34949=CARTESIAN_POINT('Ctrl Pts',(-19.9034816813503,12.6272742843372,18.));
#34950=CARTESIAN_POINT('Ctrl Pts',(-19.8717621942733,12.5431736030596,0.));
#34951=CARTESIAN_POINT('Ctrl Pts',(-19.8717621942733,12.5431736030596,18.));
#34952=CARTESIAN_POINT('Ctrl Pts',(-19.839568972011,12.4594350764989,0.));
#34953=CARTESIAN_POINT('Ctrl Pts',(-19.839568972011,12.4594350764989,18.));
#34954=CARTESIAN_POINT('Ctrl Pts',(-19.8069022248387,12.3760638341708,0.));
#34955=CARTESIAN_POINT('Ctrl Pts',(-19.8069022248387,12.3760638341708,18.));
#34956=CARTESIAN_POINT('Ctrl Pts',(-19.7737622285562,12.2930652417987,0.));
#34957=CARTESIAN_POINT('Ctrl Pts',(-19.7737622285562,12.2930652417987,18.));
#34958=CARTESIAN_POINT('Ctrl Pts',(-19.7401492304335,12.2104446447874,0.));
#34959=CARTESIAN_POINT('Ctrl Pts',(-19.7401492304335,12.2104446447874,18.));
#34960=CARTESIAN_POINT('Ctrl Pts',(-19.7060633406705,12.1282070378972,0.));
#34961=CARTESIAN_POINT('Ctrl Pts',(-19.7060633406705,12.1282070378972,18.));
#34962=CARTESIAN_POINT('Ctrl Pts',(-19.6715045149944,12.0463570680309,0.));
#34963=CARTESIAN_POINT('Ctrl Pts',(-19.6715045149944,12.0463570680309,18.));
#34964=CARTESIAN_POINT('Ctrl Pts',(-19.6364725931695,11.9648992312094,0.));
#34965=CARTESIAN_POINT('Ctrl Pts',(-19.6364725931695,11.9648992312094,18.));
#34966=CARTESIAN_POINT('Ctrl Pts',(-19.6009673241771,11.8838380136222,0.));
#34967=CARTESIAN_POINT('Ctrl Pts',(-19.6009673241771,11.8838380136222,18.));
#34968=CARTESIAN_POINT('Ctrl Pts',(-19.5649883985826,11.8031780389346,0.));
#34969=CARTESIAN_POINT('Ctrl Pts',(-19.5649883985826,11.8031780389346,18.));
#34970=CARTESIAN_POINT('Ctrl Pts',(-19.5285354853626,11.722924244195,0.));
#34971=CARTESIAN_POINT('Ctrl Pts',(-19.5285354853626,11.722924244195,18.));
#34972=CARTESIAN_POINT('Ctrl Pts',(-19.4916082541529,11.6430819099846,0.));
#34973=CARTESIAN_POINT('Ctrl Pts',(-19.4916082541529,11.6430819099846,18.));
#34974=CARTESIAN_POINT('Ctrl Pts',(-19.4542063779876,11.5636565297382,0.));
#34975=CARTESIAN_POINT('Ctrl Pts',(-19.4542063779876,11.5636565297382,18.));
#34976=CARTESIAN_POINT('Ctrl Pts',(-19.4163295466324,11.4846537135043,0.));
#34977=CARTESIAN_POINT('Ctrl Pts',(-19.4163295466324,11.4846537135043,18.));
#34978=CARTESIAN_POINT('Ctrl Pts',(-19.3779774742875,11.4060790880015,0.));
#34979=CARTESIAN_POINT('Ctrl Pts',(-19.3779774742875,11.4060790880015,18.));
#34980=CARTESIAN_POINT('Ctrl Pts',(-19.3391499248083,11.3279381634523,0.));
#34981=CARTESIAN_POINT('Ctrl Pts',(-19.3391499248083,11.3279381634523,18.));
#34982=CARTESIAN_POINT('Ctrl Pts',(-19.2998466936739,11.2502363198588,0.));
#34983=CARTESIAN_POINT('Ctrl Pts',(-19.2998466936739,11.2502363198588,18.));
#34984=CARTESIAN_POINT('Ctrl Pts',(-19.2600675167206,11.1729790050543,0.));
#34985=CARTESIAN_POINT('Ctrl Pts',(-19.2600675167206,11.1729790050543,18.));
#34986=CARTESIAN_POINT('Ctrl Pts',(-19.2198119937835,11.0961718903994,0.));
#34987=CARTESIAN_POINT('Ctrl Pts',(-19.2198119937835,11.0961718903994,18.));
#34988=CARTESIAN_POINT('Ctrl Pts',(-19.1790795192393,11.0198210228993,0.));
#34989=CARTESIAN_POINT('Ctrl Pts',(-19.1790795192393,11.0198210228993,18.));
#34990=CARTESIAN_POINT('Ctrl Pts',(-19.1378691901023,10.9439330179206,0.));
#34991=CARTESIAN_POINT('Ctrl Pts',(-19.1378691901023,10.9439330179206,18.));
#34992=CARTESIAN_POINT('Ctrl Pts',(-19.0961797996403,10.868515097783,0.));
#34993=CARTESIAN_POINT('Ctrl Pts',(-19.0961797996403,10.868515097783,18.));
#34994=CARTESIAN_POINT('Ctrl Pts',(-19.0540100416943,10.7935747414879,0.));
#34995=CARTESIAN_POINT('Ctrl Pts',(-19.0540100416943,10.7935747414879,18.));
#34996=CARTESIAN_POINT('Ctrl Pts',(-19.0113586878152,10.7191193896586,0.));
#34997=CARTESIAN_POINT('Ctrl Pts',(-19.0113586878152,10.7191193896586,18.));
#34998=CARTESIAN_POINT('Ctrl Pts',(-18.9682247574834,10.6451561585969,0.));
#34999=CARTESIAN_POINT('Ctrl Pts',(-18.9682247574834,10.6451561585969,18.));
#35000=CARTESIAN_POINT('Ctrl Pts',(-18.9246077453188,10.5716914651544,0.));
#35001=CARTESIAN_POINT('Ctrl Pts',(-18.9246077453188,10.5716914651544,18.));
#35002=CARTESIAN_POINT('Ctrl Pts',(-18.8805076729356,10.4987309368494,0.));
#35003=CARTESIAN_POINT('Ctrl Pts',(-18.8805076729356,10.4987309368494,18.));
#35004=CARTESIAN_POINT('Ctrl Pts',(-18.8359245594214,10.4262802670211,0.));
#35005=CARTESIAN_POINT('Ctrl Pts',(-18.8359245594214,10.4262802670211,18.));
#35006=CARTESIAN_POINT('Ctrl Pts',(-18.7908579693851,10.3543459451258,0.));
#35007=CARTESIAN_POINT('Ctrl Pts',(-18.7908579693851,10.3543459451258,18.));
#35008=CARTESIAN_POINT('Ctrl Pts',(-18.7453065790062,10.2829359603685,0.));
#35009=CARTESIAN_POINT('Ctrl Pts',(-18.7453065790062,10.2829359603685,18.));
#35010=CARTESIAN_POINT('Ctrl Pts',(-18.699267629819,10.2120606864872,0.));
#35011=CARTESIAN_POINT('Ctrl Pts',(-18.699267629819,10.2120606864872,18.));
#35012=CARTESIAN_POINT('Ctrl Pts',(-18.6527367592664,10.1417331637795,0.));
#35013=CARTESIAN_POINT('Ctrl Pts',(-18.6527367592664,10.1417331637795,18.));
#35014=CARTESIAN_POINT('Ctrl Pts',(-18.605709190442,10.0719672018851,0.));
#35015=CARTESIAN_POINT('Ctrl Pts',(-18.605709190442,10.0719672018851,18.));
#35016=CARTESIAN_POINT('Ctrl Pts',(-18.5581807679204,10.0027757313807,0.));
#35017=CARTESIAN_POINT('Ctrl Pts',(-18.5581807679204,10.0027757313807,18.));
#35018=CARTESIAN_POINT('Ctrl Pts',(-18.5101489409161,9.93416923996829,0.));
#35019=CARTESIAN_POINT('Ctrl Pts',(-18.5101489409161,9.93416923996829,18.));
#35020=CARTESIAN_POINT('Ctrl Pts',(-18.461614050347,9.86615372541685,0.));
#35021=CARTESIAN_POINT('Ctrl Pts',(-18.461614050347,9.86615372541685,18.));
#35022=CARTESIAN_POINT('Ctrl Pts',(-18.4125796444662,9.79873019947434,0.));
#35023=CARTESIAN_POINT('Ctrl Pts',(-18.4125796444662,9.79873019947434,18.));
#35024=CARTESIAN_POINT('Ctrl Pts',(-18.3630495772677,9.73189932619939,0.));
#35025=CARTESIAN_POINT('Ctrl Pts',(-18.3630495772677,9.73189932619939,18.));
#35026=CARTESIAN_POINT('Ctrl Pts',(-18.3130254811852,9.6656654640326,0.));
#35027=CARTESIAN_POINT('Ctrl Pts',(-18.3130254811852,9.6656654640326,18.));
#35028=CARTESIAN_POINT('Ctrl Pts',(-18.2625044208165,9.60004042085347,0.));
#35029=CARTESIAN_POINT('Ctrl Pts',(-18.2625044208165,9.60004042085347,18.));
#35030=CARTESIAN_POINT('Ctrl Pts',(-18.2114756946126,9.53504856811685,0.));
#35031=CARTESIAN_POINT('Ctrl Pts',(-18.2114756946126,9.53504856811685,18.));
#35032=CARTESIAN_POINT('Ctrl Pts',(-18.1599204445014,9.47072748065832,0.));
#35033=CARTESIAN_POINT('Ctrl Pts',(-18.1599204445014,9.47072748065832,18.));
#35034=CARTESIAN_POINT('Ctrl Pts',(-18.1078184146735,9.40711718355464,0.));
#35035=CARTESIAN_POINT('Ctrl Pts',(-18.1078184146735,9.40711718355464,18.));
#35036=CARTESIAN_POINT('Ctrl Pts',(-18.0551538338035,9.34425079614396,0.));
#35037=CARTESIAN_POINT('Ctrl Pts',(-18.0551538338035,9.34425079614396,18.));
#35038=CARTESIAN_POINT('Ctrl Pts',(-18.0019206847747,9.28214615574471,0.));
#35039=CARTESIAN_POINT('Ctrl Pts',(-18.0019206847747,9.28214615574471,18.));
#35040=CARTESIAN_POINT('Ctrl Pts',(-17.9481305624284,9.22079331175917,0.));
#35041=CARTESIAN_POINT('Ctrl Pts',(-17.9481305624284,9.22079331175917,18.));
#35042=CARTESIAN_POINT('Ctrl Pts',(-17.8938116696237,9.1601561636161,0.));
#35043=CARTESIAN_POINT('Ctrl Pts',(-17.8938116696237,9.1601561636161,18.));
#35044=CARTESIAN_POINT('Ctrl Pts',(-17.8389924349283,9.10019864472208,0.));
#35045=CARTESIAN_POINT('Ctrl Pts',(-17.8389924349283,9.10019864472208,18.));
#35046=CARTESIAN_POINT('Ctrl Pts',(-17.7836872744016,9.04090748239097,0.));
#35047=CARTESIAN_POINT('Ctrl Pts',(-17.7836872744016,9.04090748239097,18.));
#35048=CARTESIAN_POINT('Ctrl Pts',(-17.7278841963319,8.98231202490686,0.));
#35049=CARTESIAN_POINT('Ctrl Pts',(-17.7278841963319,8.98231202490686,18.));
#35050=CARTESIAN_POINT('Ctrl Pts',(-17.6715250120654,8.92451585185175,0.));
#35051=CARTESIAN_POINT('Ctrl Pts',(-17.6715250120654,8.92451585185175,18.));
#35052=CARTESIAN_POINT('Ctrl Pts',(-17.614513388992,8.86768402115344,0.));
#35053=CARTESIAN_POINT('Ctrl Pts',(-17.614513388992,8.86768402115344,18.));
#35054=CARTESIAN_POINT('Ctrl Pts',(-17.5567525798882,8.81198307239551,0.));
#35055=CARTESIAN_POINT('Ctrl Pts',(-17.5567525798882,8.81198307239551,18.));
#35056=CARTESIAN_POINT('Ctrl Pts',(-17.4981785296199,8.75752832625954,0.));
#35057=CARTESIAN_POINT('Ctrl Pts',(-17.4981785296199,8.75752832625954,18.));
#35058=CARTESIAN_POINT('Ctrl Pts',(-17.438788019753,8.70433925112174,0.));
#35059=CARTESIAN_POINT('Ctrl Pts',(-17.438788019753,8.70433925112174,18.));
#35060=CARTESIAN_POINT('Ctrl Pts',(-17.3786861166843,8.65226368112816,0.));
#35061=CARTESIAN_POINT('Ctrl Pts',(-17.3786861166843,8.65226368112816,18.));
#35062=CARTESIAN_POINT('Ctrl Pts',(-17.3180459442745,8.60104338529165,0.));
#35063=CARTESIAN_POINT('Ctrl Pts',(-17.3180459442745,8.60104338529165,18.));
#35064=CARTESIAN_POINT('Ctrl Pts',(-17.2570167183611,8.55046295192433,0.));
#35065=CARTESIAN_POINT('Ctrl Pts',(-17.2570167183611,8.55046295192433,18.));
#35066=CARTESIAN_POINT('Ctrl Pts',(-17.1956428575086,8.50048099003883,0.));
#35067=CARTESIAN_POINT('Ctrl Pts',(-17.1956428575086,8.50048099003883,18.));
#35068=CARTESIAN_POINT('Ctrl Pts',(-17.1337886602855,8.45135198307877,0.));
#35069=CARTESIAN_POINT('Ctrl Pts',(-17.1337886602855,8.45135198307877,18.));
#35070=CARTESIAN_POINT('Ctrl Pts',(-17.071033847921,8.40379607744266,0.));
#35071=CARTESIAN_POINT('Ctrl Pts',(-17.071033847921,8.40379607744266,18.));
#35072=CARTESIAN_POINT('Ctrl Pts',(-17.0067806259695,8.35882146841244,0.));
#35073=CARTESIAN_POINT('Ctrl Pts',(-17.0067806259695,8.35882146841244,18.));
#35074=CARTESIAN_POINT('Ctrl Pts',(-16.9536879065132,8.32573081382563,0.));
#35075=CARTESIAN_POINT('Ctrl Pts',(-16.9536879065132,8.32573081382563,18.));
#35076=CARTESIAN_POINT('Ctrl Pts',(-16.9126979078877,8.30290517019115,0.));
#35077=CARTESIAN_POINT('Ctrl Pts',(-16.9126979078877,8.30290517019115,18.));
#35078=CARTESIAN_POINT('Ctrl Pts',(-16.8848228151885,8.28862062120315,0.));
#35079=CARTESIAN_POINT('Ctrl Pts',(-16.8848228151885,8.28862062120315,18.));
#35080=CARTESIAN_POINT('Ctrl Pts',(-16.8707481591095,8.28171148831561,0.));
#35081=CARTESIAN_POINT('Ctrl Pts',(-16.8707481591095,8.28171148831561,18.));
#35082=CARTESIAN_POINT('',(-20.0837475345525,13.1393715591102,0.));
#35083=CARTESIAN_POINT('Ctrl Pts',(-16.8707481591095,8.28171148831561,0.));
#35084=CARTESIAN_POINT('Ctrl Pts',(-16.8848228151885,8.28862062120315,0.));
#35085=CARTESIAN_POINT('Ctrl Pts',(-16.9126979078877,8.30290517019115,0.));
#35086=CARTESIAN_POINT('Ctrl Pts',(-16.9536879065132,8.32573081382563,0.));
#35087=CARTESIAN_POINT('Ctrl Pts',(-17.0067806259695,8.35882146841244,0.));
#35088=CARTESIAN_POINT('Ctrl Pts',(-17.071033847921,8.40379607744266,0.));
#35089=CARTESIAN_POINT('Ctrl Pts',(-17.1337886602855,8.45135198307877,0.));
#35090=CARTESIAN_POINT('Ctrl Pts',(-17.1956428575086,8.50048099003883,0.));
#35091=CARTESIAN_POINT('Ctrl Pts',(-17.2570167183611,8.55046295192433,0.));
#35092=CARTESIAN_POINT('Ctrl Pts',(-17.3180459442745,8.60104338529165,0.));
#35093=CARTESIAN_POINT('Ctrl Pts',(-17.3786861166843,8.65226368112816,0.));
#35094=CARTESIAN_POINT('Ctrl Pts',(-17.438788019753,8.70433925112174,0.));
#35095=CARTESIAN_POINT('Ctrl Pts',(-17.4981785296199,8.75752832625954,0.));
#35096=CARTESIAN_POINT('Ctrl Pts',(-17.5567525798882,8.81198307239551,0.));
#35097=CARTESIAN_POINT('Ctrl Pts',(-17.614513388992,8.86768402115344,0.));
#35098=CARTESIAN_POINT('Ctrl Pts',(-17.6715250120654,8.92451585185175,0.));
#35099=CARTESIAN_POINT('Ctrl Pts',(-17.7278841963319,8.98231202490686,0.));
#35100=CARTESIAN_POINT('Ctrl Pts',(-17.7836872744016,9.04090748239097,0.));
#35101=CARTESIAN_POINT('Ctrl Pts',(-17.8389924349283,9.10019864472208,0.));
#35102=CARTESIAN_POINT('Ctrl Pts',(-17.8938116696237,9.1601561636161,0.));
#35103=CARTESIAN_POINT('Ctrl Pts',(-17.9481305624284,9.22079331175917,0.));
#35104=CARTESIAN_POINT('Ctrl Pts',(-18.0019206847747,9.28214615574471,0.));
#35105=CARTESIAN_POINT('Ctrl Pts',(-18.0551538338035,9.34425079614396,0.));
#35106=CARTESIAN_POINT('Ctrl Pts',(-18.1078184146735,9.40711718355464,0.));
#35107=CARTESIAN_POINT('Ctrl Pts',(-18.1599204445014,9.47072748065832,0.));
#35108=CARTESIAN_POINT('Ctrl Pts',(-18.2114756946126,9.53504856811685,0.));
#35109=CARTESIAN_POINT('Ctrl Pts',(-18.2625044208165,9.60004042085347,0.));
#35110=CARTESIAN_POINT('Ctrl Pts',(-18.3130254811852,9.6656654640326,0.));
#35111=CARTESIAN_POINT('Ctrl Pts',(-18.3630495772677,9.73189932619939,0.));
#35112=CARTESIAN_POINT('Ctrl Pts',(-18.4125796444662,9.79873019947434,0.));
#35113=CARTESIAN_POINT('Ctrl Pts',(-18.461614050347,9.86615372541685,0.));
#35114=CARTESIAN_POINT('Ctrl Pts',(-18.5101489409161,9.93416923996829,0.));
#35115=CARTESIAN_POINT('Ctrl Pts',(-18.5581807679204,10.0027757313807,0.));
#35116=CARTESIAN_POINT('Ctrl Pts',(-18.605709190442,10.0719672018851,0.));
#35117=CARTESIAN_POINT('Ctrl Pts',(-18.6527367592664,10.1417331637795,0.));
#35118=CARTESIAN_POINT('Ctrl Pts',(-18.699267629819,10.2120606864872,0.));
#35119=CARTESIAN_POINT('Ctrl Pts',(-18.7453065790062,10.2829359603685,0.));
#35120=CARTESIAN_POINT('Ctrl Pts',(-18.7908579693851,10.3543459451258,0.));
#35121=CARTESIAN_POINT('Ctrl Pts',(-18.8359245594214,10.4262802670211,0.));
#35122=CARTESIAN_POINT('Ctrl Pts',(-18.8805076729356,10.4987309368494,0.));
#35123=CARTESIAN_POINT('Ctrl Pts',(-18.9246077453188,10.5716914651544,0.));
#35124=CARTESIAN_POINT('Ctrl Pts',(-18.9682247574834,10.6451561585969,0.));
#35125=CARTESIAN_POINT('Ctrl Pts',(-19.0113586878152,10.7191193896586,0.));
#35126=CARTESIAN_POINT('Ctrl Pts',(-19.0540100416943,10.7935747414879,0.));
#35127=CARTESIAN_POINT('Ctrl Pts',(-19.0961797996403,10.868515097783,0.));
#35128=CARTESIAN_POINT('Ctrl Pts',(-19.1378691901023,10.9439330179206,0.));
#35129=CARTESIAN_POINT('Ctrl Pts',(-19.1790795192393,11.0198210228993,0.));
#35130=CARTESIAN_POINT('Ctrl Pts',(-19.2198119937835,11.0961718903994,0.));
#35131=CARTESIAN_POINT('Ctrl Pts',(-19.2600675167206,11.1729790050543,0.));
#35132=CARTESIAN_POINT('Ctrl Pts',(-19.2998466936739,11.2502363198588,0.));
#35133=CARTESIAN_POINT('Ctrl Pts',(-19.3391499248083,11.3279381634523,0.));
#35134=CARTESIAN_POINT('Ctrl Pts',(-19.3779774742875,11.4060790880015,0.));
#35135=CARTESIAN_POINT('Ctrl Pts',(-19.4163295466324,11.4846537135043,0.));
#35136=CARTESIAN_POINT('Ctrl Pts',(-19.4542063779876,11.5636565297382,0.));
#35137=CARTESIAN_POINT('Ctrl Pts',(-19.4916082541529,11.6430819099846,0.));
#35138=CARTESIAN_POINT('Ctrl Pts',(-19.5285354853626,11.722924244195,0.));
#35139=CARTESIAN_POINT('Ctrl Pts',(-19.5649883985826,11.8031780389346,0.));
#35140=CARTESIAN_POINT('Ctrl Pts',(-19.6009673241771,11.8838380136222,0.));
#35141=CARTESIAN_POINT('Ctrl Pts',(-19.6364725931695,11.9648992312094,0.));
#35142=CARTESIAN_POINT('Ctrl Pts',(-19.6715045149944,12.0463570680309,0.));
#35143=CARTESIAN_POINT('Ctrl Pts',(-19.7060633406705,12.1282070378972,0.));
#35144=CARTESIAN_POINT('Ctrl Pts',(-19.7401492304335,12.2104446447874,0.));
#35145=CARTESIAN_POINT('Ctrl Pts',(-19.7737622285562,12.2930652417987,0.));
#35146=CARTESIAN_POINT('Ctrl Pts',(-19.8069022248387,12.3760638341708,0.));
#35147=CARTESIAN_POINT('Ctrl Pts',(-19.839568972011,12.4594350764989,0.));
#35148=CARTESIAN_POINT('Ctrl Pts',(-19.8717621942733,12.5431736030596,0.));
#35149=CARTESIAN_POINT('Ctrl Pts',(-19.9034816813503,12.6272742843372,0.));
#35150=CARTESIAN_POINT('Ctrl Pts',(-19.9347273847264,12.7117325003719,0.));
#35151=CARTESIAN_POINT('Ctrl Pts',(-19.9654995335894,12.7965444294443,0.));
#35152=CARTESIAN_POINT('Ctrl Pts',(-20.0018585267766,12.8987398182747,0.));
#35153=CARTESIAN_POINT('Ctrl Pts',(-20.0315673466055,12.9843387891477,0.));
#35154=CARTESIAN_POINT('Ctrl Pts',(-20.054957345404,13.0530957702829,0.));
#35155=CARTESIAN_POINT('Ctrl Pts',(-20.0722879610899,13.1048196144678,0.));
#35156=CARTESIAN_POINT('Ctrl Pts',(-20.0837475345526,13.1393715591102,0.));
#35157=CARTESIAN_POINT('',(-20.0837475345525,13.1393715591102,15.));
#35158=CARTESIAN_POINT('Ctrl Pts',(-20.0837475345526,13.1393715591102,15.));
#35159=CARTESIAN_POINT('Ctrl Pts',(-20.0780177478283,13.1220955868173,15.));
#35160=CARTESIAN_POINT('Ctrl Pts',(-20.0665110891946,13.0875783330728,15.));
#35161=CARTESIAN_POINT('Ctrl Pts',(-20.0491098457044,13.0359065249991,15.));
#35162=CARTESIAN_POINT('Ctrl Pts',(-20.0256255826397,12.9672189949731,15.));
#35163=CARTESIAN_POINT('Ctrl Pts',(-19.9957986945787,12.8817072534696,15.));
#35164=CARTESIAN_POINT('Ctrl Pts',(-19.9654995335894,12.7965444294443,15.));
#35165=CARTESIAN_POINT('Ctrl Pts',(-19.9347273847264,12.7117325003719,15.));
#35166=CARTESIAN_POINT('Ctrl Pts',(-19.9034816813503,12.6272742843372,15.));
#35167=CARTESIAN_POINT('Ctrl Pts',(-19.8717621942733,12.5431736030596,15.));
#35168=CARTESIAN_POINT('Ctrl Pts',(-19.839568972011,12.4594350764989,15.));
#35169=CARTESIAN_POINT('Ctrl Pts',(-19.8069022248387,12.3760638341708,15.));
#35170=CARTESIAN_POINT('Ctrl Pts',(-19.7737622285562,12.2930652417987,15.));
#35171=CARTESIAN_POINT('Ctrl Pts',(-19.7401492304335,12.2104446447874,15.));
#35172=CARTESIAN_POINT('Ctrl Pts',(-19.7060633406705,12.1282070378972,15.));
#35173=CARTESIAN_POINT('Ctrl Pts',(-19.6715045149944,12.0463570680309,15.));
#35174=CARTESIAN_POINT('Ctrl Pts',(-19.6364725931695,11.9648992312094,15.));
#35175=CARTESIAN_POINT('Ctrl Pts',(-19.6009673241771,11.8838380136222,15.));
#35176=CARTESIAN_POINT('Ctrl Pts',(-19.5649883985826,11.8031780389346,15.));
#35177=CARTESIAN_POINT('Ctrl Pts',(-19.5285354853626,11.722924244195,15.));
#35178=CARTESIAN_POINT('Ctrl Pts',(-19.4916082541529,11.6430819099846,15.));
#35179=CARTESIAN_POINT('Ctrl Pts',(-19.4542063779876,11.5636565297382,15.));
#35180=CARTESIAN_POINT('Ctrl Pts',(-19.4163295466324,11.4846537135043,15.));
#35181=CARTESIAN_POINT('Ctrl Pts',(-19.3779774742875,11.4060790880015,15.));
#35182=CARTESIAN_POINT('Ctrl Pts',(-19.3391499248083,11.3279381634523,15.));
#35183=CARTESIAN_POINT('Ctrl Pts',(-19.2998466936739,11.2502363198588,15.));
#35184=CARTESIAN_POINT('Ctrl Pts',(-19.2600675167206,11.1729790050543,15.));
#35185=CARTESIAN_POINT('Ctrl Pts',(-19.2198119937835,11.0961718903994,15.));
#35186=CARTESIAN_POINT('Ctrl Pts',(-19.1790795192393,11.0198210228993,15.));
#35187=CARTESIAN_POINT('Ctrl Pts',(-19.1378691901023,10.9439330179206,15.));
#35188=CARTESIAN_POINT('Ctrl Pts',(-19.0961797996403,10.868515097783,15.));
#35189=CARTESIAN_POINT('Ctrl Pts',(-19.0540100416943,10.7935747414879,15.));
#35190=CARTESIAN_POINT('Ctrl Pts',(-19.0113586878152,10.7191193896586,15.));
#35191=CARTESIAN_POINT('Ctrl Pts',(-18.9682247574834,10.6451561585969,15.));
#35192=CARTESIAN_POINT('Ctrl Pts',(-18.9246077453188,10.5716914651544,15.));
#35193=CARTESIAN_POINT('Ctrl Pts',(-18.8805076729356,10.4987309368494,15.));
#35194=CARTESIAN_POINT('Ctrl Pts',(-18.8359245594214,10.4262802670211,15.));
#35195=CARTESIAN_POINT('Ctrl Pts',(-18.7908579693851,10.3543459451258,15.));
#35196=CARTESIAN_POINT('Ctrl Pts',(-18.7453065790062,10.2829359603685,15.));
#35197=CARTESIAN_POINT('Ctrl Pts',(-18.699267629819,10.2120606864872,15.));
#35198=CARTESIAN_POINT('Ctrl Pts',(-18.6527367592664,10.1417331637795,15.));
#35199=CARTESIAN_POINT('Ctrl Pts',(-18.605709190442,10.0719672018851,15.));
#35200=CARTESIAN_POINT('Ctrl Pts',(-18.5581807679204,10.0027757313807,15.));
#35201=CARTESIAN_POINT('Ctrl Pts',(-18.5101489409161,9.93416923996829,15.));
#35202=CARTESIAN_POINT('Ctrl Pts',(-18.461614050347,9.86615372541685,15.));
#35203=CARTESIAN_POINT('Ctrl Pts',(-18.4125796444662,9.79873019947434,15.));
#35204=CARTESIAN_POINT('Ctrl Pts',(-18.3630495772677,9.73189932619939,15.));
#35205=CARTESIAN_POINT('Ctrl Pts',(-18.3130254811852,9.6656654640326,15.));
#35206=CARTESIAN_POINT('Ctrl Pts',(-18.2625044208165,9.60004042085347,15.));
#35207=CARTESIAN_POINT('Ctrl Pts',(-18.2114756946126,9.53504856811685,15.));
#35208=CARTESIAN_POINT('Ctrl Pts',(-18.1599204445014,9.47072748065832,15.));
#35209=CARTESIAN_POINT('Ctrl Pts',(-18.1078184146735,9.40711718355464,15.));
#35210=CARTESIAN_POINT('Ctrl Pts',(-18.0551538338035,9.34425079614396,15.));
#35211=CARTESIAN_POINT('Ctrl Pts',(-18.0019206847747,9.28214615574471,15.));
#35212=CARTESIAN_POINT('Ctrl Pts',(-17.9481305624284,9.22079331175917,15.));
#35213=CARTESIAN_POINT('Ctrl Pts',(-17.8938116696237,9.1601561636161,15.));
#35214=CARTESIAN_POINT('Ctrl Pts',(-17.8389924349283,9.10019864472208,15.));
#35215=CARTESIAN_POINT('Ctrl Pts',(-17.7836872744016,9.04090748239097,15.));
#35216=CARTESIAN_POINT('Ctrl Pts',(-17.7278841963319,8.98231202490686,15.));
#35217=CARTESIAN_POINT('Ctrl Pts',(-17.6715250120654,8.92451585185175,15.));
#35218=CARTESIAN_POINT('Ctrl Pts',(-17.614513388992,8.86768402115344,15.));
#35219=CARTESIAN_POINT('Ctrl Pts',(-17.5567525798882,8.81198307239551,15.));
#35220=CARTESIAN_POINT('Ctrl Pts',(-17.4981785296199,8.75752832625954,15.));
#35221=CARTESIAN_POINT('Ctrl Pts',(-17.438788019753,8.70433925112174,15.));
#35222=CARTESIAN_POINT('Ctrl Pts',(-17.3786861166843,8.65226368112816,15.));
#35223=CARTESIAN_POINT('Ctrl Pts',(-17.3180459442745,8.60104338529165,15.));
#35224=CARTESIAN_POINT('Ctrl Pts',(-17.2570167183611,8.55046295192433,15.));
#35225=CARTESIAN_POINT('Ctrl Pts',(-17.1956428575086,8.50048099003883,15.));
#35226=CARTESIAN_POINT('Ctrl Pts',(-17.1337886602855,8.45135198307877,15.));
#35227=CARTESIAN_POINT('Ctrl Pts',(-17.071033847921,8.40379607744266,15.));
#35228=CARTESIAN_POINT('Ctrl Pts',(-17.0067806259695,8.35882146841244,15.));
#35229=CARTESIAN_POINT('Ctrl Pts',(-16.9536879065132,8.32573081382563,15.));
#35230=CARTESIAN_POINT('Ctrl Pts',(-16.9126979078877,8.30290517019115,15.));
#35231=CARTESIAN_POINT('Ctrl Pts',(-16.8848228151885,8.28862062120315,15.));
#35232=CARTESIAN_POINT('Ctrl Pts',(-16.8707481591095,8.28171148831561,15.));
#35233=CARTESIAN_POINT('',(-20.0837475345525,13.1393715591102,0.));
#35234=CARTESIAN_POINT('Origin',(-9.33709008296438E-14,6.79236997764462E-14,
0.));
#35235=CARTESIAN_POINT('',(-18.7025042402277,15.040489857191,0.));
#35236=CARTESIAN_POINT('Origin',(-9.33709008296438E-14,6.79236997764462E-14,
0.));
#35237=CARTESIAN_POINT('',(-18.7025042402277,15.040489857191,15.));
#35238=CARTESIAN_POINT('Origin',(-9.33709008296438E-14,6.79236997764462E-14,
15.));
#35239=CARTESIAN_POINT('',(-18.7025042402277,15.040489857191,0.));
#35240=CARTESIAN_POINT('Ctrl Pts',(-13.0897235660237,13.4858453790958,0.));
#35241=CARTESIAN_POINT('Ctrl Pts',(-13.0897235660237,13.4858453790958,18.));
#35242=CARTESIAN_POINT('Ctrl Pts',(-13.1006438497967,13.4970961329957,0.));
#35243=CARTESIAN_POINT('Ctrl Pts',(-13.1006438497967,13.4970961329957,18.));
#35244=CARTESIAN_POINT('Ctrl Pts',(-13.1228431405579,13.5191927531554,0.));
#35245=CARTESIAN_POINT('Ctrl Pts',(-13.1228431405579,13.5191927531554,18.));
#35246=CARTESIAN_POINT('Ctrl Pts',(-13.1572182238498,13.5511230466604,0.));
#35247=CARTESIAN_POINT('Ctrl Pts',(-13.1572182238498,13.5511230466604,18.));
#35248=CARTESIAN_POINT('Ctrl Pts',(-13.2050958591127,13.5913916488449,0.));
#35249=CARTESIAN_POINT('Ctrl Pts',(-13.2050958591127,13.5913916488449,18.));
#35250=CARTESIAN_POINT('Ctrl Pts',(-13.267724591625,13.6386021757691,0.));
#35251=CARTESIAN_POINT('Ctrl Pts',(-13.267724591625,13.6386021757691,18.));
#35252=CARTESIAN_POINT('Ctrl Pts',(-13.332345249068,13.6835899659728,0.));
#35253=CARTESIAN_POINT('Ctrl Pts',(-13.332345249068,13.6835899659728,18.));
#35254=CARTESIAN_POINT('Ctrl Pts',(-13.3981837093918,13.7272351052346,0.));
#35255=CARTESIAN_POINT('Ctrl Pts',(-13.3981837093918,13.7272351052346,18.));
#35256=CARTESIAN_POINT('Ctrl Pts',(-13.4646849459541,13.7701598398937,0.));
#35257=CARTESIAN_POINT('Ctrl Pts',(-13.4646849459541,13.7701598398937,18.));
#35258=CARTESIAN_POINT('Ctrl Pts',(-13.5316488646659,13.8125718693898,0.));
#35259=CARTESIAN_POINT('Ctrl Pts',(-13.5316488646659,13.8125718693898,18.));
#35260=CARTESIAN_POINT('Ctrl Pts',(-13.5991011046042,13.854416158639,0.));
#35261=CARTESIAN_POINT('Ctrl Pts',(-13.5991011046042,13.854416158639,18.));
#35262=CARTESIAN_POINT('Ctrl Pts',(-13.6672004242289,13.8954842290745,0.));
#35263=CARTESIAN_POINT('Ctrl Pts',(-13.6672004242289,13.8954842290745,18.));
#35264=CARTESIAN_POINT('Ctrl Pts',(-13.7361389175879,13.9355316323567,0.));
#35265=CARTESIAN_POINT('Ctrl Pts',(-13.7361389175879,13.9355316323567,18.));
#35266=CARTESIAN_POINT('Ctrl Pts',(-13.806028835706,13.9744114225699,0.));
#35267=CARTESIAN_POINT('Ctrl Pts',(-13.806028835706,13.9744114225699,18.));
#35268=CARTESIAN_POINT('Ctrl Pts',(-13.876852657608,14.0121326766855,0.));
#35269=CARTESIAN_POINT('Ctrl Pts',(-13.876852657608,14.0121326766855,18.));
#35270=CARTESIAN_POINT('Ctrl Pts',(-13.9485205009332,14.0487919508068,0.));
#35271=CARTESIAN_POINT('Ctrl Pts',(-13.9485205009332,14.0487919508068,18.));
#35272=CARTESIAN_POINT('Ctrl Pts',(-14.0209038736616,14.0845327205726,0.));
#35273=CARTESIAN_POINT('Ctrl Pts',(-14.0209038736616,14.0845327205726,18.));
#35274=CARTESIAN_POINT('Ctrl Pts',(-14.0938755647891,14.1194976094444,0.));
#35275=CARTESIAN_POINT('Ctrl Pts',(-14.0938755647891,14.1194976094444,18.));
#35276=CARTESIAN_POINT('Ctrl Pts',(-14.1673550455622,14.1537739659715,0.));
#35277=CARTESIAN_POINT('Ctrl Pts',(-14.1673550455622,14.1537739659715,18.));
#35278=CARTESIAN_POINT('Ctrl Pts',(-14.2413181097468,14.1873822640681,0.));
#35279=CARTESIAN_POINT('Ctrl Pts',(-14.2413181097468,14.1873822640681,18.));
#35280=CARTESIAN_POINT('Ctrl Pts',(-14.3157729256101,14.2203046917613,0.));
#35281=CARTESIAN_POINT('Ctrl Pts',(-14.3157729256101,14.2203046917613,18.));
#35282=CARTESIAN_POINT('Ctrl Pts',(-14.3907450096103,14.2525030666863,0.));
#35283=CARTESIAN_POINT('Ctrl Pts',(-14.3907450096103,14.2525030666863,18.));
#35284=CARTESIAN_POINT('Ctrl Pts',(-14.4662599802682,14.2839394106401,0.));
#35285=CARTESIAN_POINT('Ctrl Pts',(-14.4662599802682,14.2839394106401,18.));
#35286=CARTESIAN_POINT('Ctrl Pts',(-14.5423237181615,14.3145996213697,0.));
#35287=CARTESIAN_POINT('Ctrl Pts',(-14.5423237181615,14.3145996213697,18.));
#35288=CARTESIAN_POINT('Ctrl Pts',(-14.6189211183837,14.3444949335274,0.));
#35289=CARTESIAN_POINT('Ctrl Pts',(-14.6189211183837,14.3444949335274,18.));
#35290=CARTESIAN_POINT('Ctrl Pts',(-14.6960255561799,14.3736505809735,0.));
#35291=CARTESIAN_POINT('Ctrl Pts',(-14.6960255561799,14.3736505809735,18.));
#35292=CARTESIAN_POINT('Ctrl Pts',(-14.7736052248294,14.4020981965564,0.));
#35293=CARTESIAN_POINT('Ctrl Pts',(-14.7736052248294,14.4020981965564,18.));
#35294=CARTESIAN_POINT('Ctrl Pts',(-14.8516302160049,14.4298673266313,0.));
#35295=CARTESIAN_POINT('Ctrl Pts',(-14.8516302160049,14.4298673266313,18.));
#35296=CARTESIAN_POINT('Ctrl Pts',(-14.9300806580357,14.4569756801697,0.));
#35297=CARTESIAN_POINT('Ctrl Pts',(-14.9300806580357,14.4569756801697,18.));
#35298=CARTESIAN_POINT('Ctrl Pts',(-15.0089462280504,14.4834296977405,0.));
#35299=CARTESIAN_POINT('Ctrl Pts',(-15.0089462280504,14.4834296977405,18.));
#35300=CARTESIAN_POINT('Ctrl Pts',(-15.0882222764759,14.5092291736391,0.));
#35301=CARTESIAN_POINT('Ctrl Pts',(-15.0882222764759,14.5092291736391,18.));
#35302=CARTESIAN_POINT('Ctrl Pts',(-15.1679069808052,14.5343706477051,0.));
#35303=CARTESIAN_POINT('Ctrl Pts',(-15.1679069808052,14.5343706477051,18.));
#35304=CARTESIAN_POINT('Ctrl Pts',(-15.2479982823383,14.5588510579962,0.));
#35305=CARTESIAN_POINT('Ctrl Pts',(-15.2479982823383,14.5588510579962,18.));
#35306=CARTESIAN_POINT('Ctrl Pts',(-15.3284903715086,14.5826719336929,0.));
#35307=CARTESIAN_POINT('Ctrl Pts',(-15.3284903715086,14.5826719336929,18.));
#35308=CARTESIAN_POINT('Ctrl Pts',(-15.4093740621547,14.6058389416146,0.));
#35309=CARTESIAN_POINT('Ctrl Pts',(-15.4093740621547,14.6058389416146,18.));
#35310=CARTESIAN_POINT('Ctrl Pts',(-15.4906383406647,14.6283600295736,0.));
#35311=CARTESIAN_POINT('Ctrl Pts',(-15.4906383406647,14.6283600295736,18.));
#35312=CARTESIAN_POINT('Ctrl Pts',(-15.5722715494357,14.6502440080912,0.));
#35313=CARTESIAN_POINT('Ctrl Pts',(-15.5722715494357,14.6502440080912,18.));
#35314=CARTESIAN_POINT('Ctrl Pts',(-15.6542626345121,14.6714990558793,0.));
#35315=CARTESIAN_POINT('Ctrl Pts',(-15.6542626345121,14.6714990558793,18.));
#35316=CARTESIAN_POINT('Ctrl Pts',(-15.7366025822956,14.692131002056,0.));
#35317=CARTESIAN_POINT('Ctrl Pts',(-15.7366025822956,14.692131002056,18.));
#35318=CARTESIAN_POINT('Ctrl Pts',(-15.8192842036838,14.7121435744495,0.));
#35319=CARTESIAN_POINT('Ctrl Pts',(-15.8192842036838,14.7121435744495,18.));
#35320=CARTESIAN_POINT('Ctrl Pts',(-15.9023014613802,14.7315391924939,0.));
#35321=CARTESIAN_POINT('Ctrl Pts',(-15.9023014613802,14.7315391924939,18.));
#35322=CARTESIAN_POINT('Ctrl Pts',(-15.9856489347991,14.7503195973741,0.));
#35323=CARTESIAN_POINT('Ctrl Pts',(-15.9856489347991,14.7503195973741,18.));
#35324=CARTESIAN_POINT('Ctrl Pts',(-16.0693212651732,14.7684865075326,0.));
#35325=CARTESIAN_POINT('Ctrl Pts',(-16.0693212651732,14.7684865075326,18.));
#35326=CARTESIAN_POINT('Ctrl Pts',(-16.1533125058853,14.7860423865308,0.));
#35327=CARTESIAN_POINT('Ctrl Pts',(-16.1533125058853,14.7860423865308,18.));
#35328=CARTESIAN_POINT('Ctrl Pts',(-16.2376161919272,14.8029903659562,0.));
#35329=CARTESIAN_POINT('Ctrl Pts',(-16.2376161919272,14.8029903659562,18.));
#35330=CARTESIAN_POINT('Ctrl Pts',(-16.3222256264574,14.8193339134125,0.));
#35331=CARTESIAN_POINT('Ctrl Pts',(-16.3222256264574,14.8193339134125,18.));
#35332=CARTESIAN_POINT('Ctrl Pts',(-16.4071341001481,14.8350765822692,0.));
#35333=CARTESIAN_POINT('Ctrl Pts',(-16.4071341001481,14.8350765822692,18.));
#35334=CARTESIAN_POINT('Ctrl Pts',(-16.492335117066,14.8502217520165,0.));
#35335=CARTESIAN_POINT('Ctrl Pts',(-16.492335117066,14.8502217520165,18.));
#35336=CARTESIAN_POINT('Ctrl Pts',(-16.5778226646614,14.8647723257055,0.));
#35337=CARTESIAN_POINT('Ctrl Pts',(-16.5778226646614,14.8647723257055,18.));
#35338=CARTESIAN_POINT('Ctrl Pts',(-16.6635911790385,14.8787307479454,0.));
#35339=CARTESIAN_POINT('Ctrl Pts',(-16.6635911790385,14.8787307479454,18.));
#35340=CARTESIAN_POINT('Ctrl Pts',(-16.7496353900706,14.8920991518626,0.));
#35341=CARTESIAN_POINT('Ctrl Pts',(-16.7496353900706,14.8920991518626,18.));
#35342=CARTESIAN_POINT('Ctrl Pts',(-16.8359501981915,14.9048794721647,0.));
#35343=CARTESIAN_POINT('Ctrl Pts',(-16.8359501981915,14.9048794721647,18.));
#35344=CARTESIAN_POINT('Ctrl Pts',(-16.9225305499155,14.9170735658747,0.));
#35345=CARTESIAN_POINT('Ctrl Pts',(-16.9225305499155,14.9170735658747,18.));
#35346=CARTESIAN_POINT('Ctrl Pts',(-17.0093712776822,14.9286833603319,0.));
#35347=CARTESIAN_POINT('Ctrl Pts',(-17.0093712776822,14.9286833603319,18.));
#35348=CARTESIAN_POINT('Ctrl Pts',(-17.0964671184813,14.9397108660998,0.));
#35349=CARTESIAN_POINT('Ctrl Pts',(-17.0964671184813,14.9397108660998,18.));
#35350=CARTESIAN_POINT('Ctrl Pts',(-17.1838128327073,14.9501581118289,0.));
#35351=CARTESIAN_POINT('Ctrl Pts',(-17.1838128327073,14.9501581118289,18.));
#35352=CARTESIAN_POINT('Ctrl Pts',(-17.2714032968314,14.9600271060471,0.));
#35353=CARTESIAN_POINT('Ctrl Pts',(-17.2714032968314,14.9600271060471,18.));
#35354=CARTESIAN_POINT('Ctrl Pts',(-17.3592335908102,14.9693197947387,0.));
#35355=CARTESIAN_POINT('Ctrl Pts',(-17.3592335908102,14.9693197947387,18.));
#35356=CARTESIAN_POINT('Ctrl Pts',(-17.4472991215239,14.9780380183576,0.));
#35357=CARTESIAN_POINT('Ctrl Pts',(-17.4472991215239,14.9780380183576,18.));
#35358=CARTESIAN_POINT('Ctrl Pts',(-17.5355955872257,14.9861834999847,0.));
#35359=CARTESIAN_POINT('Ctrl Pts',(-17.5355955872257,14.9861834999847,18.));
#35360=CARTESIAN_POINT('Ctrl Pts',(-17.6241187988652,14.9937578646616,0.));
#35361=CARTESIAN_POINT('Ctrl Pts',(-17.6241187988652,14.9937578646616,18.));
#35362=CARTESIAN_POINT('Ctrl Pts',(-17.7128645299878,15.0007626541287,0.));
#35363=CARTESIAN_POINT('Ctrl Pts',(-17.7128645299878,15.0007626541287,18.));
#35364=CARTESIAN_POINT('Ctrl Pts',(-17.8018283748074,15.0071993464636,0.));
#35365=CARTESIAN_POINT('Ctrl Pts',(-17.8018283748074,15.0071993464636,18.));
#35366=CARTESIAN_POINT('Ctrl Pts',(-17.891005548971,15.0130693803259,0.));
#35367=CARTESIAN_POINT('Ctrl Pts',(-17.891005548971,15.0130693803259,18.));
#35368=CARTESIAN_POINT('Ctrl Pts',(-17.980390892286,15.0183741723687,0.));
#35369=CARTESIAN_POINT('Ctrl Pts',(-17.980390892286,15.0183741723687,18.));
#35370=CARTESIAN_POINT('Ctrl Pts',(-18.0699792164192,15.0231151183906,0.));
#35371=CARTESIAN_POINT('Ctrl Pts',(-18.0699792164192,15.0231151183906,18.));
#35372=CARTESIAN_POINT('Ctrl Pts',(-18.1597655779328,15.0272936035154,0.));
#35373=CARTESIAN_POINT('Ctrl Pts',(-18.1597655779328,15.0272936035154,18.));
#35374=CARTESIAN_POINT('Ctrl Pts',(-18.2497455679917,15.0309110092482,0.));
#35375=CARTESIAN_POINT('Ctrl Pts',(-18.2497455679917,15.0309110092482,18.));
#35376=CARTESIAN_POINT('Ctrl Pts',(-18.3399156227477,15.0339687345357,0.));
#35377=CARTESIAN_POINT('Ctrl Pts',(-18.3399156227477,15.0339687345357,18.));
#35378=CARTESIAN_POINT('Ctrl Pts',(-18.430273237144,15.0364681891201,0.));
#35379=CARTESIAN_POINT('Ctrl Pts',(-18.430273237144,15.0364681891201,18.));
#35380=CARTESIAN_POINT('Ctrl Pts',(-18.5208167514208,15.0384106640282,0.));
#35381=CARTESIAN_POINT('Ctrl Pts',(-18.5208167514208,15.0384106640282,18.));
#35382=CARTESIAN_POINT('Ctrl Pts',(-18.5933995108277,15.0395199113665,0.));
#35383=CARTESIAN_POINT('Ctrl Pts',(-18.5933995108277,15.0395199113665,18.));
#35384=CARTESIAN_POINT('Ctrl Pts',(-18.6479196005666,15.0401020105546,0.));
#35385=CARTESIAN_POINT('Ctrl Pts',(-18.6479196005666,15.0401020105546,18.));
#35386=CARTESIAN_POINT('Ctrl Pts',(-18.6843032127312,15.0403790752228,0.));
#35387=CARTESIAN_POINT('Ctrl Pts',(-18.6843032127312,15.0403790752228,18.));
#35388=CARTESIAN_POINT('Ctrl Pts',(-18.7025042402277,15.0404898571911,0.));
#35389=CARTESIAN_POINT('Ctrl Pts',(-18.7025042402277,15.0404898571911,18.));
#35390=CARTESIAN_POINT('Ctrl Pts',(-13.0897235660237,13.4858453790958,0.));
#35391=CARTESIAN_POINT('Ctrl Pts',(-13.1006438497967,13.4970961329957,0.));
#35392=CARTESIAN_POINT('Ctrl Pts',(-13.1228431405579,13.5191927531554,0.));
#35393=CARTESIAN_POINT('Ctrl Pts',(-13.1572182238498,13.5511230466604,0.));
#35394=CARTESIAN_POINT('Ctrl Pts',(-13.2050958591127,13.5913916488449,0.));
#35395=CARTESIAN_POINT('Ctrl Pts',(-13.267724591625,13.6386021757691,0.));
#35396=CARTESIAN_POINT('Ctrl Pts',(-13.332345249068,13.6835899659728,0.));
#35397=CARTESIAN_POINT('Ctrl Pts',(-13.3981837093918,13.7272351052346,0.));
#35398=CARTESIAN_POINT('Ctrl Pts',(-13.4646849459541,13.7701598398937,0.));
#35399=CARTESIAN_POINT('Ctrl Pts',(-13.5316488646659,13.8125718693898,0.));
#35400=CARTESIAN_POINT('Ctrl Pts',(-13.5991011046042,13.854416158639,0.));
#35401=CARTESIAN_POINT('Ctrl Pts',(-13.6672004242289,13.8954842290745,0.));
#35402=CARTESIAN_POINT('Ctrl Pts',(-13.7361389175879,13.9355316323567,0.));
#35403=CARTESIAN_POINT('Ctrl Pts',(-13.806028835706,13.9744114225699,0.));
#35404=CARTESIAN_POINT('Ctrl Pts',(-13.876852657608,14.0121326766855,0.));
#35405=CARTESIAN_POINT('Ctrl Pts',(-13.9485205009332,14.0487919508068,0.));
#35406=CARTESIAN_POINT('Ctrl Pts',(-14.0209038736616,14.0845327205726,0.));
#35407=CARTESIAN_POINT('Ctrl Pts',(-14.0938755647891,14.1194976094444,0.));
#35408=CARTESIAN_POINT('Ctrl Pts',(-14.1673550455622,14.1537739659715,0.));
#35409=CARTESIAN_POINT('Ctrl Pts',(-14.2413181097468,14.1873822640681,0.));
#35410=CARTESIAN_POINT('Ctrl Pts',(-14.3157729256101,14.2203046917613,0.));
#35411=CARTESIAN_POINT('Ctrl Pts',(-14.3907450096103,14.2525030666863,0.));
#35412=CARTESIAN_POINT('Ctrl Pts',(-14.4662599802682,14.2839394106401,0.));
#35413=CARTESIAN_POINT('Ctrl Pts',(-14.5423237181615,14.3145996213697,0.));
#35414=CARTESIAN_POINT('Ctrl Pts',(-14.6189211183837,14.3444949335274,0.));
#35415=CARTESIAN_POINT('Ctrl Pts',(-14.6960255561799,14.3736505809735,0.));
#35416=CARTESIAN_POINT('Ctrl Pts',(-14.7736052248294,14.4020981965564,0.));
#35417=CARTESIAN_POINT('Ctrl Pts',(-14.8516302160049,14.4298673266313,0.));
#35418=CARTESIAN_POINT('Ctrl Pts',(-14.9300806580357,14.4569756801697,0.));
#35419=CARTESIAN_POINT('Ctrl Pts',(-15.0089462280504,14.4834296977405,0.));
#35420=CARTESIAN_POINT('Ctrl Pts',(-15.0882222764759,14.5092291736391,0.));
#35421=CARTESIAN_POINT('Ctrl Pts',(-15.1679069808052,14.5343706477051,0.));
#35422=CARTESIAN_POINT('Ctrl Pts',(-15.2479982823383,14.5588510579962,0.));
#35423=CARTESIAN_POINT('Ctrl Pts',(-15.3284903715086,14.5826719336929,0.));
#35424=CARTESIAN_POINT('Ctrl Pts',(-15.4093740621547,14.6058389416146,0.));
#35425=CARTESIAN_POINT('Ctrl Pts',(-15.4906383406647,14.6283600295736,0.));
#35426=CARTESIAN_POINT('Ctrl Pts',(-15.5722715494357,14.6502440080912,0.));
#35427=CARTESIAN_POINT('Ctrl Pts',(-15.6542626345121,14.6714990558793,0.));
#35428=CARTESIAN_POINT('Ctrl Pts',(-15.7366025822956,14.692131002056,0.));
#35429=CARTESIAN_POINT('Ctrl Pts',(-15.8192842036838,14.7121435744495,0.));
#35430=CARTESIAN_POINT('Ctrl Pts',(-15.9023014613802,14.7315391924939,0.));
#35431=CARTESIAN_POINT('Ctrl Pts',(-15.9856489347991,14.7503195973741,0.));
#35432=CARTESIAN_POINT('Ctrl Pts',(-16.0693212651732,14.7684865075326,0.));
#35433=CARTESIAN_POINT('Ctrl Pts',(-16.1533125058853,14.7860423865308,0.));
#35434=CARTESIAN_POINT('Ctrl Pts',(-16.2376161919272,14.8029903659562,0.));
#35435=CARTESIAN_POINT('Ctrl Pts',(-16.3222256264574,14.8193339134125,0.));
#35436=CARTESIAN_POINT('Ctrl Pts',(-16.4071341001481,14.8350765822692,0.));
#35437=CARTESIAN_POINT('Ctrl Pts',(-16.492335117066,14.8502217520165,0.));
#35438=CARTESIAN_POINT('Ctrl Pts',(-16.5778226646614,14.8647723257055,0.));
#35439=CARTESIAN_POINT('Ctrl Pts',(-16.6635911790385,14.8787307479454,0.));
#35440=CARTESIAN_POINT('Ctrl Pts',(-16.7496353900706,14.8920991518626,0.));
#35441=CARTESIAN_POINT('Ctrl Pts',(-16.8359501981915,14.9048794721647,0.));
#35442=CARTESIAN_POINT('Ctrl Pts',(-16.9225305499155,14.9170735658747,0.));
#35443=CARTESIAN_POINT('Ctrl Pts',(-17.0093712776822,14.9286833603319,0.));
#35444=CARTESIAN_POINT('Ctrl Pts',(-17.0964671184813,14.9397108660998,0.));
#35445=CARTESIAN_POINT('Ctrl Pts',(-17.1838128327073,14.9501581118289,0.));
#35446=CARTESIAN_POINT('Ctrl Pts',(-17.2714032968314,14.9600271060471,0.));
#35447=CARTESIAN_POINT('Ctrl Pts',(-17.3592335908102,14.9693197947387,0.));
#35448=CARTESIAN_POINT('Ctrl Pts',(-17.4472991215239,14.9780380183576,0.));
#35449=CARTESIAN_POINT('Ctrl Pts',(-17.5355955872257,14.9861834999847,0.));
#35450=CARTESIAN_POINT('Ctrl Pts',(-17.6241187988652,14.9937578646616,0.));
#35451=CARTESIAN_POINT('Ctrl Pts',(-17.7128645299878,15.0007626541287,0.));
#35452=CARTESIAN_POINT('Ctrl Pts',(-17.8018283748074,15.0071993464636,0.));
#35453=CARTESIAN_POINT('Ctrl Pts',(-17.891005548971,15.0130693803259,0.));
#35454=CARTESIAN_POINT('Ctrl Pts',(-17.980390892286,15.0183741723687,0.));
#35455=CARTESIAN_POINT('Ctrl Pts',(-18.0699792164192,15.0231151183906,0.));
#35456=CARTESIAN_POINT('Ctrl Pts',(-18.1597655779328,15.0272936035154,0.));
#35457=CARTESIAN_POINT('Ctrl Pts',(-18.2497455679917,15.0309110092482,0.));
#35458=CARTESIAN_POINT('Ctrl Pts',(-18.3399156227477,15.0339687345357,0.));
#35459=CARTESIAN_POINT('Ctrl Pts',(-18.4483447600233,15.036968080037,0.));
#35460=CARTESIAN_POINT('Ctrl Pts',(-18.5389347492702,15.038771310026,0.));
#35461=CARTESIAN_POINT('Ctrl Pts',(-18.6115544313469,15.0397694451467,0.));
#35462=CARTESIAN_POINT('Ctrl Pts',(-18.6661021851765,15.0402682932586,0.));
#35463=CARTESIAN_POINT('Ctrl Pts',(-18.7025042402277,15.0404898571911,0.));
#35464=CARTESIAN_POINT('Ctrl Pts',(-13.0897235660237,13.4858453790958,15.));
#35465=CARTESIAN_POINT('Ctrl Pts',(-13.1006438497967,13.4970961329957,15.));
#35466=CARTESIAN_POINT('Ctrl Pts',(-13.1228431405579,13.5191927531554,15.));
#35467=CARTESIAN_POINT('Ctrl Pts',(-13.1572182238498,13.5511230466604,15.));
#35468=CARTESIAN_POINT('Ctrl Pts',(-13.2050958591127,13.5913916488449,15.));
#35469=CARTESIAN_POINT('Ctrl Pts',(-13.267724591625,13.6386021757691,15.));
#35470=CARTESIAN_POINT('Ctrl Pts',(-13.332345249068,13.6835899659728,15.));
#35471=CARTESIAN_POINT('Ctrl Pts',(-13.3981837093918,13.7272351052346,15.));
#35472=CARTESIAN_POINT('Ctrl Pts',(-13.4646849459541,13.7701598398937,15.));
#35473=CARTESIAN_POINT('Ctrl Pts',(-13.5316488646659,13.8125718693898,15.));
#35474=CARTESIAN_POINT('Ctrl Pts',(-13.5991011046042,13.854416158639,15.));
#35475=CARTESIAN_POINT('Ctrl Pts',(-13.6672004242289,13.8954842290745,15.));
#35476=CARTESIAN_POINT('Ctrl Pts',(-13.7361389175879,13.9355316323567,15.));
#35477=CARTESIAN_POINT('Ctrl Pts',(-13.806028835706,13.9744114225699,15.));
#35478=CARTESIAN_POINT('Ctrl Pts',(-13.876852657608,14.0121326766855,15.));
#35479=CARTESIAN_POINT('Ctrl Pts',(-13.9485205009332,14.0487919508068,15.));
#35480=CARTESIAN_POINT('Ctrl Pts',(-14.0209038736616,14.0845327205726,15.));
#35481=CARTESIAN_POINT('Ctrl Pts',(-14.0938755647891,14.1194976094444,15.));
#35482=CARTESIAN_POINT('Ctrl Pts',(-14.1673550455622,14.1537739659715,15.));
#35483=CARTESIAN_POINT('Ctrl Pts',(-14.2413181097468,14.1873822640681,15.));
#35484=CARTESIAN_POINT('Ctrl Pts',(-14.3157729256101,14.2203046917613,15.));
#35485=CARTESIAN_POINT('Ctrl Pts',(-14.3907450096103,14.2525030666863,15.));
#35486=CARTESIAN_POINT('Ctrl Pts',(-14.4662599802682,14.2839394106401,15.));
#35487=CARTESIAN_POINT('Ctrl Pts',(-14.5423237181615,14.3145996213697,15.));
#35488=CARTESIAN_POINT('Ctrl Pts',(-14.6189211183837,14.3444949335274,15.));
#35489=CARTESIAN_POINT('Ctrl Pts',(-14.6960255561799,14.3736505809735,15.));
#35490=CARTESIAN_POINT('Ctrl Pts',(-14.7736052248294,14.4020981965564,15.));
#35491=CARTESIAN_POINT('Ctrl Pts',(-14.8516302160049,14.4298673266313,15.));
#35492=CARTESIAN_POINT('Ctrl Pts',(-14.9300806580357,14.4569756801697,15.));
#35493=CARTESIAN_POINT('Ctrl Pts',(-15.0089462280504,14.4834296977405,15.));
#35494=CARTESIAN_POINT('Ctrl Pts',(-15.0882222764759,14.5092291736391,15.));
#35495=CARTESIAN_POINT('Ctrl Pts',(-15.1679069808052,14.5343706477051,15.));
#35496=CARTESIAN_POINT('Ctrl Pts',(-15.2479982823383,14.5588510579962,15.));
#35497=CARTESIAN_POINT('Ctrl Pts',(-15.3284903715086,14.5826719336929,15.));
#35498=CARTESIAN_POINT('Ctrl Pts',(-15.4093740621547,14.6058389416146,15.));
#35499=CARTESIAN_POINT('Ctrl Pts',(-15.4906383406647,14.6283600295736,15.));
#35500=CARTESIAN_POINT('Ctrl Pts',(-15.5722715494357,14.6502440080912,15.));
#35501=CARTESIAN_POINT('Ctrl Pts',(-15.6542626345121,14.6714990558793,15.));
#35502=CARTESIAN_POINT('Ctrl Pts',(-15.7366025822956,14.692131002056,15.));
#35503=CARTESIAN_POINT('Ctrl Pts',(-15.8192842036838,14.7121435744495,15.));
#35504=CARTESIAN_POINT('Ctrl Pts',(-15.9023014613802,14.7315391924939,15.));
#35505=CARTESIAN_POINT('Ctrl Pts',(-15.9856489347991,14.7503195973741,15.));
#35506=CARTESIAN_POINT('Ctrl Pts',(-16.0693212651732,14.7684865075326,15.));
#35507=CARTESIAN_POINT('Ctrl Pts',(-16.1533125058853,14.7860423865308,15.));
#35508=CARTESIAN_POINT('Ctrl Pts',(-16.2376161919272,14.8029903659562,15.));
#35509=CARTESIAN_POINT('Ctrl Pts',(-16.3222256264574,14.8193339134125,15.));
#35510=CARTESIAN_POINT('Ctrl Pts',(-16.4071341001481,14.8350765822692,15.));
#35511=CARTESIAN_POINT('Ctrl Pts',(-16.492335117066,14.8502217520165,15.));
#35512=CARTESIAN_POINT('Ctrl Pts',(-16.5778226646614,14.8647723257055,15.));
#35513=CARTESIAN_POINT('Ctrl Pts',(-16.6635911790385,14.8787307479454,15.));
#35514=CARTESIAN_POINT('Ctrl Pts',(-16.7496353900706,14.8920991518626,15.));
#35515=CARTESIAN_POINT('Ctrl Pts',(-16.8359501981915,14.9048794721647,15.));
#35516=CARTESIAN_POINT('Ctrl Pts',(-16.9225305499155,14.9170735658747,15.));
#35517=CARTESIAN_POINT('Ctrl Pts',(-17.0093712776822,14.9286833603319,15.));
#35518=CARTESIAN_POINT('Ctrl Pts',(-17.0964671184813,14.9397108660998,15.));
#35519=CARTESIAN_POINT('Ctrl Pts',(-17.1838128327073,14.9501581118289,15.));
#35520=CARTESIAN_POINT('Ctrl Pts',(-17.2714032968314,14.9600271060471,15.));
#35521=CARTESIAN_POINT('Ctrl Pts',(-17.3592335908102,14.9693197947387,15.));
#35522=CARTESIAN_POINT('Ctrl Pts',(-17.4472991215239,14.9780380183576,15.));
#35523=CARTESIAN_POINT('Ctrl Pts',(-17.5355955872257,14.9861834999847,15.));
#35524=CARTESIAN_POINT('Ctrl Pts',(-17.6241187988652,14.9937578646616,15.));
#35525=CARTESIAN_POINT('Ctrl Pts',(-17.7128645299878,15.0007626541287,15.));
#35526=CARTESIAN_POINT('Ctrl Pts',(-17.8018283748074,15.0071993464636,15.));
#35527=CARTESIAN_POINT('Ctrl Pts',(-17.891005548971,15.0130693803259,15.));
#35528=CARTESIAN_POINT('Ctrl Pts',(-17.980390892286,15.0183741723687,15.));
#35529=CARTESIAN_POINT('Ctrl Pts',(-18.0699792164192,15.0231151183906,15.));
#35530=CARTESIAN_POINT('Ctrl Pts',(-18.1597655779328,15.0272936035154,15.));
#35531=CARTESIAN_POINT('Ctrl Pts',(-18.2497455679917,15.0309110092482,15.));
#35532=CARTESIAN_POINT('Ctrl Pts',(-18.3399156227477,15.0339687345357,15.));
#35533=CARTESIAN_POINT('Ctrl Pts',(-18.4483447600233,15.036968080037,15.));
#35534=CARTESIAN_POINT('Ctrl Pts',(-18.5389347492702,15.038771310026,15.));
#35535=CARTESIAN_POINT('Ctrl Pts',(-18.6115544313469,15.0397694451467,15.));
#35536=CARTESIAN_POINT('Ctrl Pts',(-18.6661021851765,15.0402682932586,15.));
#35537=CARTESIAN_POINT('Ctrl Pts',(-18.7025042402277,15.0404898571911,15.));
#35538=CARTESIAN_POINT('Ctrl Pts',(-8.52496423935285,22.4349054983023,0.));
#35539=CARTESIAN_POINT('Ctrl Pts',(-8.52496423935285,22.4349054983023,18.));
#35540=CARTESIAN_POINT('Ctrl Pts',(-8.53048330625154,22.4175610589877,0.));
#35541=CARTESIAN_POINT('Ctrl Pts',(-8.53048330625154,22.4175610589877,18.));
#35542=CARTESIAN_POINT('Ctrl Pts',(-8.54146295656906,22.3828725698612,0.));
#35543=CARTESIAN_POINT('Ctrl Pts',(-8.54146295656906,22.3828725698612,18.));
#35544=CARTESIAN_POINT('Ctrl Pts',(-8.55775698160722,22.3308410047044,0.));
#35545=CARTESIAN_POINT('Ctrl Pts',(-8.55775698160722,22.3308410047044,18.));
#35546=CARTESIAN_POINT('Ctrl Pts',(-8.57913133085326,22.2614679221214,0.));
#35547=CARTESIAN_POINT('Ctrl Pts',(-8.57913133085326,22.2614679221214,18.));
#35548=CARTESIAN_POINT('Ctrl Pts',(-8.60526341207613,22.1747556651024,0.));
#35549=CARTESIAN_POINT('Ctrl Pts',(-8.60526341207613,22.1747556651024,18.));
#35550=CARTESIAN_POINT('Ctrl Pts',(-8.63080832792612,22.0880480931906,0.));
#35551=CARTESIAN_POINT('Ctrl Pts',(-8.63080832792612,22.0880480931906,18.));
#35552=CARTESIAN_POINT('Ctrl Pts',(-8.6557643376698,22.0013463859623,0.));
#35553=CARTESIAN_POINT('Ctrl Pts',(-8.6557643376698,22.0013463859623,18.));
#35554=CARTESIAN_POINT('Ctrl Pts',(-8.68012932645739,21.9146524902336,0.));
#35555=CARTESIAN_POINT('Ctrl Pts',(-8.68012932645739,21.9146524902336,18.));
#35556=CARTESIAN_POINT('Ctrl Pts',(-8.70390086252202,21.8279693631274,0.));
#35557=CARTESIAN_POINT('Ctrl Pts',(-8.70390086252202,21.8279693631274,18.));
#35558=CARTESIAN_POINT('Ctrl Pts',(-8.72707626956921,21.7413007707864,0.));
#35559=CARTESIAN_POINT('Ctrl Pts',(-8.72707626956921,21.7413007707864,18.));
#35560=CARTESIAN_POINT('Ctrl Pts',(-8.74965270266163,21.6546509866725,0.));
#35561=CARTESIAN_POINT('Ctrl Pts',(-8.74965270266163,21.6546509866725,18.));
#35562=CARTESIAN_POINT('Ctrl Pts',(-8.77162723103298,21.5680245138584,0.));
#35563=CARTESIAN_POINT('Ctrl Pts',(-8.77162723103298,21.5680245138584,18.));
#35564=CARTESIAN_POINT('Ctrl Pts',(-8.79299691277858,21.481425822209,0.));
#35565=CARTESIAN_POINT('Ctrl Pts',(-8.79299691277858,21.481425822209,18.));
#35566=CARTESIAN_POINT('Ctrl Pts',(-8.81375890120581,21.3948590173441,0.));
#35567=CARTESIAN_POINT('Ctrl Pts',(-8.81375890120581,21.3948590173441,18.));
#35568=CARTESIAN_POINT('Ctrl Pts',(-8.83391042911628,21.3083278326642,0.));
#35569=CARTESIAN_POINT('Ctrl Pts',(-8.83391042911628,21.3083278326642,18.));
#35570=CARTESIAN_POINT('Ctrl Pts',(-8.85344872418155,21.2218358113425,0.));
#35571=CARTESIAN_POINT('Ctrl Pts',(-8.85344872418155,21.2218358113425,18.));
#35572=CARTESIAN_POINT('Ctrl Pts',(-8.87237094640748,21.1353864352374,0.));
#35573=CARTESIAN_POINT('Ctrl Pts',(-8.87237094640748,21.1353864352374,18.));
#35574=CARTESIAN_POINT('Ctrl Pts',(-8.89067412773385,21.0489832630915,0.));
#35575=CARTESIAN_POINT('Ctrl Pts',(-8.89067412773385,21.0489832630915,18.));
#35576=CARTESIAN_POINT('Ctrl Pts',(-8.90835509843284,20.9626300944902,0.));
#35577=CARTESIAN_POINT('Ctrl Pts',(-8.90835509843284,20.9626300944902,18.));
#35578=CARTESIAN_POINT('Ctrl Pts',(-8.92541048738648,20.8763310073304,0.));
#35579=CARTESIAN_POINT('Ctrl Pts',(-8.92541048738648,20.8763310073304,18.));
#35580=CARTESIAN_POINT('Ctrl Pts',(-8.94183680111377,20.7900902537083,0.));
#35581=CARTESIAN_POINT('Ctrl Pts',(-8.94183680111377,20.7900902537083,18.));
#35582=CARTESIAN_POINT('Ctrl Pts',(-8.95763049112623,20.7039121898975,0.));
#35583=CARTESIAN_POINT('Ctrl Pts',(-8.95763049112623,20.7039121898975,18.));
#35584=CARTESIAN_POINT('Ctrl Pts',(-8.97278801890467,20.6178012000199,0.));
#35585=CARTESIAN_POINT('Ctrl Pts',(-8.97278801890467,20.6178012000199,18.));
#35586=CARTESIAN_POINT('Ctrl Pts',(-8.98730595457659,20.5317616031369,0.));
#35587=CARTESIAN_POINT('Ctrl Pts',(-8.98730595457659,20.5317616031369,18.));
#35588=CARTESIAN_POINT('Ctrl Pts',(-9.00118097039516,20.4457976315472,0.));
#35589=CARTESIAN_POINT('Ctrl Pts',(-9.00118097039516,20.4457976315472,18.));
#35590=CARTESIAN_POINT('Ctrl Pts',(-9.01440965049155,20.3599135373691,0.));
#35591=CARTESIAN_POINT('Ctrl Pts',(-9.01440965049155,20.3599135373691,18.));
#35592=CARTESIAN_POINT('Ctrl Pts',(-9.02698833758324,20.2741136736186,0.));
#35593=CARTESIAN_POINT('Ctrl Pts',(-9.02698833758324,20.2741136736186,18.));
#35594=CARTESIAN_POINT('Ctrl Pts',(-9.03891298737031,20.1884025764493,0.));
#35595=CARTESIAN_POINT('Ctrl Pts',(-9.03891298737031,20.1884025764493,18.));
#35596=CARTESIAN_POINT('Ctrl Pts',(-9.0501789809071,20.1027850670435,0.));
#35597=CARTESIAN_POINT('Ctrl Pts',(-9.0501789809071,20.1027850670435,18.));
#35598=CARTESIAN_POINT('Ctrl Pts',(-9.0607810967537,20.0172662790811,0.));
#35599=CARTESIAN_POINT('Ctrl Pts',(-9.0607810967537,20.0172662790811,18.));
#35600=CARTESIAN_POINT('Ctrl Pts',(-9.0707138821585,19.9318514954605,0.));
#35601=CARTESIAN_POINT('Ctrl Pts',(-9.0707138821585,19.9318514954605,18.));
#35602=CARTESIAN_POINT('Ctrl Pts',(-9.07997196979668,19.846546013708,0.));
#35603=CARTESIAN_POINT('Ctrl Pts',(-9.07997196979668,19.846546013708,18.));
#35604=CARTESIAN_POINT('Ctrl Pts',(-9.08855038355401,19.7613550146978,0.));
#35605=CARTESIAN_POINT('Ctrl Pts',(-9.08855038355401,19.7613550146978,18.));
#35606=CARTESIAN_POINT('Ctrl Pts',(-9.0964449428387,19.6762833927168,0.));
#35607=CARTESIAN_POINT('Ctrl Pts',(-9.0964449428387,19.6762833927168,18.));
#35608=CARTESIAN_POINT('Ctrl Pts',(-9.10365235736464,19.5913357132276,0.));
#35609=CARTESIAN_POINT('Ctrl Pts',(-9.10365235736464,19.5913357132276,18.));
#35610=CARTESIAN_POINT('Ctrl Pts',(-9.11016929611335,19.5065165934577,0.));
#35611=CARTESIAN_POINT('Ctrl Pts',(-9.11016929611335,19.5065165934577,18.));
#35612=CARTESIAN_POINT('Ctrl Pts',(-9.1159915924392,19.4218310275711,0.));
#35613=CARTESIAN_POINT('Ctrl Pts',(-9.1159915924392,19.4218310275711,18.));
#35614=CARTESIAN_POINT('Ctrl Pts',(-9.12111347941199,19.3372847008483,0.));
#35615=CARTESIAN_POINT('Ctrl Pts',(-9.12111347941199,19.3372847008483,18.));
#35616=CARTESIAN_POINT('Ctrl Pts',(-9.12552662785599,19.2528843844341,0.));
#35617=CARTESIAN_POINT('Ctrl Pts',(-9.12552662785599,19.2528843844341,18.));
#35618=CARTESIAN_POINT('Ctrl Pts',(-9.12921984349375,19.1686380639041,0.));
#35619=CARTESIAN_POINT('Ctrl Pts',(-9.12921984349375,19.1686380639041,18.));
#35620=CARTESIAN_POINT('Ctrl Pts',(-9.13218114462419,19.0845541036965,0.));
#35621=CARTESIAN_POINT('Ctrl Pts',(-9.13218114462419,19.0845541036965,18.));
#35622=CARTESIAN_POINT('Ctrl Pts',(-9.13439956903533,19.0006405223697,0.));
#35623=CARTESIAN_POINT('Ctrl Pts',(-9.13439956903533,19.0006405223697,18.));
#35624=CARTESIAN_POINT('Ctrl Pts',(-9.13586688858168,18.9169043053388,0.));
#35625=CARTESIAN_POINT('Ctrl Pts',(-9.13586688858168,18.9169043053388,18.));
#35626=CARTESIAN_POINT('Ctrl Pts',(-9.13657985367153,18.8333505052874,0.));
#35627=CARTESIAN_POINT('Ctrl Pts',(-9.13657985367153,18.8333505052874,18.));
#35628=CARTESIAN_POINT('Ctrl Pts',(-9.13654074021147,18.7499820263476,0.));
#35629=CARTESIAN_POINT('Ctrl Pts',(-9.13654074021147,18.7499820263476,18.));
#35630=CARTESIAN_POINT('Ctrl Pts',(-9.13575227582418,18.6668016710749,0.));
#35631=CARTESIAN_POINT('Ctrl Pts',(-9.13575227582418,18.6668016710749,18.));
#35632=CARTESIAN_POINT('Ctrl Pts',(-9.13421321934922,18.5838139250423,0.));
#35633=CARTESIAN_POINT('Ctrl Pts',(-9.13421321934922,18.5838139250423,18.));
#35634=CARTESIAN_POINT('Ctrl Pts',(-9.13191425549883,18.5010266156389,0.));
#35635=CARTESIAN_POINT('Ctrl Pts',(-9.13191425549883,18.5010266156389,18.));
#35636=CARTESIAN_POINT('Ctrl Pts',(-9.12883240135631,18.4184531695731,0.));
#35637=CARTESIAN_POINT('Ctrl Pts',(-9.12883240135631,18.4184531695731,18.));
#35638=CARTESIAN_POINT('Ctrl Pts',(-9.12493031448671,18.3361129010289,0.));
#35639=CARTESIAN_POINT('Ctrl Pts',(-9.12493031448671,18.3361129010289,18.));
#35640=CARTESIAN_POINT('Ctrl Pts',(-9.12016808144599,18.2540262849075,0.));
#35641=CARTESIAN_POINT('Ctrl Pts',(-9.12016808144599,18.2540262849075,18.));
#35642=CARTESIAN_POINT('Ctrl Pts',(-9.11451347590539,18.1722108451637,0.));
#35643=CARTESIAN_POINT('Ctrl Pts',(-9.11451347590539,18.1722108451637,18.));
#35644=CARTESIAN_POINT('Ctrl Pts',(-9.10795114540259,18.0906774757189,0.));
#35645=CARTESIAN_POINT('Ctrl Pts',(-9.10795114540259,18.0906774757189,18.));
#35646=CARTESIAN_POINT('Ctrl Pts',(-9.10049631917583,18.0094249416472,0.));
#35647=CARTESIAN_POINT('Ctrl Pts',(-9.10049631917583,18.0094249416472,18.));
#35648=CARTESIAN_POINT('Ctrl Pts',(-9.09219303320079,17.9284406141976,0.));
#35649=CARTESIAN_POINT('Ctrl Pts',(-9.09219303320079,17.9284406141976,18.));
#35650=CARTESIAN_POINT('Ctrl Pts',(-9.08308548608349,17.8477120247758,0.));
#35651=CARTESIAN_POINT('Ctrl Pts',(-9.08308548608349,17.8477120247758,18.));
#35652=CARTESIAN_POINT('Ctrl Pts',(-9.07319314215026,17.7672369091005,0.));
#35653=CARTESIAN_POINT('Ctrl Pts',(-9.07319314215026,17.7672369091005,18.));
#35654=CARTESIAN_POINT('Ctrl Pts',(-9.06248904941394,17.6870319618808,0.));
#35655=CARTESIAN_POINT('Ctrl Pts',(-9.06248904941394,17.6870319618808,18.));
#35656=CARTESIAN_POINT('Ctrl Pts',(-9.05086524971401,17.6071467783263,0.));
#35657=CARTESIAN_POINT('Ctrl Pts',(-9.05086524971401,17.6071467783263,18.));
#35658=CARTESIAN_POINT('Ctrl Pts',(-9.03814678971601,17.5276582702181,0.));
#35659=CARTESIAN_POINT('Ctrl Pts',(-9.03814678971601,17.5276582702181,18.));
#35660=CARTESIAN_POINT('Ctrl Pts',(-9.0241575097608,17.4486443043185,0.));
#35661=CARTESIAN_POINT('Ctrl Pts',(-9.0241575097608,17.4486443043185,18.));
#35662=CARTESIAN_POINT('Ctrl Pts',(-9.00877780436036,17.3701605263553,0.));
#35663=CARTESIAN_POINT('Ctrl Pts',(-9.00877780436036,17.3701605263553,18.));
#35664=CARTESIAN_POINT('Ctrl Pts',(-8.99199362652256,17.2922207948279,0.));
#35665=CARTESIAN_POINT('Ctrl Pts',(-8.99199362652256,17.2922207948279,18.));
#35666=CARTESIAN_POINT('Ctrl Pts',(-8.97397941759265,17.2147637614528,0.));
#35667=CARTESIAN_POINT('Ctrl Pts',(-8.97397941759265,17.2147637614528,18.));
#35668=CARTESIAN_POINT('Ctrl Pts',(-8.95502702208203,17.1376822726252,0.));
#35669=CARTESIAN_POINT('Ctrl Pts',(-8.95502702208203,17.1376822726252,18.));
#35670=CARTESIAN_POINT('Ctrl Pts',(-8.93538377395243,17.0608897634975,0.));
#35671=CARTESIAN_POINT('Ctrl Pts',(-8.93538377395243,17.0608897634975,18.));
#35672=CARTESIAN_POINT('Ctrl Pts',(-8.91510993758932,16.9843788566346,0.));
#35673=CARTESIAN_POINT('Ctrl Pts',(-8.91510993758932,16.9843788566346,18.));
#35674=CARTESIAN_POINT('Ctrl Pts',(-8.89394614661328,16.908275670167,0.));
#35675=CARTESIAN_POINT('Ctrl Pts',(-8.89394614661328,16.908275670167,18.));
#35676=CARTESIAN_POINT('Ctrl Pts',(-8.87112909692392,16.8329157811062,0.));
#35677=CARTESIAN_POINT('Ctrl Pts',(-8.87112909692392,16.8329157811062,18.));
#35678=CARTESIAN_POINT('Ctrl Pts',(-8.84558256033742,16.7587634618101,0.));
#35679=CARTESIAN_POINT('Ctrl Pts',(-8.84558256033742,16.7587634618101,18.));
#35680=CARTESIAN_POINT('Ctrl Pts',(-8.82207984677446,16.7007854423938,0.));
#35681=CARTESIAN_POINT('Ctrl Pts',(-8.82207984677446,16.7007854423938,18.));
#35682=CARTESIAN_POINT('Ctrl Pts',(-8.8023348179895,16.6582257921024,0.));
#35683=CARTESIAN_POINT('Ctrl Pts',(-8.8023348179895,16.6582257921024,18.));
#35684=CARTESIAN_POINT('Ctrl Pts',(-8.78817964150686,16.6302847808193,0.));
#35685=CARTESIAN_POINT('Ctrl Pts',(-8.78817964150686,16.6302847808193,18.));
#35686=CARTESIAN_POINT('Ctrl Pts',(-8.78085409196639,16.6164222996225,0.));
#35687=CARTESIAN_POINT('Ctrl Pts',(-8.78085409196639,16.6164222996225,18.));
#35688=CARTESIAN_POINT('',(-8.52496423935279,22.4349054983023,0.));
#35689=CARTESIAN_POINT('Ctrl Pts',(-8.78085409196639,16.6164222996225,0.));
#35690=CARTESIAN_POINT('Ctrl Pts',(-8.78817964150686,16.6302847808193,0.));
#35691=CARTESIAN_POINT('Ctrl Pts',(-8.8023348179895,16.6582257921024,0.));
#35692=CARTESIAN_POINT('Ctrl Pts',(-8.82207984677446,16.7007854423938,0.));
#35693=CARTESIAN_POINT('Ctrl Pts',(-8.84558256033742,16.7587634618101,0.));
#35694=CARTESIAN_POINT('Ctrl Pts',(-8.87112909692392,16.8329157811062,0.));
#35695=CARTESIAN_POINT('Ctrl Pts',(-8.89394614661328,16.908275670167,0.));
#35696=CARTESIAN_POINT('Ctrl Pts',(-8.91510993758932,16.9843788566346,0.));
#35697=CARTESIAN_POINT('Ctrl Pts',(-8.93538377395243,17.0608897634975,0.));
#35698=CARTESIAN_POINT('Ctrl Pts',(-8.95502702208203,17.1376822726252,0.));
#35699=CARTESIAN_POINT('Ctrl Pts',(-8.97397941759265,17.2147637614528,0.));
#35700=CARTESIAN_POINT('Ctrl Pts',(-8.99199362652256,17.2922207948279,0.));
#35701=CARTESIAN_POINT('Ctrl Pts',(-9.00877780436036,17.3701605263553,0.));
#35702=CARTESIAN_POINT('Ctrl Pts',(-9.0241575097608,17.4486443043185,0.));
#35703=CARTESIAN_POINT('Ctrl Pts',(-9.03814678971601,17.5276582702181,0.));
#35704=CARTESIAN_POINT('Ctrl Pts',(-9.05086524971401,17.6071467783263,0.));
#35705=CARTESIAN_POINT('Ctrl Pts',(-9.06248904941394,17.6870319618808,0.));
#35706=CARTESIAN_POINT('Ctrl Pts',(-9.07319314215026,17.7672369091005,0.));
#35707=CARTESIAN_POINT('Ctrl Pts',(-9.08308548608349,17.8477120247758,0.));
#35708=CARTESIAN_POINT('Ctrl Pts',(-9.09219303320079,17.9284406141976,0.));
#35709=CARTESIAN_POINT('Ctrl Pts',(-9.10049631917583,18.0094249416472,0.));
#35710=CARTESIAN_POINT('Ctrl Pts',(-9.10795114540259,18.0906774757189,0.));
#35711=CARTESIAN_POINT('Ctrl Pts',(-9.11451347590539,18.1722108451637,0.));
#35712=CARTESIAN_POINT('Ctrl Pts',(-9.12016808144599,18.2540262849075,0.));
#35713=CARTESIAN_POINT('Ctrl Pts',(-9.12493031448671,18.3361129010289,0.));
#35714=CARTESIAN_POINT('Ctrl Pts',(-9.12883240135631,18.4184531695731,0.));
#35715=CARTESIAN_POINT('Ctrl Pts',(-9.13191425549883,18.5010266156389,0.));
#35716=CARTESIAN_POINT('Ctrl Pts',(-9.13421321934922,18.5838139250423,0.));
#35717=CARTESIAN_POINT('Ctrl Pts',(-9.13575227582418,18.6668016710749,0.));
#35718=CARTESIAN_POINT('Ctrl Pts',(-9.13654074021147,18.7499820263476,0.));
#35719=CARTESIAN_POINT('Ctrl Pts',(-9.13657985367153,18.8333505052874,0.));
#35720=CARTESIAN_POINT('Ctrl Pts',(-9.13586688858168,18.9169043053388,0.));
#35721=CARTESIAN_POINT('Ctrl Pts',(-9.13439956903533,19.0006405223697,0.));
#35722=CARTESIAN_POINT('Ctrl Pts',(-9.13218114462419,19.0845541036965,0.));
#35723=CARTESIAN_POINT('Ctrl Pts',(-9.12921984349375,19.1686380639041,0.));
#35724=CARTESIAN_POINT('Ctrl Pts',(-9.12552662785599,19.2528843844341,0.));
#35725=CARTESIAN_POINT('Ctrl Pts',(-9.12111347941199,19.3372847008483,0.));
#35726=CARTESIAN_POINT('Ctrl Pts',(-9.1159915924392,19.4218310275711,0.));
#35727=CARTESIAN_POINT('Ctrl Pts',(-9.11016929611335,19.5065165934577,0.));
#35728=CARTESIAN_POINT('Ctrl Pts',(-9.10365235736464,19.5913357132276,0.));
#35729=CARTESIAN_POINT('Ctrl Pts',(-9.0964449428387,19.6762833927168,0.));
#35730=CARTESIAN_POINT('Ctrl Pts',(-9.08855038355401,19.7613550146978,0.));
#35731=CARTESIAN_POINT('Ctrl Pts',(-9.07997196979668,19.846546013708,0.));
#35732=CARTESIAN_POINT('Ctrl Pts',(-9.0707138821585,19.9318514954605,0.));
#35733=CARTESIAN_POINT('Ctrl Pts',(-9.0607810967537,20.0172662790811,0.));
#35734=CARTESIAN_POINT('Ctrl Pts',(-9.0501789809071,20.1027850670435,0.));
#35735=CARTESIAN_POINT('Ctrl Pts',(-9.03891298737031,20.1884025764493,0.));
#35736=CARTESIAN_POINT('Ctrl Pts',(-9.02698833758324,20.2741136736186,0.));
#35737=CARTESIAN_POINT('Ctrl Pts',(-9.01440965049155,20.3599135373691,0.));
#35738=CARTESIAN_POINT('Ctrl Pts',(-9.00118097039516,20.4457976315472,0.));
#35739=CARTESIAN_POINT('Ctrl Pts',(-8.98730595457659,20.5317616031369,0.));
#35740=CARTESIAN_POINT('Ctrl Pts',(-8.97278801890467,20.6178012000199,0.));
#35741=CARTESIAN_POINT('Ctrl Pts',(-8.95763049112623,20.7039121898975,0.));
#35742=CARTESIAN_POINT('Ctrl Pts',(-8.94183680111377,20.7900902537083,0.));
#35743=CARTESIAN_POINT('Ctrl Pts',(-8.92541048738648,20.8763310073304,0.));
#35744=CARTESIAN_POINT('Ctrl Pts',(-8.90835509843284,20.9626300944902,0.));
#35745=CARTESIAN_POINT('Ctrl Pts',(-8.89067412773385,21.0489832630915,0.));
#35746=CARTESIAN_POINT('Ctrl Pts',(-8.87237094640748,21.1353864352374,0.));
#35747=CARTESIAN_POINT('Ctrl Pts',(-8.85344872418155,21.2218358113425,0.));
#35748=CARTESIAN_POINT('Ctrl Pts',(-8.83391042911628,21.3083278326642,0.));
#35749=CARTESIAN_POINT('Ctrl Pts',(-8.81375890120581,21.3948590173441,0.));
#35750=CARTESIAN_POINT('Ctrl Pts',(-8.79299691277858,21.481425822209,0.));
#35751=CARTESIAN_POINT('Ctrl Pts',(-8.77162723103298,21.5680245138584,0.));
#35752=CARTESIAN_POINT('Ctrl Pts',(-8.74965270266163,21.6546509866725,0.));
#35753=CARTESIAN_POINT('Ctrl Pts',(-8.72707626956921,21.7413007707864,0.));
#35754=CARTESIAN_POINT('Ctrl Pts',(-8.70390086252202,21.8279693631274,0.));
#35755=CARTESIAN_POINT('Ctrl Pts',(-8.68012932645739,21.9146524902336,0.));
#35756=CARTESIAN_POINT('Ctrl Pts',(-8.6557643376698,22.0013463859623,0.));
#35757=CARTESIAN_POINT('Ctrl Pts',(-8.63080832792612,22.0880480931906,0.));
#35758=CARTESIAN_POINT('Ctrl Pts',(-8.60015442890613,22.1920971794848,0.));
#35759=CARTESIAN_POINT('Ctrl Pts',(-8.57387555634004,22.2788106077806,0.));
#35760=CARTESIAN_POINT('Ctrl Pts',(-8.55238412336295,22.3481844703457,0.));
#35761=CARTESIAN_POINT('Ctrl Pts',(-8.53600237317212,22.400216619619,0.));
#35762=CARTESIAN_POINT('Ctrl Pts',(-8.52496423935285,22.4349054983023,0.));
#35763=CARTESIAN_POINT('',(-8.52496423935279,22.4349054983023,15.));
#35764=CARTESIAN_POINT('Ctrl Pts',(-8.52496423935285,22.4349054983023,15.));
#35765=CARTESIAN_POINT('Ctrl Pts',(-8.53048330625154,22.4175610589877,15.));
#35766=CARTESIAN_POINT('Ctrl Pts',(-8.54146295656906,22.3828725698612,15.));
#35767=CARTESIAN_POINT('Ctrl Pts',(-8.55775698160722,22.3308410047044,15.));
#35768=CARTESIAN_POINT('Ctrl Pts',(-8.57913133085326,22.2614679221214,15.));
#35769=CARTESIAN_POINT('Ctrl Pts',(-8.60526341207613,22.1747556651024,15.));
#35770=CARTESIAN_POINT('Ctrl Pts',(-8.63080832792612,22.0880480931906,15.));
#35771=CARTESIAN_POINT('Ctrl Pts',(-8.6557643376698,22.0013463859623,15.));
#35772=CARTESIAN_POINT('Ctrl Pts',(-8.68012932645739,21.9146524902336,15.));
#35773=CARTESIAN_POINT('Ctrl Pts',(-8.70390086252202,21.8279693631274,15.));
#35774=CARTESIAN_POINT('Ctrl Pts',(-8.72707626956921,21.7413007707864,15.));
#35775=CARTESIAN_POINT('Ctrl Pts',(-8.74965270266163,21.6546509866725,15.));
#35776=CARTESIAN_POINT('Ctrl Pts',(-8.77162723103298,21.5680245138584,15.));
#35777=CARTESIAN_POINT('Ctrl Pts',(-8.79299691277858,21.481425822209,15.));
#35778=CARTESIAN_POINT('Ctrl Pts',(-8.81375890120581,21.3948590173441,15.));
#35779=CARTESIAN_POINT('Ctrl Pts',(-8.83391042911628,21.3083278326642,15.));
#35780=CARTESIAN_POINT('Ctrl Pts',(-8.85344872418155,21.2218358113425,15.));
#35781=CARTESIAN_POINT('Ctrl Pts',(-8.87237094640748,21.1353864352374,15.));
#35782=CARTESIAN_POINT('Ctrl Pts',(-8.89067412773385,21.0489832630915,15.));
#35783=CARTESIAN_POINT('Ctrl Pts',(-8.90835509843284,20.9626300944902,15.));
#35784=CARTESIAN_POINT('Ctrl Pts',(-8.92541048738648,20.8763310073304,15.));
#35785=CARTESIAN_POINT('Ctrl Pts',(-8.94183680111377,20.7900902537083,15.));
#35786=CARTESIAN_POINT('Ctrl Pts',(-8.95763049112623,20.7039121898975,15.));
#35787=CARTESIAN_POINT('Ctrl Pts',(-8.97278801890467,20.6178012000199,15.));
#35788=CARTESIAN_POINT('Ctrl Pts',(-8.98730595457659,20.5317616031369,15.));
#35789=CARTESIAN_POINT('Ctrl Pts',(-9.00118097039516,20.4457976315472,15.));
#35790=CARTESIAN_POINT('Ctrl Pts',(-9.01440965049155,20.3599135373691,15.));
#35791=CARTESIAN_POINT('Ctrl Pts',(-9.02698833758324,20.2741136736186,15.));
#35792=CARTESIAN_POINT('Ctrl Pts',(-9.03891298737031,20.1884025764493,15.));
#35793=CARTESIAN_POINT('Ctrl Pts',(-9.0501789809071,20.1027850670435,15.));
#35794=CARTESIAN_POINT('Ctrl Pts',(-9.0607810967537,20.0172662790811,15.));
#35795=CARTESIAN_POINT('Ctrl Pts',(-9.0707138821585,19.9318514954605,15.));
#35796=CARTESIAN_POINT('Ctrl Pts',(-9.07997196979668,19.846546013708,15.));
#35797=CARTESIAN_POINT('Ctrl Pts',(-9.08855038355401,19.7613550146978,15.));
#35798=CARTESIAN_POINT('Ctrl Pts',(-9.0964449428387,19.6762833927168,15.));
#35799=CARTESIAN_POINT('Ctrl Pts',(-9.10365235736464,19.5913357132276,15.));
#35800=CARTESIAN_POINT('Ctrl Pts',(-9.11016929611335,19.5065165934577,15.));
#35801=CARTESIAN_POINT('Ctrl Pts',(-9.1159915924392,19.4218310275711,15.));
#35802=CARTESIAN_POINT('Ctrl Pts',(-9.12111347941199,19.3372847008483,15.));
#35803=CARTESIAN_POINT('Ctrl Pts',(-9.12552662785599,19.2528843844341,15.));
#35804=CARTESIAN_POINT('Ctrl Pts',(-9.12921984349375,19.1686380639041,15.));
#35805=CARTESIAN_POINT('Ctrl Pts',(-9.13218114462419,19.0845541036965,15.));
#35806=CARTESIAN_POINT('Ctrl Pts',(-9.13439956903533,19.0006405223697,15.));
#35807=CARTESIAN_POINT('Ctrl Pts',(-9.13586688858168,18.9169043053388,15.));
#35808=CARTESIAN_POINT('Ctrl Pts',(-9.13657985367153,18.8333505052874,15.));
#35809=CARTESIAN_POINT('Ctrl Pts',(-9.13654074021147,18.7499820263476,15.));
#35810=CARTESIAN_POINT('Ctrl Pts',(-9.13575227582418,18.6668016710749,15.));
#35811=CARTESIAN_POINT('Ctrl Pts',(-9.13421321934922,18.5838139250423,15.));
#35812=CARTESIAN_POINT('Ctrl Pts',(-9.13191425549883,18.5010266156389,15.));
#35813=CARTESIAN_POINT('Ctrl Pts',(-9.12883240135631,18.4184531695731,15.));
#35814=CARTESIAN_POINT('Ctrl Pts',(-9.12493031448671,18.3361129010289,15.));
#35815=CARTESIAN_POINT('Ctrl Pts',(-9.12016808144599,18.2540262849075,15.));
#35816=CARTESIAN_POINT('Ctrl Pts',(-9.11451347590539,18.1722108451637,15.));
#35817=CARTESIAN_POINT('Ctrl Pts',(-9.10795114540259,18.0906774757189,15.));
#35818=CARTESIAN_POINT('Ctrl Pts',(-9.10049631917583,18.0094249416472,15.));
#35819=CARTESIAN_POINT('Ctrl Pts',(-9.09219303320079,17.9284406141976,15.));
#35820=CARTESIAN_POINT('Ctrl Pts',(-9.08308548608349,17.8477120247758,15.));
#35821=CARTESIAN_POINT('Ctrl Pts',(-9.07319314215026,17.7672369091005,15.));
#35822=CARTESIAN_POINT('Ctrl Pts',(-9.06248904941394,17.6870319618808,15.));
#35823=CARTESIAN_POINT('Ctrl Pts',(-9.05086524971401,17.6071467783263,15.));
#35824=CARTESIAN_POINT('Ctrl Pts',(-9.03814678971601,17.5276582702181,15.));
#35825=CARTESIAN_POINT('Ctrl Pts',(-9.0241575097608,17.4486443043185,15.));
#35826=CARTESIAN_POINT('Ctrl Pts',(-9.00877780436036,17.3701605263553,15.));
#35827=CARTESIAN_POINT('Ctrl Pts',(-8.99199362652256,17.2922207948279,15.));
#35828=CARTESIAN_POINT('Ctrl Pts',(-8.97397941759265,17.2147637614528,15.));
#35829=CARTESIAN_POINT('Ctrl Pts',(-8.95502702208203,17.1376822726252,15.));
#35830=CARTESIAN_POINT('Ctrl Pts',(-8.93538377395243,17.0608897634975,15.));
#35831=CARTESIAN_POINT('Ctrl Pts',(-8.91510993758932,16.9843788566346,15.));
#35832=CARTESIAN_POINT('Ctrl Pts',(-8.89394614661328,16.908275670167,15.));
#35833=CARTESIAN_POINT('Ctrl Pts',(-8.87112909692392,16.8329157811062,15.));
#35834=CARTESIAN_POINT('Ctrl Pts',(-8.84558256033742,16.7587634618101,15.));
#35835=CARTESIAN_POINT('Ctrl Pts',(-8.82207984677446,16.7007854423938,15.));
#35836=CARTESIAN_POINT('Ctrl Pts',(-8.8023348179895,16.6582257921024,15.));
#35837=CARTESIAN_POINT('Ctrl Pts',(-8.78817964150686,16.6302847808193,15.));
#35838=CARTESIAN_POINT('Ctrl Pts',(-8.78085409196639,16.6164222996225,15.));
#35839=CARTESIAN_POINT('',(-8.52496423935279,22.4349054983023,0.));
#35840=CARTESIAN_POINT('Origin',(-3.56140965415431E-14,1.09833465940894E-13,
0.));
#35841=CARTESIAN_POINT('',(-6.29006564240226,23.1610680715348,0.));
#35842=CARTESIAN_POINT('Origin',(-3.56140965415431E-14,1.09833465940894E-13,
0.));
#35843=CARTESIAN_POINT('',(-6.29006564240226,23.1610680715348,15.));
#35844=CARTESIAN_POINT('Origin',(-3.56140965415431E-14,1.09833465940894E-13,
15.));
#35845=CARTESIAN_POINT('',(-6.29006564240226,23.1610680715348,0.));
#35846=CARTESIAN_POINT('Ctrl Pts',(-2.66302778805429,18.6042245638953,0.));
#35847=CARTESIAN_POINT('Ctrl Pts',(-2.66302778805429,18.6042245638953,18.));
#35848=CARTESIAN_POINT('Ctrl Pts',(-2.66524945599054,18.6197453967525,0.));
#35849=CARTESIAN_POINT('Ctrl Pts',(-2.66524945599054,18.6197453967525,18.));
#35850=CARTESIAN_POINT('Ctrl Pts',(-2.67022099202408,18.6506703537007,0.));
#35851=CARTESIAN_POINT('Ctrl Pts',(-2.67022099202408,18.6506703537007,18.));
#35852=CARTESIAN_POINT('Ctrl Pts',(-2.67926286296661,18.696707670787,0.));
#35853=CARTESIAN_POINT('Ctrl Pts',(-2.67926286296661,18.696707670787,18.));
#35854=CARTESIAN_POINT('Ctrl Pts',(-2.69432739305027,18.7574274222161,0.));
#35855=CARTESIAN_POINT('Ctrl Pts',(-2.69432739305027,18.7574274222161,18.));
#35856=CARTESIAN_POINT('Ctrl Pts',(-2.71724545050994,18.8324337861517,0.));
#35857=CARTESIAN_POINT('Ctrl Pts',(-2.71724545050994,18.8324337861517,18.));
#35858=CARTESIAN_POINT('Ctrl Pts',(-2.74308150095404,18.9068127424043,0.));
#35859=CARTESIAN_POINT('Ctrl Pts',(-2.74308150095404,18.9068127424043,18.));
#35860=CARTESIAN_POINT('Ctrl Pts',(-2.77069196504715,18.980821277801,0.));
#35861=CARTESIAN_POINT('Ctrl Pts',(-2.77069196504715,18.980821277801,18.));
#35862=CARTESIAN_POINT('Ctrl Pts',(-2.79926206958176,19.0546365637297,0.));
#35863=CARTESIAN_POINT('Ctrl Pts',(-2.79926206958176,19.0546365637297,18.));
#35864=CARTESIAN_POINT('Ctrl Pts',(-2.828507852372,19.1283090202125,0.));
#35865=CARTESIAN_POINT('Ctrl Pts',(-2.828507852372,19.1283090202125,18.));
#35866=CARTESIAN_POINT('Ctrl Pts',(-2.85848240467741,19.2018091932025,0.));
#35867=CARTESIAN_POINT('Ctrl Pts',(-2.85848240467741,19.2018091932025,18.));
#35868=CARTESIAN_POINT('Ctrl Pts',(-2.88943670541708,19.2750617358775,0.));
#35869=CARTESIAN_POINT('Ctrl Pts',(-2.88943670541708,19.2750617358775,18.));
#35870=CARTESIAN_POINT('Ctrl Pts',(-2.92166984506916,19.3479817954251,0.));
#35871=CARTESIAN_POINT('Ctrl Pts',(-2.92166984506916,19.3479817954251,18.));
#35872=CARTESIAN_POINT('Ctrl Pts',(-2.95535900926266,19.420516469599,0.));
#35873=CARTESIAN_POINT('Ctrl Pts',(-2.95535900926266,19.420516469599,18.));
#35874=CARTESIAN_POINT('Ctrl Pts',(-2.99048468792079,19.4926628032527,0.));
#35875=CARTESIAN_POINT('Ctrl Pts',(-2.99048468792079,19.4926628032527,18.));
#35876=CARTESIAN_POINT('Ctrl Pts',(-3.02691741043284,19.5644460803884,0.));
#35877=CARTESIAN_POINT('Ctrl Pts',(-3.02691741043284,19.5644460803884,18.));
#35878=CARTESIAN_POINT('Ctrl Pts',(-3.06446889170638,19.635906849522,0.));
#35879=CARTESIAN_POINT('Ctrl Pts',(-3.06446889170638,19.635906849522,18.));
#35880=CARTESIAN_POINT('Ctrl Pts',(-3.10295238390997,19.7070857227052,0.));
#35881=CARTESIAN_POINT('Ctrl Pts',(-3.10295238390997,19.7070857227052,18.));
#35882=CARTESIAN_POINT('Ctrl Pts',(-3.1422513957243,19.7780060327854,0.));
#35883=CARTESIAN_POINT('Ctrl Pts',(-3.1422513957243,19.7780060327854,18.));
#35884=CARTESIAN_POINT('Ctrl Pts',(-3.18233430962982,19.8486701154397,0.));
#35885=CARTESIAN_POINT('Ctrl Pts',(-3.18233430962982,19.8486701154397,18.));
#35886=CARTESIAN_POINT('Ctrl Pts',(-3.22321820350857,19.9190683616661,0.));
#35887=CARTESIAN_POINT('Ctrl Pts',(-3.22321820350857,19.9190683616661,18.));
#35888=CARTESIAN_POINT('Ctrl Pts',(-3.26494616363974,19.9891848794807,0.));
#35889=CARTESIAN_POINT('Ctrl Pts',(-3.26494616363974,19.9891848794807,18.));
#35890=CARTESIAN_POINT('Ctrl Pts',(-3.30756123886962,20.0590040020603,0.));
#35891=CARTESIAN_POINT('Ctrl Pts',(-3.30756123886962,20.0590040020603,18.));
#35892=CARTESIAN_POINT('Ctrl Pts',(-3.351076475782,20.1285177769596,0.));
#35893=CARTESIAN_POINT('Ctrl Pts',(-3.351076475782,20.1285177769596,18.));
#35894=CARTESIAN_POINT('Ctrl Pts',(-3.39547305068767,20.1977264147619,0.));
#35895=CARTESIAN_POINT('Ctrl Pts',(-3.39547305068767,20.1977264147619,18.));
#35896=CARTESIAN_POINT('Ctrl Pts',(-3.44071459161672,20.2666346804507,0.));
#35897=CARTESIAN_POINT('Ctrl Pts',(-3.44071459161672,20.2666346804507,18.));
#35898=CARTESIAN_POINT('Ctrl Pts',(-3.48675677306966,20.3352494700167,0.));
#35899=CARTESIAN_POINT('Ctrl Pts',(-3.48675677306966,20.3352494700167,18.));
#35900=CARTESIAN_POINT('Ctrl Pts',(-3.53355803178954,20.4035771072894,0.));
#35901=CARTESIAN_POINT('Ctrl Pts',(-3.53355803178954,20.4035771072894,18.));
#35902=CARTESIAN_POINT('Ctrl Pts',(-3.58109188218494,20.4716202388531,0.));
#35903=CARTESIAN_POINT('Ctrl Pts',(-3.58109188218494,20.4716202388531,18.));
#35904=CARTESIAN_POINT('Ctrl Pts',(-3.62934618720589,20.5393780076056,0.));
#35905=CARTESIAN_POINT('Ctrl Pts',(-3.62934618720589,20.5393780076056,18.));
#35906=CARTESIAN_POINT('Ctrl Pts',(-3.67831730617887,20.6068475141781,0.));
#35907=CARTESIAN_POINT('Ctrl Pts',(-3.67831730617887,20.6068475141781,18.));
#35908=CARTESIAN_POINT('Ctrl Pts',(-3.72800579849619,20.6740248879992,0.));
#35909=CARTESIAN_POINT('Ctrl Pts',(-3.72800579849619,20.6740248879992,18.));
#35910=CARTESIAN_POINT('Ctrl Pts',(-3.77841179839888,20.740906441832,0.));
#35911=CARTESIAN_POINT('Ctrl Pts',(-3.77841179839888,20.740906441832,18.));
#35912=CARTESIAN_POINT('Ctrl Pts',(-3.82952970701915,20.8074899980321,0.));
#35913=CARTESIAN_POINT('Ctrl Pts',(-3.82952970701915,20.8074899980321,18.));
#35914=CARTESIAN_POINT('Ctrl Pts',(-3.88134876172354,20.8737747416623,0.));
#35915=CARTESIAN_POINT('Ctrl Pts',(-3.88134876172354,20.8737747416623,18.));
#35916=CARTESIAN_POINT('Ctrl Pts',(-3.93385538070582,20.9397606289993,0.));
#35917=CARTESIAN_POINT('Ctrl Pts',(-3.93385538070582,20.9397606289993,18.));
#35918=CARTESIAN_POINT('Ctrl Pts',(-3.98703495407281,21.0054479357374,0.));
#35919=CARTESIAN_POINT('Ctrl Pts',(-3.98703495407281,21.0054479357374,18.));
#35920=CARTESIAN_POINT('Ctrl Pts',(-4.04087373166023,21.0708367812416,0.));
#35921=CARTESIAN_POINT('Ctrl Pts',(-4.04087373166023,21.0708367812416,18.));
#35922=CARTESIAN_POINT('Ctrl Pts',(-4.09536099504429,21.1359265833073,0.));
#35923=CARTESIAN_POINT('Ctrl Pts',(-4.09536099504429,21.1359265833073,18.));
#35924=CARTESIAN_POINT('Ctrl Pts',(-4.15048873695645,21.2007161321625,0.));
#35925=CARTESIAN_POINT('Ctrl Pts',(-4.15048873695645,21.2007161321625,18.));
#35926=CARTESIAN_POINT('Ctrl Pts',(-4.20625065101369,21.2652038365365,0.));
#35927=CARTESIAN_POINT('Ctrl Pts',(-4.20625065101369,21.2652038365365,18.));
#35928=CARTESIAN_POINT('Ctrl Pts',(-4.26264132842711,21.3293879189372,0.));
#35929=CARTESIAN_POINT('Ctrl Pts',(-4.26264132842711,21.3293879189372,18.));
#35930=CARTESIAN_POINT('Ctrl Pts',(-4.31965542378783,21.3932666198096,0.));
#35931=CARTESIAN_POINT('Ctrl Pts',(-4.31965542378783,21.3932666198096,18.));
#35932=CARTESIAN_POINT('Ctrl Pts',(-4.37728667813637,21.4568384368826,0.));
#35933=CARTESIAN_POINT('Ctrl Pts',(-4.37728667813637,21.4568384368826,18.));
#35934=CARTESIAN_POINT('Ctrl Pts',(-4.43552802047029,21.5201021036274,0.));
#35935=CARTESIAN_POINT('Ctrl Pts',(-4.43552802047029,21.5201021036274,18.));
#35936=CARTESIAN_POINT('Ctrl Pts',(-4.49437199472474,21.5830564890896,0.));
#35937=CARTESIAN_POINT('Ctrl Pts',(-4.49437199472474,21.5830564890896,18.));
#35938=CARTESIAN_POINT('Ctrl Pts',(-4.55381108432127,21.6457005243617,0.));
#35939=CARTESIAN_POINT('Ctrl Pts',(-4.55381108432127,21.6457005243617,18.));
#35940=CARTESIAN_POINT('Ctrl Pts',(-4.6138380475249,21.7080331252945,0.));
#35941=CARTESIAN_POINT('Ctrl Pts',(-4.6138380475249,21.7080331252945,18.));
#35942=CARTESIAN_POINT('Ctrl Pts',(-4.67444631371023,21.770053106418,0.));
#35943=CARTESIAN_POINT('Ctrl Pts',(-4.67444631371023,21.770053106418,18.));
#35944=CARTESIAN_POINT('Ctrl Pts',(-4.73562994468575,21.8317591750867,0.));
#35945=CARTESIAN_POINT('Ctrl Pts',(-4.73562994468575,21.8317591750867,18.));
#35946=CARTESIAN_POINT('Ctrl Pts',(-4.7973834230091,21.8931499593332,0.));
#35947=CARTESIAN_POINT('Ctrl Pts',(-4.7973834230091,21.8931499593332,18.));
#35948=CARTESIAN_POINT('Ctrl Pts',(-4.85970148585195,21.954224026919,0.));
#35949=CARTESIAN_POINT('Ctrl Pts',(-4.85970148585195,21.954224026919,18.));
#35950=CARTESIAN_POINT('Ctrl Pts',(-4.92257895332779,22.0149799098431,0.));
#35951=CARTESIAN_POINT('Ctrl Pts',(-4.92257895332779,22.0149799098431,18.));
#35952=CARTESIAN_POINT('Ctrl Pts',(-4.98601051193086,22.0754161299398,0.));
#35953=CARTESIAN_POINT('Ctrl Pts',(-4.98601051193086,22.0754161299398,18.));
#35954=CARTESIAN_POINT('Ctrl Pts',(-5.04999072201681,22.1355312202693,0.));
#35955=CARTESIAN_POINT('Ctrl Pts',(-5.04999072201681,22.1355312202693,18.));
#35956=CARTESIAN_POINT('Ctrl Pts',(-5.11451415224483,22.1953237422816,0.));
#35957=CARTESIAN_POINT('Ctrl Pts',(-5.11451415224483,22.1953237422816,18.));
#35958=CARTESIAN_POINT('Ctrl Pts',(-5.17957547700992,22.2547923093751,0.));
#35959=CARTESIAN_POINT('Ctrl Pts',(-5.17957547700992,22.2547923093751,18.));
#35960=CARTESIAN_POINT('Ctrl Pts',(-5.24516957209272,22.3139356039553,0.));
#35961=CARTESIAN_POINT('Ctrl Pts',(-5.24516957209272,22.3139356039553,18.));
#35962=CARTESIAN_POINT('Ctrl Pts',(-5.31129163978934,22.3727524152125,0.));
#35963=CARTESIAN_POINT('Ctrl Pts',(-5.31129163978934,22.3727524152125,18.));
#35964=CARTESIAN_POINT('Ctrl Pts',(-5.37793718711213,22.4312416086453,0.));
#35965=CARTESIAN_POINT('Ctrl Pts',(-5.37793718711213,22.4312416086453,18.));
#35966=CARTESIAN_POINT('Ctrl Pts',(-5.44510186987254,22.4894020366778,0.));
#35967=CARTESIAN_POINT('Ctrl Pts',(-5.44510186987254,22.4894020366778,18.));
#35968=CARTESIAN_POINT('Ctrl Pts',(-5.51278136258486,22.5472324623564,0.));
#35969=CARTESIAN_POINT('Ctrl Pts',(-5.51278136258486,22.5472324623564,18.));
#35970=CARTESIAN_POINT('Ctrl Pts',(-5.58097123210075,22.6047314918151,0.));
#35971=CARTESIAN_POINT('Ctrl Pts',(-5.58097123210075,22.6047314918151,18.));
#35972=CARTESIAN_POINT('Ctrl Pts',(-5.64966676217478,22.6618974767817,0.));
#35973=CARTESIAN_POINT('Ctrl Pts',(-5.64966676217478,22.6618974767817,18.));
#35974=CARTESIAN_POINT('Ctrl Pts',(-5.71886294543539,22.7187285302677,0.));
#35975=CARTESIAN_POINT('Ctrl Pts',(-5.71886294543539,22.7187285302677,18.));
#35976=CARTESIAN_POINT('Ctrl Pts',(-5.7885547640031,22.7752227318719,0.));
#35977=CARTESIAN_POINT('Ctrl Pts',(-5.7885547640031,22.7752227318719,18.));
#35978=CARTESIAN_POINT('Ctrl Pts',(-5.85873740439746,22.8313782965033,0.));
#35979=CARTESIAN_POINT('Ctrl Pts',(-5.85873740439746,22.8313782965033,18.));
#35980=CARTESIAN_POINT('Ctrl Pts',(-5.92940648776744,22.8871937503747,0.));
#35981=CARTESIAN_POINT('Ctrl Pts',(-5.92940648776744,22.8871937503747,18.));
#35982=CARTESIAN_POINT('Ctrl Pts',(-6.00055830861927,22.9426681304804,0.));
#35983=CARTESIAN_POINT('Ctrl Pts',(-6.00055830861927,22.9426681304804,18.));
#35984=CARTESIAN_POINT('Ctrl Pts',(-6.07219001169363,22.9978011048904,0.));
#35985=CARTESIAN_POINT('Ctrl Pts',(-6.07219001169363,22.9978011048904,18.));
#35986=CARTESIAN_POINT('Ctrl Pts',(-6.14429949537005,23.0525927424848,0.));
#35987=CARTESIAN_POINT('Ctrl Pts',(-6.14429949537005,23.0525927424848,18.));
#35988=CARTESIAN_POINT('Ctrl Pts',(-6.20236818200218,23.0961532179825,0.));
#35989=CARTESIAN_POINT('Ctrl Pts',(-6.20236818200218,23.0961532179825,18.));
#35990=CARTESIAN_POINT('Ctrl Pts',(-6.24613371181767,23.1286702508203,0.));
#35991=CARTESIAN_POINT('Ctrl Pts',(-6.24613371181767,23.1286702508203,18.));
#35992=CARTESIAN_POINT('Ctrl Pts',(-6.27540581784971,23.1502801515009,0.));
#35993=CARTESIAN_POINT('Ctrl Pts',(-6.27540581784971,23.1502801515009,18.));
#35994=CARTESIAN_POINT('Ctrl Pts',(-6.29006564240226,23.1610680715348,0.));
#35995=CARTESIAN_POINT('Ctrl Pts',(-6.29006564240226,23.1610680715348,18.));
#35996=CARTESIAN_POINT('Ctrl Pts',(-2.66302778805429,18.6042245638953,0.));
#35997=CARTESIAN_POINT('Ctrl Pts',(-2.66524945599054,18.6197453967525,0.));
#35998=CARTESIAN_POINT('Ctrl Pts',(-2.67022099202408,18.6506703537007,0.));
#35999=CARTESIAN_POINT('Ctrl Pts',(-2.67926286296661,18.696707670787,0.));
#36000=CARTESIAN_POINT('Ctrl Pts',(-2.69432739305027,18.7574274222161,0.));
#36001=CARTESIAN_POINT('Ctrl Pts',(-2.71724545050994,18.8324337861517,0.));
#36002=CARTESIAN_POINT('Ctrl Pts',(-2.74308150095404,18.9068127424043,0.));
#36003=CARTESIAN_POINT('Ctrl Pts',(-2.77069196504715,18.980821277801,0.));
#36004=CARTESIAN_POINT('Ctrl Pts',(-2.79926206958176,19.0546365637297,0.));
#36005=CARTESIAN_POINT('Ctrl Pts',(-2.828507852372,19.1283090202125,0.));
#36006=CARTESIAN_POINT('Ctrl Pts',(-2.85848240467741,19.2018091932025,0.));
#36007=CARTESIAN_POINT('Ctrl Pts',(-2.88943670541708,19.2750617358775,0.));
#36008=CARTESIAN_POINT('Ctrl Pts',(-2.92166984506916,19.3479817954251,0.));
#36009=CARTESIAN_POINT('Ctrl Pts',(-2.95535900926266,19.420516469599,0.));
#36010=CARTESIAN_POINT('Ctrl Pts',(-2.99048468792079,19.4926628032527,0.));
#36011=CARTESIAN_POINT('Ctrl Pts',(-3.02691741043284,19.5644460803884,0.));
#36012=CARTESIAN_POINT('Ctrl Pts',(-3.06446889170638,19.635906849522,0.));
#36013=CARTESIAN_POINT('Ctrl Pts',(-3.10295238390997,19.7070857227052,0.));
#36014=CARTESIAN_POINT('Ctrl Pts',(-3.1422513957243,19.7780060327854,0.));
#36015=CARTESIAN_POINT('Ctrl Pts',(-3.18233430962982,19.8486701154397,0.));
#36016=CARTESIAN_POINT('Ctrl Pts',(-3.22321820350857,19.9190683616661,0.));
#36017=CARTESIAN_POINT('Ctrl Pts',(-3.26494616363974,19.9891848794807,0.));
#36018=CARTESIAN_POINT('Ctrl Pts',(-3.30756123886962,20.0590040020603,0.));
#36019=CARTESIAN_POINT('Ctrl Pts',(-3.351076475782,20.1285177769596,0.));
#36020=CARTESIAN_POINT('Ctrl Pts',(-3.39547305068767,20.1977264147619,0.));
#36021=CARTESIAN_POINT('Ctrl Pts',(-3.44071459161672,20.2666346804507,0.));
#36022=CARTESIAN_POINT('Ctrl Pts',(-3.48675677306966,20.3352494700167,0.));
#36023=CARTESIAN_POINT('Ctrl Pts',(-3.53355803178954,20.4035771072894,0.));
#36024=CARTESIAN_POINT('Ctrl Pts',(-3.58109188218494,20.4716202388531,0.));
#36025=CARTESIAN_POINT('Ctrl Pts',(-3.62934618720589,20.5393780076056,0.));
#36026=CARTESIAN_POINT('Ctrl Pts',(-3.67831730617887,20.6068475141781,0.));
#36027=CARTESIAN_POINT('Ctrl Pts',(-3.72800579849619,20.6740248879992,0.));
#36028=CARTESIAN_POINT('Ctrl Pts',(-3.77841179839888,20.740906441832,0.));
#36029=CARTESIAN_POINT('Ctrl Pts',(-3.82952970701915,20.8074899980321,0.));
#36030=CARTESIAN_POINT('Ctrl Pts',(-3.88134876172354,20.8737747416623,0.));
#36031=CARTESIAN_POINT('Ctrl Pts',(-3.93385538070582,20.9397606289993,0.));
#36032=CARTESIAN_POINT('Ctrl Pts',(-3.98703495407281,21.0054479357374,0.));
#36033=CARTESIAN_POINT('Ctrl Pts',(-4.04087373166023,21.0708367812416,0.));
#36034=CARTESIAN_POINT('Ctrl Pts',(-4.09536099504429,21.1359265833073,0.));
#36035=CARTESIAN_POINT('Ctrl Pts',(-4.15048873695645,21.2007161321625,0.));
#36036=CARTESIAN_POINT('Ctrl Pts',(-4.20625065101369,21.2652038365365,0.));
#36037=CARTESIAN_POINT('Ctrl Pts',(-4.26264132842711,21.3293879189372,0.));
#36038=CARTESIAN_POINT('Ctrl Pts',(-4.31965542378783,21.3932666198096,0.));
#36039=CARTESIAN_POINT('Ctrl Pts',(-4.37728667813637,21.4568384368826,0.));
#36040=CARTESIAN_POINT('Ctrl Pts',(-4.43552802047029,21.5201021036274,0.));
#36041=CARTESIAN_POINT('Ctrl Pts',(-4.49437199472474,21.5830564890896,0.));
#36042=CARTESIAN_POINT('Ctrl Pts',(-4.55381108432127,21.6457005243617,0.));
#36043=CARTESIAN_POINT('Ctrl Pts',(-4.6138380475249,21.7080331252945,0.));
#36044=CARTESIAN_POINT('Ctrl Pts',(-4.67444631371023,21.770053106418,0.));
#36045=CARTESIAN_POINT('Ctrl Pts',(-4.73562994468575,21.8317591750867,0.));
#36046=CARTESIAN_POINT('Ctrl Pts',(-4.7973834230091,21.8931499593332,0.));
#36047=CARTESIAN_POINT('Ctrl Pts',(-4.85970148585195,21.954224026919,0.));
#36048=CARTESIAN_POINT('Ctrl Pts',(-4.92257895332779,22.0149799098431,0.));
#36049=CARTESIAN_POINT('Ctrl Pts',(-4.98601051193086,22.0754161299398,0.));
#36050=CARTESIAN_POINT('Ctrl Pts',(-5.04999072201681,22.1355312202693,0.));
#36051=CARTESIAN_POINT('Ctrl Pts',(-5.11451415224483,22.1953237422816,0.));
#36052=CARTESIAN_POINT('Ctrl Pts',(-5.17957547700992,22.2547923093751,0.));
#36053=CARTESIAN_POINT('Ctrl Pts',(-5.24516957209272,22.3139356039553,0.));
#36054=CARTESIAN_POINT('Ctrl Pts',(-5.31129163978934,22.3727524152125,0.));
#36055=CARTESIAN_POINT('Ctrl Pts',(-5.37793718711213,22.4312416086453,0.));
#36056=CARTESIAN_POINT('Ctrl Pts',(-5.44510186987254,22.4894020366778,0.));
#36057=CARTESIAN_POINT('Ctrl Pts',(-5.51278136258486,22.5472324623564,0.));
#36058=CARTESIAN_POINT('Ctrl Pts',(-5.58097123210075,22.6047314918151,0.));
#36059=CARTESIAN_POINT('Ctrl Pts',(-5.64966676217478,22.6618974767817,0.));
#36060=CARTESIAN_POINT('Ctrl Pts',(-5.71886294543539,22.7187285302677,0.));
#36061=CARTESIAN_POINT('Ctrl Pts',(-5.7885547640031,22.7752227318719,0.));
#36062=CARTESIAN_POINT('Ctrl Pts',(-5.85873740439746,22.8313782965033,0.));
#36063=CARTESIAN_POINT('Ctrl Pts',(-5.92940648776744,22.8871937503747,0.));
#36064=CARTESIAN_POINT('Ctrl Pts',(-6.00055830861927,22.9426681304804,0.));
#36065=CARTESIAN_POINT('Ctrl Pts',(-6.0865163523085,23.0088276997724,0.));
#36066=CARTESIAN_POINT('Ctrl Pts',(-6.15874528113544,23.0635340031629,0.));
#36067=CARTESIAN_POINT('Ctrl Pts',(-6.21690914895776,23.107026289589,0.));
#36068=CARTESIAN_POINT('Ctrl Pts',(-6.26074599324763,23.1394922314359,0.));
#36069=CARTESIAN_POINT('Ctrl Pts',(-6.29006564240226,23.1610680715348,0.));
#36070=CARTESIAN_POINT('Ctrl Pts',(-2.66302778805429,18.6042245638953,15.));
#36071=CARTESIAN_POINT('Ctrl Pts',(-2.66524945599054,18.6197453967525,15.));
#36072=CARTESIAN_POINT('Ctrl Pts',(-2.67022099202408,18.6506703537007,15.));
#36073=CARTESIAN_POINT('Ctrl Pts',(-2.67926286296661,18.696707670787,15.));
#36074=CARTESIAN_POINT('Ctrl Pts',(-2.69432739305027,18.7574274222161,15.));
#36075=CARTESIAN_POINT('Ctrl Pts',(-2.71724545050994,18.8324337861517,15.));
#36076=CARTESIAN_POINT('Ctrl Pts',(-2.74308150095404,18.9068127424043,15.));
#36077=CARTESIAN_POINT('Ctrl Pts',(-2.77069196504715,18.980821277801,15.));
#36078=CARTESIAN_POINT('Ctrl Pts',(-2.79926206958176,19.0546365637297,15.));
#36079=CARTESIAN_POINT('Ctrl Pts',(-2.828507852372,19.1283090202125,15.));
#36080=CARTESIAN_POINT('Ctrl Pts',(-2.85848240467741,19.2018091932025,15.));
#36081=CARTESIAN_POINT('Ctrl Pts',(-2.88943670541708,19.2750617358775,15.));
#36082=CARTESIAN_POINT('Ctrl Pts',(-2.92166984506916,19.3479817954251,15.));
#36083=CARTESIAN_POINT('Ctrl Pts',(-2.95535900926266,19.420516469599,15.));
#36084=CARTESIAN_POINT('Ctrl Pts',(-2.99048468792079,19.4926628032527,15.));
#36085=CARTESIAN_POINT('Ctrl Pts',(-3.02691741043284,19.5644460803884,15.));
#36086=CARTESIAN_POINT('Ctrl Pts',(-3.06446889170638,19.635906849522,15.));
#36087=CARTESIAN_POINT('Ctrl Pts',(-3.10295238390997,19.7070857227052,15.));
#36088=CARTESIAN_POINT('Ctrl Pts',(-3.1422513957243,19.7780060327854,15.));
#36089=CARTESIAN_POINT('Ctrl Pts',(-3.18233430962982,19.8486701154397,15.));
#36090=CARTESIAN_POINT('Ctrl Pts',(-3.22321820350857,19.9190683616661,15.));
#36091=CARTESIAN_POINT('Ctrl Pts',(-3.26494616363974,19.9891848794807,15.));
#36092=CARTESIAN_POINT('Ctrl Pts',(-3.30756123886962,20.0590040020603,15.));
#36093=CARTESIAN_POINT('Ctrl Pts',(-3.351076475782,20.1285177769596,15.));
#36094=CARTESIAN_POINT('Ctrl Pts',(-3.39547305068767,20.1977264147619,15.));
#36095=CARTESIAN_POINT('Ctrl Pts',(-3.44071459161672,20.2666346804507,15.));
#36096=CARTESIAN_POINT('Ctrl Pts',(-3.48675677306966,20.3352494700167,15.));
#36097=CARTESIAN_POINT('Ctrl Pts',(-3.53355803178954,20.4035771072894,15.));
#36098=CARTESIAN_POINT('Ctrl Pts',(-3.58109188218494,20.4716202388531,15.));
#36099=CARTESIAN_POINT('Ctrl Pts',(-3.62934618720589,20.5393780076056,15.));
#36100=CARTESIAN_POINT('Ctrl Pts',(-3.67831730617887,20.6068475141781,15.));
#36101=CARTESIAN_POINT('Ctrl Pts',(-3.72800579849619,20.6740248879992,15.));
#36102=CARTESIAN_POINT('Ctrl Pts',(-3.77841179839888,20.740906441832,15.));
#36103=CARTESIAN_POINT('Ctrl Pts',(-3.82952970701915,20.8074899980321,15.));
#36104=CARTESIAN_POINT('Ctrl Pts',(-3.88134876172354,20.8737747416623,15.));
#36105=CARTESIAN_POINT('Ctrl Pts',(-3.93385538070582,20.9397606289993,15.));
#36106=CARTESIAN_POINT('Ctrl Pts',(-3.98703495407281,21.0054479357374,15.));
#36107=CARTESIAN_POINT('Ctrl Pts',(-4.04087373166023,21.0708367812416,15.));
#36108=CARTESIAN_POINT('Ctrl Pts',(-4.09536099504429,21.1359265833073,15.));
#36109=CARTESIAN_POINT('Ctrl Pts',(-4.15048873695645,21.2007161321625,15.));
#36110=CARTESIAN_POINT('Ctrl Pts',(-4.20625065101369,21.2652038365365,15.));
#36111=CARTESIAN_POINT('Ctrl Pts',(-4.26264132842711,21.3293879189372,15.));
#36112=CARTESIAN_POINT('Ctrl Pts',(-4.31965542378783,21.3932666198096,15.));
#36113=CARTESIAN_POINT('Ctrl Pts',(-4.37728667813637,21.4568384368826,15.));
#36114=CARTESIAN_POINT('Ctrl Pts',(-4.43552802047029,21.5201021036274,15.));
#36115=CARTESIAN_POINT('Ctrl Pts',(-4.49437199472474,21.5830564890896,15.));
#36116=CARTESIAN_POINT('Ctrl Pts',(-4.55381108432127,21.6457005243617,15.));
#36117=CARTESIAN_POINT('Ctrl Pts',(-4.6138380475249,21.7080331252945,15.));
#36118=CARTESIAN_POINT('Ctrl Pts',(-4.67444631371023,21.770053106418,15.));
#36119=CARTESIAN_POINT('Ctrl Pts',(-4.73562994468575,21.8317591750867,15.));
#36120=CARTESIAN_POINT('Ctrl Pts',(-4.7973834230091,21.8931499593332,15.));
#36121=CARTESIAN_POINT('Ctrl Pts',(-4.85970148585195,21.954224026919,15.));
#36122=CARTESIAN_POINT('Ctrl Pts',(-4.92257895332779,22.0149799098431,15.));
#36123=CARTESIAN_POINT('Ctrl Pts',(-4.98601051193086,22.0754161299398,15.));
#36124=CARTESIAN_POINT('Ctrl Pts',(-5.04999072201681,22.1355312202693,15.));
#36125=CARTESIAN_POINT('Ctrl Pts',(-5.11451415224483,22.1953237422816,15.));
#36126=CARTESIAN_POINT('Ctrl Pts',(-5.17957547700992,22.2547923093751,15.));
#36127=CARTESIAN_POINT('Ctrl Pts',(-5.24516957209272,22.3139356039553,15.));
#36128=CARTESIAN_POINT('Ctrl Pts',(-5.31129163978934,22.3727524152125,15.));
#36129=CARTESIAN_POINT('Ctrl Pts',(-5.37793718711213,22.4312416086453,15.));
#36130=CARTESIAN_POINT('Ctrl Pts',(-5.44510186987254,22.4894020366778,15.));
#36131=CARTESIAN_POINT('Ctrl Pts',(-5.51278136258486,22.5472324623564,15.));
#36132=CARTESIAN_POINT('Ctrl Pts',(-5.58097123210075,22.6047314918151,15.));
#36133=CARTESIAN_POINT('Ctrl Pts',(-5.64966676217478,22.6618974767817,15.));
#36134=CARTESIAN_POINT('Ctrl Pts',(-5.71886294543539,22.7187285302677,15.));
#36135=CARTESIAN_POINT('Ctrl Pts',(-5.7885547640031,22.7752227318719,15.));
#36136=CARTESIAN_POINT('Ctrl Pts',(-5.85873740439746,22.8313782965033,15.));
#36137=CARTESIAN_POINT('Ctrl Pts',(-5.92940648776744,22.8871937503747,15.));
#36138=CARTESIAN_POINT('Ctrl Pts',(-6.00055830861927,22.9426681304804,15.));
#36139=CARTESIAN_POINT('Ctrl Pts',(-6.0865163523085,23.0088276997724,15.));
#36140=CARTESIAN_POINT('Ctrl Pts',(-6.15874528113544,23.0635340031629,15.));
#36141=CARTESIAN_POINT('Ctrl Pts',(-6.21690914895776,23.107026289589,15.));
#36142=CARTESIAN_POINT('Ctrl Pts',(-6.26074599324763,23.1394922314359,15.));
#36143=CARTESIAN_POINT('Ctrl Pts',(-6.29006564240226,23.1610680715348,15.));
#36144=CARTESIAN_POINT('Ctrl Pts',(6.29006564240227,23.1610680715348,0.));
#36145=CARTESIAN_POINT('Ctrl Pts',(6.29006564240227,23.1610680715348,18.));
#36146=CARTESIAN_POINT('Ctrl Pts',(6.27540581784972,23.1502801515009,0.));
#36147=CARTESIAN_POINT('Ctrl Pts',(6.27540581784972,23.1502801515009,18.));
#36148=CARTESIAN_POINT('Ctrl Pts',(6.24613371181767,23.1286702508203,0.));
#36149=CARTESIAN_POINT('Ctrl Pts',(6.24613371181767,23.1286702508203,18.));
#36150=CARTESIAN_POINT('Ctrl Pts',(6.20236818200219,23.0961532179825,0.));
#36151=CARTESIAN_POINT('Ctrl Pts',(6.20236818200219,23.0961532179825,18.));
#36152=CARTESIAN_POINT('Ctrl Pts',(6.14429949537005,23.0525927424848,0.));
#36153=CARTESIAN_POINT('Ctrl Pts',(6.14429949537005,23.0525927424848,18.));
#36154=CARTESIAN_POINT('Ctrl Pts',(6.07219001169363,22.9978011048904,0.));
#36155=CARTESIAN_POINT('Ctrl Pts',(6.07219001169363,22.9978011048904,18.));
#36156=CARTESIAN_POINT('Ctrl Pts',(6.00055830861927,22.9426681304804,0.));
#36157=CARTESIAN_POINT('Ctrl Pts',(6.00055830861927,22.9426681304804,18.));
#36158=CARTESIAN_POINT('Ctrl Pts',(5.92940648776744,22.8871937503747,0.));
#36159=CARTESIAN_POINT('Ctrl Pts',(5.92940648776744,22.8871937503747,18.));
#36160=CARTESIAN_POINT('Ctrl Pts',(5.85873740439747,22.8313782965033,0.));
#36161=CARTESIAN_POINT('Ctrl Pts',(5.85873740439747,22.8313782965033,18.));
#36162=CARTESIAN_POINT('Ctrl Pts',(5.78855476400311,22.7752227318719,0.));
#36163=CARTESIAN_POINT('Ctrl Pts',(5.78855476400311,22.7752227318719,18.));
#36164=CARTESIAN_POINT('Ctrl Pts',(5.71886294543539,22.7187285302677,0.));
#36165=CARTESIAN_POINT('Ctrl Pts',(5.71886294543539,22.7187285302677,18.));
#36166=CARTESIAN_POINT('Ctrl Pts',(5.64966676217478,22.6618974767817,0.));
#36167=CARTESIAN_POINT('Ctrl Pts',(5.64966676217478,22.6618974767817,18.));
#36168=CARTESIAN_POINT('Ctrl Pts',(5.58097123210075,22.6047314918151,0.));
#36169=CARTESIAN_POINT('Ctrl Pts',(5.58097123210075,22.6047314918151,18.));
#36170=CARTESIAN_POINT('Ctrl Pts',(5.51278136258486,22.5472324623564,0.));
#36171=CARTESIAN_POINT('Ctrl Pts',(5.51278136258486,22.5472324623564,18.));
#36172=CARTESIAN_POINT('Ctrl Pts',(5.44510186987254,22.4894020366778,0.));
#36173=CARTESIAN_POINT('Ctrl Pts',(5.44510186987254,22.4894020366778,18.));
#36174=CARTESIAN_POINT('Ctrl Pts',(5.37793718711213,22.4312416086453,0.));
#36175=CARTESIAN_POINT('Ctrl Pts',(5.37793718711213,22.4312416086453,18.));
#36176=CARTESIAN_POINT('Ctrl Pts',(5.31129163978934,22.3727524152125,0.));
#36177=CARTESIAN_POINT('Ctrl Pts',(5.31129163978934,22.3727524152125,18.));
#36178=CARTESIAN_POINT('Ctrl Pts',(5.24516957209272,22.3139356039553,0.));
#36179=CARTESIAN_POINT('Ctrl Pts',(5.24516957209272,22.3139356039553,18.));
#36180=CARTESIAN_POINT('Ctrl Pts',(5.17957547700992,22.2547923093751,0.));
#36181=CARTESIAN_POINT('Ctrl Pts',(5.17957547700992,22.2547923093751,18.));
#36182=CARTESIAN_POINT('Ctrl Pts',(5.11451415224484,22.1953237422816,0.));
#36183=CARTESIAN_POINT('Ctrl Pts',(5.11451415224484,22.1953237422816,18.));
#36184=CARTESIAN_POINT('Ctrl Pts',(5.04999072201681,22.1355312202693,0.));
#36185=CARTESIAN_POINT('Ctrl Pts',(5.04999072201681,22.1355312202693,18.));
#36186=CARTESIAN_POINT('Ctrl Pts',(4.98601051193086,22.0754161299398,0.));
#36187=CARTESIAN_POINT('Ctrl Pts',(4.98601051193086,22.0754161299398,18.));
#36188=CARTESIAN_POINT('Ctrl Pts',(4.92257895332779,22.0149799098431,0.));
#36189=CARTESIAN_POINT('Ctrl Pts',(4.92257895332779,22.0149799098431,18.));
#36190=CARTESIAN_POINT('Ctrl Pts',(4.85970148585195,21.954224026919,0.));
#36191=CARTESIAN_POINT('Ctrl Pts',(4.85970148585195,21.954224026919,18.));
#36192=CARTESIAN_POINT('Ctrl Pts',(4.7973834230091,21.8931499593332,0.));
#36193=CARTESIAN_POINT('Ctrl Pts',(4.7973834230091,21.8931499593332,18.));
#36194=CARTESIAN_POINT('Ctrl Pts',(4.73562994468575,21.8317591750867,0.));
#36195=CARTESIAN_POINT('Ctrl Pts',(4.73562994468575,21.8317591750867,18.));
#36196=CARTESIAN_POINT('Ctrl Pts',(4.67444631371023,21.770053106418,0.));
#36197=CARTESIAN_POINT('Ctrl Pts',(4.67444631371023,21.770053106418,18.));
#36198=CARTESIAN_POINT('Ctrl Pts',(4.6138380475249,21.7080331252945,0.));
#36199=CARTESIAN_POINT('Ctrl Pts',(4.6138380475249,21.7080331252945,18.));
#36200=CARTESIAN_POINT('Ctrl Pts',(4.55381108432127,21.6457005243617,0.));
#36201=CARTESIAN_POINT('Ctrl Pts',(4.55381108432127,21.6457005243617,18.));
#36202=CARTESIAN_POINT('Ctrl Pts',(4.49437199472474,21.5830564890896,0.));
#36203=CARTESIAN_POINT('Ctrl Pts',(4.49437199472474,21.5830564890896,18.));
#36204=CARTESIAN_POINT('Ctrl Pts',(4.43552802047029,21.5201021036274,0.));
#36205=CARTESIAN_POINT('Ctrl Pts',(4.43552802047029,21.5201021036274,18.));
#36206=CARTESIAN_POINT('Ctrl Pts',(4.37728667813637,21.4568384368826,0.));
#36207=CARTESIAN_POINT('Ctrl Pts',(4.37728667813637,21.4568384368826,18.));
#36208=CARTESIAN_POINT('Ctrl Pts',(4.31965542378783,21.3932666198096,0.));
#36209=CARTESIAN_POINT('Ctrl Pts',(4.31965542378783,21.3932666198096,18.));
#36210=CARTESIAN_POINT('Ctrl Pts',(4.26264132842711,21.3293879189372,0.));
#36211=CARTESIAN_POINT('Ctrl Pts',(4.26264132842711,21.3293879189372,18.));
#36212=CARTESIAN_POINT('Ctrl Pts',(4.20625065101369,21.2652038365365,0.));
#36213=CARTESIAN_POINT('Ctrl Pts',(4.20625065101369,21.2652038365365,18.));
#36214=CARTESIAN_POINT('Ctrl Pts',(4.15048873695645,21.2007161321625,0.));
#36215=CARTESIAN_POINT('Ctrl Pts',(4.15048873695645,21.2007161321625,18.));
#36216=CARTESIAN_POINT('Ctrl Pts',(4.09536099504429,21.1359265833073,0.));
#36217=CARTESIAN_POINT('Ctrl Pts',(4.09536099504429,21.1359265833073,18.));
#36218=CARTESIAN_POINT('Ctrl Pts',(4.04087373166023,21.0708367812416,0.));
#36219=CARTESIAN_POINT('Ctrl Pts',(4.04087373166023,21.0708367812416,18.));
#36220=CARTESIAN_POINT('Ctrl Pts',(3.98703495407281,21.0054479357374,0.));
#36221=CARTESIAN_POINT('Ctrl Pts',(3.98703495407281,21.0054479357374,18.));
#36222=CARTESIAN_POINT('Ctrl Pts',(3.93385538070582,20.9397606289993,0.));
#36223=CARTESIAN_POINT('Ctrl Pts',(3.93385538070582,20.9397606289993,18.));
#36224=CARTESIAN_POINT('Ctrl Pts',(3.88134876172354,20.8737747416623,0.));
#36225=CARTESIAN_POINT('Ctrl Pts',(3.88134876172354,20.8737747416623,18.));
#36226=CARTESIAN_POINT('Ctrl Pts',(3.82952970701916,20.8074899980321,0.));
#36227=CARTESIAN_POINT('Ctrl Pts',(3.82952970701916,20.8074899980321,18.));
#36228=CARTESIAN_POINT('Ctrl Pts',(3.77841179839888,20.740906441832,0.));
#36229=CARTESIAN_POINT('Ctrl Pts',(3.77841179839888,20.740906441832,18.));
#36230=CARTESIAN_POINT('Ctrl Pts',(3.7280057984962,20.6740248879992,0.));
#36231=CARTESIAN_POINT('Ctrl Pts',(3.7280057984962,20.6740248879992,18.));
#36232=CARTESIAN_POINT('Ctrl Pts',(3.67831730617888,20.6068475141781,0.));
#36233=CARTESIAN_POINT('Ctrl Pts',(3.67831730617888,20.6068475141781,18.));
#36234=CARTESIAN_POINT('Ctrl Pts',(3.6293461872059,20.5393780076056,0.));
#36235=CARTESIAN_POINT('Ctrl Pts',(3.6293461872059,20.5393780076056,18.));
#36236=CARTESIAN_POINT('Ctrl Pts',(3.58109188218494,20.4716202388531,0.));
#36237=CARTESIAN_POINT('Ctrl Pts',(3.58109188218494,20.4716202388531,18.));
#36238=CARTESIAN_POINT('Ctrl Pts',(3.53355803178955,20.4035771072894,0.));
#36239=CARTESIAN_POINT('Ctrl Pts',(3.53355803178955,20.4035771072894,18.));
#36240=CARTESIAN_POINT('Ctrl Pts',(3.48675677306966,20.3352494700167,0.));
#36241=CARTESIAN_POINT('Ctrl Pts',(3.48675677306966,20.3352494700167,18.));
#36242=CARTESIAN_POINT('Ctrl Pts',(3.44071459161672,20.2666346804507,0.));
#36243=CARTESIAN_POINT('Ctrl Pts',(3.44071459161672,20.2666346804507,18.));
#36244=CARTESIAN_POINT('Ctrl Pts',(3.39547305068768,20.1977264147619,0.));
#36245=CARTESIAN_POINT('Ctrl Pts',(3.39547305068768,20.1977264147619,18.));
#36246=CARTESIAN_POINT('Ctrl Pts',(3.35107647578201,20.1285177769596,0.));
#36247=CARTESIAN_POINT('Ctrl Pts',(3.35107647578201,20.1285177769596,18.));
#36248=CARTESIAN_POINT('Ctrl Pts',(3.30756123886962,20.0590040020604,0.));
#36249=CARTESIAN_POINT('Ctrl Pts',(3.30756123886962,20.0590040020604,18.));
#36250=CARTESIAN_POINT('Ctrl Pts',(3.26494616363974,19.9891848794807,0.));
#36251=CARTESIAN_POINT('Ctrl Pts',(3.26494616363974,19.9891848794807,18.));
#36252=CARTESIAN_POINT('Ctrl Pts',(3.22321820350857,19.9190683616661,0.));
#36253=CARTESIAN_POINT('Ctrl Pts',(3.22321820350857,19.9190683616661,18.));
#36254=CARTESIAN_POINT('Ctrl Pts',(3.18233430962982,19.8486701154397,0.));
#36255=CARTESIAN_POINT('Ctrl Pts',(3.18233430962982,19.8486701154397,18.));
#36256=CARTESIAN_POINT('Ctrl Pts',(3.14225139572431,19.7780060327854,0.));
#36257=CARTESIAN_POINT('Ctrl Pts',(3.14225139572431,19.7780060327854,18.));
#36258=CARTESIAN_POINT('Ctrl Pts',(3.10295238390997,19.7070857227052,0.));
#36259=CARTESIAN_POINT('Ctrl Pts',(3.10295238390997,19.7070857227052,18.));
#36260=CARTESIAN_POINT('Ctrl Pts',(3.06446889170638,19.635906849522,0.));
#36261=CARTESIAN_POINT('Ctrl Pts',(3.06446889170638,19.635906849522,18.));
#36262=CARTESIAN_POINT('Ctrl Pts',(3.02691741043284,19.5644460803884,0.));
#36263=CARTESIAN_POINT('Ctrl Pts',(3.02691741043284,19.5644460803884,18.));
#36264=CARTESIAN_POINT('Ctrl Pts',(2.99048468792079,19.4926628032527,0.));
#36265=CARTESIAN_POINT('Ctrl Pts',(2.99048468792079,19.4926628032527,18.));
#36266=CARTESIAN_POINT('Ctrl Pts',(2.95535900926266,19.420516469599,0.));
#36267=CARTESIAN_POINT('Ctrl Pts',(2.95535900926266,19.420516469599,18.));
#36268=CARTESIAN_POINT('Ctrl Pts',(2.92166984506916,19.3479817954251,0.));
#36269=CARTESIAN_POINT('Ctrl Pts',(2.92166984506916,19.3479817954251,18.));
#36270=CARTESIAN_POINT('Ctrl Pts',(2.88943670541709,19.2750617358775,0.));
#36271=CARTESIAN_POINT('Ctrl Pts',(2.88943670541709,19.2750617358775,18.));
#36272=CARTESIAN_POINT('Ctrl Pts',(2.85848240467741,19.2018091932025,0.));
#36273=CARTESIAN_POINT('Ctrl Pts',(2.85848240467741,19.2018091932025,18.));
#36274=CARTESIAN_POINT('Ctrl Pts',(2.828507852372,19.1283090202125,0.));
#36275=CARTESIAN_POINT('Ctrl Pts',(2.828507852372,19.1283090202125,18.));
#36276=CARTESIAN_POINT('Ctrl Pts',(2.79926206958176,19.0546365637297,0.));
#36277=CARTESIAN_POINT('Ctrl Pts',(2.79926206958176,19.0546365637297,18.));
#36278=CARTESIAN_POINT('Ctrl Pts',(2.77069196504715,18.980821277801,0.));
#36279=CARTESIAN_POINT('Ctrl Pts',(2.77069196504715,18.980821277801,18.));
#36280=CARTESIAN_POINT('Ctrl Pts',(2.74308150095405,18.9068127424043,0.));
#36281=CARTESIAN_POINT('Ctrl Pts',(2.74308150095405,18.9068127424043,18.));
#36282=CARTESIAN_POINT('Ctrl Pts',(2.71724545050995,18.8324337861517,0.));
#36283=CARTESIAN_POINT('Ctrl Pts',(2.71724545050995,18.8324337861517,18.));
#36284=CARTESIAN_POINT('Ctrl Pts',(2.69432739305028,18.7574274222161,0.));
#36285=CARTESIAN_POINT('Ctrl Pts',(2.69432739305028,18.7574274222161,18.));
#36286=CARTESIAN_POINT('Ctrl Pts',(2.67926286296661,18.696707670787,0.));
#36287=CARTESIAN_POINT('Ctrl Pts',(2.67926286296661,18.696707670787,18.));
#36288=CARTESIAN_POINT('Ctrl Pts',(2.67022099202409,18.6506703537007,0.));
#36289=CARTESIAN_POINT('Ctrl Pts',(2.67022099202409,18.6506703537007,18.));
#36290=CARTESIAN_POINT('Ctrl Pts',(2.66524945599055,18.6197453967525,0.));
#36291=CARTESIAN_POINT('Ctrl Pts',(2.66524945599055,18.6197453967525,18.));
#36292=CARTESIAN_POINT('Ctrl Pts',(2.66302778805429,18.6042245638953,0.));
#36293=CARTESIAN_POINT('Ctrl Pts',(2.66302778805429,18.6042245638953,18.));
#36294=CARTESIAN_POINT('',(6.29006564240232,23.1610680715348,0.));
#36295=CARTESIAN_POINT('Ctrl Pts',(2.66302778805429,18.6042245638953,0.));
#36296=CARTESIAN_POINT('Ctrl Pts',(2.66524945599055,18.6197453967525,0.));
#36297=CARTESIAN_POINT('Ctrl Pts',(2.67022099202409,18.6506703537007,0.));
#36298=CARTESIAN_POINT('Ctrl Pts',(2.67926286296661,18.696707670787,0.));
#36299=CARTESIAN_POINT('Ctrl Pts',(2.69432739305028,18.7574274222161,0.));
#36300=CARTESIAN_POINT('Ctrl Pts',(2.71724545050995,18.8324337861517,0.));
#36301=CARTESIAN_POINT('Ctrl Pts',(2.74308150095405,18.9068127424043,0.));
#36302=CARTESIAN_POINT('Ctrl Pts',(2.77069196504715,18.980821277801,0.));
#36303=CARTESIAN_POINT('Ctrl Pts',(2.79926206958176,19.0546365637297,0.));
#36304=CARTESIAN_POINT('Ctrl Pts',(2.828507852372,19.1283090202125,0.));
#36305=CARTESIAN_POINT('Ctrl Pts',(2.85848240467741,19.2018091932025,0.));
#36306=CARTESIAN_POINT('Ctrl Pts',(2.88943670541709,19.2750617358775,0.));
#36307=CARTESIAN_POINT('Ctrl Pts',(2.92166984506916,19.3479817954251,0.));
#36308=CARTESIAN_POINT('Ctrl Pts',(2.95535900926266,19.420516469599,0.));
#36309=CARTESIAN_POINT('Ctrl Pts',(2.99048468792079,19.4926628032527,0.));
#36310=CARTESIAN_POINT('Ctrl Pts',(3.02691741043284,19.5644460803884,0.));
#36311=CARTESIAN_POINT('Ctrl Pts',(3.06446889170638,19.635906849522,0.));
#36312=CARTESIAN_POINT('Ctrl Pts',(3.10295238390997,19.7070857227052,0.));
#36313=CARTESIAN_POINT('Ctrl Pts',(3.14225139572431,19.7780060327854,0.));
#36314=CARTESIAN_POINT('Ctrl Pts',(3.18233430962982,19.8486701154397,0.));
#36315=CARTESIAN_POINT('Ctrl Pts',(3.22321820350857,19.9190683616661,0.));
#36316=CARTESIAN_POINT('Ctrl Pts',(3.26494616363974,19.9891848794807,0.));
#36317=CARTESIAN_POINT('Ctrl Pts',(3.30756123886962,20.0590040020604,0.));
#36318=CARTESIAN_POINT('Ctrl Pts',(3.35107647578201,20.1285177769596,0.));
#36319=CARTESIAN_POINT('Ctrl Pts',(3.39547305068768,20.1977264147619,0.));
#36320=CARTESIAN_POINT('Ctrl Pts',(3.44071459161672,20.2666346804507,0.));
#36321=CARTESIAN_POINT('Ctrl Pts',(3.48675677306966,20.3352494700167,0.));
#36322=CARTESIAN_POINT('Ctrl Pts',(3.53355803178955,20.4035771072894,0.));
#36323=CARTESIAN_POINT('Ctrl Pts',(3.58109188218494,20.4716202388531,0.));
#36324=CARTESIAN_POINT('Ctrl Pts',(3.6293461872059,20.5393780076056,0.));
#36325=CARTESIAN_POINT('Ctrl Pts',(3.67831730617888,20.6068475141781,0.));
#36326=CARTESIAN_POINT('Ctrl Pts',(3.7280057984962,20.6740248879992,0.));
#36327=CARTESIAN_POINT('Ctrl Pts',(3.77841179839888,20.740906441832,0.));
#36328=CARTESIAN_POINT('Ctrl Pts',(3.82952970701916,20.8074899980321,0.));
#36329=CARTESIAN_POINT('Ctrl Pts',(3.88134876172354,20.8737747416623,0.));
#36330=CARTESIAN_POINT('Ctrl Pts',(3.93385538070582,20.9397606289993,0.));
#36331=CARTESIAN_POINT('Ctrl Pts',(3.98703495407281,21.0054479357374,0.));
#36332=CARTESIAN_POINT('Ctrl Pts',(4.04087373166023,21.0708367812416,0.));
#36333=CARTESIAN_POINT('Ctrl Pts',(4.09536099504429,21.1359265833073,0.));
#36334=CARTESIAN_POINT('Ctrl Pts',(4.15048873695645,21.2007161321625,0.));
#36335=CARTESIAN_POINT('Ctrl Pts',(4.20625065101369,21.2652038365365,0.));
#36336=CARTESIAN_POINT('Ctrl Pts',(4.26264132842711,21.3293879189372,0.));
#36337=CARTESIAN_POINT('Ctrl Pts',(4.31965542378783,21.3932666198096,0.));
#36338=CARTESIAN_POINT('Ctrl Pts',(4.37728667813637,21.4568384368826,0.));
#36339=CARTESIAN_POINT('Ctrl Pts',(4.43552802047029,21.5201021036274,0.));
#36340=CARTESIAN_POINT('Ctrl Pts',(4.49437199472474,21.5830564890896,0.));
#36341=CARTESIAN_POINT('Ctrl Pts',(4.55381108432127,21.6457005243617,0.));
#36342=CARTESIAN_POINT('Ctrl Pts',(4.6138380475249,21.7080331252945,0.));
#36343=CARTESIAN_POINT('Ctrl Pts',(4.67444631371023,21.770053106418,0.));
#36344=CARTESIAN_POINT('Ctrl Pts',(4.73562994468575,21.8317591750867,0.));
#36345=CARTESIAN_POINT('Ctrl Pts',(4.7973834230091,21.8931499593332,0.));
#36346=CARTESIAN_POINT('Ctrl Pts',(4.85970148585195,21.954224026919,0.));
#36347=CARTESIAN_POINT('Ctrl Pts',(4.92257895332779,22.0149799098431,0.));
#36348=CARTESIAN_POINT('Ctrl Pts',(4.98601051193086,22.0754161299398,0.));
#36349=CARTESIAN_POINT('Ctrl Pts',(5.04999072201681,22.1355312202693,0.));
#36350=CARTESIAN_POINT('Ctrl Pts',(5.11451415224484,22.1953237422816,0.));
#36351=CARTESIAN_POINT('Ctrl Pts',(5.17957547700992,22.2547923093751,0.));
#36352=CARTESIAN_POINT('Ctrl Pts',(5.24516957209272,22.3139356039553,0.));
#36353=CARTESIAN_POINT('Ctrl Pts',(5.31129163978934,22.3727524152125,0.));
#36354=CARTESIAN_POINT('Ctrl Pts',(5.37793718711213,22.4312416086453,0.));
#36355=CARTESIAN_POINT('Ctrl Pts',(5.44510186987254,22.4894020366778,0.));
#36356=CARTESIAN_POINT('Ctrl Pts',(5.51278136258486,22.5472324623564,0.));
#36357=CARTESIAN_POINT('Ctrl Pts',(5.58097123210075,22.6047314918151,0.));
#36358=CARTESIAN_POINT('Ctrl Pts',(5.64966676217478,22.6618974767817,0.));
#36359=CARTESIAN_POINT('Ctrl Pts',(5.71886294543539,22.7187285302677,0.));
#36360=CARTESIAN_POINT('Ctrl Pts',(5.78855476400311,22.7752227318719,0.));
#36361=CARTESIAN_POINT('Ctrl Pts',(5.85873740439747,22.8313782965033,0.));
#36362=CARTESIAN_POINT('Ctrl Pts',(5.92940648776744,22.8871937503747,0.));
#36363=CARTESIAN_POINT('Ctrl Pts',(6.00055830861927,22.9426681304804,0.));
#36364=CARTESIAN_POINT('Ctrl Pts',(6.0865163523085,23.0088276997724,0.));
#36365=CARTESIAN_POINT('Ctrl Pts',(6.15874528113544,23.0635340031629,0.));
#36366=CARTESIAN_POINT('Ctrl Pts',(6.21690914895778,23.107026289589,0.));
#36367=CARTESIAN_POINT('Ctrl Pts',(6.26074599324762,23.1394922314359,0.));
#36368=CARTESIAN_POINT('Ctrl Pts',(6.29006564240227,23.1610680715348,0.));
#36369=CARTESIAN_POINT('',(6.29006564240232,23.1610680715348,15.));
#36370=CARTESIAN_POINT('Ctrl Pts',(6.29006564240227,23.1610680715348,15.));
#36371=CARTESIAN_POINT('Ctrl Pts',(6.27540581784972,23.1502801515009,15.));
#36372=CARTESIAN_POINT('Ctrl Pts',(6.24613371181767,23.1286702508203,15.));
#36373=CARTESIAN_POINT('Ctrl Pts',(6.20236818200219,23.0961532179825,15.));
#36374=CARTESIAN_POINT('Ctrl Pts',(6.14429949537005,23.0525927424848,15.));
#36375=CARTESIAN_POINT('Ctrl Pts',(6.07219001169363,22.9978011048904,15.));
#36376=CARTESIAN_POINT('Ctrl Pts',(6.00055830861927,22.9426681304804,15.));
#36377=CARTESIAN_POINT('Ctrl Pts',(5.92940648776744,22.8871937503747,15.));
#36378=CARTESIAN_POINT('Ctrl Pts',(5.85873740439747,22.8313782965033,15.));
#36379=CARTESIAN_POINT('Ctrl Pts',(5.78855476400311,22.7752227318719,15.));
#36380=CARTESIAN_POINT('Ctrl Pts',(5.71886294543539,22.7187285302677,15.));
#36381=CARTESIAN_POINT('Ctrl Pts',(5.64966676217478,22.6618974767817,15.));
#36382=CARTESIAN_POINT('Ctrl Pts',(5.58097123210075,22.6047314918151,15.));
#36383=CARTESIAN_POINT('Ctrl Pts',(5.51278136258486,22.5472324623564,15.));
#36384=CARTESIAN_POINT('Ctrl Pts',(5.44510186987254,22.4894020366778,15.));
#36385=CARTESIAN_POINT('Ctrl Pts',(5.37793718711213,22.4312416086453,15.));
#36386=CARTESIAN_POINT('Ctrl Pts',(5.31129163978934,22.3727524152125,15.));
#36387=CARTESIAN_POINT('Ctrl Pts',(5.24516957209272,22.3139356039553,15.));
#36388=CARTESIAN_POINT('Ctrl Pts',(5.17957547700992,22.2547923093751,15.));
#36389=CARTESIAN_POINT('Ctrl Pts',(5.11451415224484,22.1953237422816,15.));
#36390=CARTESIAN_POINT('Ctrl Pts',(5.04999072201681,22.1355312202693,15.));
#36391=CARTESIAN_POINT('Ctrl Pts',(4.98601051193086,22.0754161299398,15.));
#36392=CARTESIAN_POINT('Ctrl Pts',(4.92257895332779,22.0149799098431,15.));
#36393=CARTESIAN_POINT('Ctrl Pts',(4.85970148585195,21.954224026919,15.));
#36394=CARTESIAN_POINT('Ctrl Pts',(4.7973834230091,21.8931499593332,15.));
#36395=CARTESIAN_POINT('Ctrl Pts',(4.73562994468575,21.8317591750867,15.));
#36396=CARTESIAN_POINT('Ctrl Pts',(4.67444631371023,21.770053106418,15.));
#36397=CARTESIAN_POINT('Ctrl Pts',(4.6138380475249,21.7080331252945,15.));
#36398=CARTESIAN_POINT('Ctrl Pts',(4.55381108432127,21.6457005243617,15.));
#36399=CARTESIAN_POINT('Ctrl Pts',(4.49437199472474,21.5830564890896,15.));
#36400=CARTESIAN_POINT('Ctrl Pts',(4.43552802047029,21.5201021036274,15.));
#36401=CARTESIAN_POINT('Ctrl Pts',(4.37728667813637,21.4568384368826,15.));
#36402=CARTESIAN_POINT('Ctrl Pts',(4.31965542378783,21.3932666198096,15.));
#36403=CARTESIAN_POINT('Ctrl Pts',(4.26264132842711,21.3293879189372,15.));
#36404=CARTESIAN_POINT('Ctrl Pts',(4.20625065101369,21.2652038365365,15.));
#36405=CARTESIAN_POINT('Ctrl Pts',(4.15048873695645,21.2007161321625,15.));
#36406=CARTESIAN_POINT('Ctrl Pts',(4.09536099504429,21.1359265833073,15.));
#36407=CARTESIAN_POINT('Ctrl Pts',(4.04087373166023,21.0708367812416,15.));
#36408=CARTESIAN_POINT('Ctrl Pts',(3.98703495407281,21.0054479357374,15.));
#36409=CARTESIAN_POINT('Ctrl Pts',(3.93385538070582,20.9397606289993,15.));
#36410=CARTESIAN_POINT('Ctrl Pts',(3.88134876172354,20.8737747416623,15.));
#36411=CARTESIAN_POINT('Ctrl Pts',(3.82952970701916,20.8074899980321,15.));
#36412=CARTESIAN_POINT('Ctrl Pts',(3.77841179839888,20.740906441832,15.));
#36413=CARTESIAN_POINT('Ctrl Pts',(3.7280057984962,20.6740248879992,15.));
#36414=CARTESIAN_POINT('Ctrl Pts',(3.67831730617888,20.6068475141781,15.));
#36415=CARTESIAN_POINT('Ctrl Pts',(3.6293461872059,20.5393780076056,15.));
#36416=CARTESIAN_POINT('Ctrl Pts',(3.58109188218494,20.4716202388531,15.));
#36417=CARTESIAN_POINT('Ctrl Pts',(3.53355803178955,20.4035771072894,15.));
#36418=CARTESIAN_POINT('Ctrl Pts',(3.48675677306966,20.3352494700167,15.));
#36419=CARTESIAN_POINT('Ctrl Pts',(3.44071459161672,20.2666346804507,15.));
#36420=CARTESIAN_POINT('Ctrl Pts',(3.39547305068768,20.1977264147619,15.));
#36421=CARTESIAN_POINT('Ctrl Pts',(3.35107647578201,20.1285177769596,15.));
#36422=CARTESIAN_POINT('Ctrl Pts',(3.30756123886962,20.0590040020604,15.));
#36423=CARTESIAN_POINT('Ctrl Pts',(3.26494616363974,19.9891848794807,15.));
#36424=CARTESIAN_POINT('Ctrl Pts',(3.22321820350857,19.9190683616661,15.));
#36425=CARTESIAN_POINT('Ctrl Pts',(3.18233430962982,19.8486701154397,15.));
#36426=CARTESIAN_POINT('Ctrl Pts',(3.14225139572431,19.7780060327854,15.));
#36427=CARTESIAN_POINT('Ctrl Pts',(3.10295238390997,19.7070857227052,15.));
#36428=CARTESIAN_POINT('Ctrl Pts',(3.06446889170638,19.635906849522,15.));
#36429=CARTESIAN_POINT('Ctrl Pts',(3.02691741043284,19.5644460803884,15.));
#36430=CARTESIAN_POINT('Ctrl Pts',(2.99048468792079,19.4926628032527,15.));
#36431=CARTESIAN_POINT('Ctrl Pts',(2.95535900926266,19.420516469599,15.));
#36432=CARTESIAN_POINT('Ctrl Pts',(2.92166984506916,19.3479817954251,15.));
#36433=CARTESIAN_POINT('Ctrl Pts',(2.88943670541709,19.2750617358775,15.));
#36434=CARTESIAN_POINT('Ctrl Pts',(2.85848240467741,19.2018091932025,15.));
#36435=CARTESIAN_POINT('Ctrl Pts',(2.828507852372,19.1283090202125,15.));
#36436=CARTESIAN_POINT('Ctrl Pts',(2.79926206958176,19.0546365637297,15.));
#36437=CARTESIAN_POINT('Ctrl Pts',(2.77069196504715,18.980821277801,15.));
#36438=CARTESIAN_POINT('Ctrl Pts',(2.74308150095405,18.9068127424043,15.));
#36439=CARTESIAN_POINT('Ctrl Pts',(2.71724545050995,18.8324337861517,15.));
#36440=CARTESIAN_POINT('Ctrl Pts',(2.69432739305028,18.7574274222161,15.));
#36441=CARTESIAN_POINT('Ctrl Pts',(2.67926286296661,18.696707670787,15.));
#36442=CARTESIAN_POINT('Ctrl Pts',(2.67022099202409,18.6506703537007,15.));
#36443=CARTESIAN_POINT('Ctrl Pts',(2.66524945599055,18.6197453967525,15.));
#36444=CARTESIAN_POINT('Ctrl Pts',(2.66302778805429,18.6042245638953,15.));
#36445=CARTESIAN_POINT('',(6.29006564240232,23.1610680715348,0.));
#36446=CARTESIAN_POINT('Origin',(3.57460821468069E-14,1.09790581218125E-13,
0.));
#36447=CARTESIAN_POINT('',(8.52496423935284,22.4349054983023,0.));
#36448=CARTESIAN_POINT('Origin',(3.57460821468069E-14,1.09790581218125E-13,
0.));
#36449=CARTESIAN_POINT('',(8.52496423935284,22.4349054983023,15.));
#36450=CARTESIAN_POINT('Origin',(3.57460821468069E-14,1.09790581218125E-13,
15.));
#36451=CARTESIAN_POINT('',(8.52496423935284,22.4349054983023,0.));
#36452=CARTESIAN_POINT('Ctrl Pts',(8.78085409196639,16.6164222996225,0.));
#36453=CARTESIAN_POINT('Ctrl Pts',(8.78085409196639,16.6164222996225,18.));
#36454=CARTESIAN_POINT('Ctrl Pts',(8.78817964150686,16.6302847808193,0.));
#36455=CARTESIAN_POINT('Ctrl Pts',(8.78817964150686,16.6302847808193,18.));
#36456=CARTESIAN_POINT('Ctrl Pts',(8.80233481798951,16.6582257921024,0.));
#36457=CARTESIAN_POINT('Ctrl Pts',(8.80233481798951,16.6582257921024,18.));
#36458=CARTESIAN_POINT('Ctrl Pts',(8.82207984677447,16.7007854423938,0.));
#36459=CARTESIAN_POINT('Ctrl Pts',(8.82207984677447,16.7007854423938,18.));
#36460=CARTESIAN_POINT('Ctrl Pts',(8.84558256033742,16.7587634618101,0.));
#36461=CARTESIAN_POINT('Ctrl Pts',(8.84558256033742,16.7587634618101,18.));
#36462=CARTESIAN_POINT('Ctrl Pts',(8.87112909692392,16.8329157811062,0.));
#36463=CARTESIAN_POINT('Ctrl Pts',(8.87112909692392,16.8329157811062,18.));
#36464=CARTESIAN_POINT('Ctrl Pts',(8.89394614661328,16.908275670167,0.));
#36465=CARTESIAN_POINT('Ctrl Pts',(8.89394614661328,16.908275670167,18.));
#36466=CARTESIAN_POINT('Ctrl Pts',(8.91510993758932,16.9843788566346,0.));
#36467=CARTESIAN_POINT('Ctrl Pts',(8.91510993758932,16.9843788566346,18.));
#36468=CARTESIAN_POINT('Ctrl Pts',(8.93538377395243,17.0608897634975,0.));
#36469=CARTESIAN_POINT('Ctrl Pts',(8.93538377395243,17.0608897634975,18.));
#36470=CARTESIAN_POINT('Ctrl Pts',(8.95502702208203,17.1376822726252,0.));
#36471=CARTESIAN_POINT('Ctrl Pts',(8.95502702208203,17.1376822726252,18.));
#36472=CARTESIAN_POINT('Ctrl Pts',(8.97397941759265,17.2147637614528,0.));
#36473=CARTESIAN_POINT('Ctrl Pts',(8.97397941759265,17.2147637614528,18.));
#36474=CARTESIAN_POINT('Ctrl Pts',(8.99199362652257,17.2922207948279,0.));
#36475=CARTESIAN_POINT('Ctrl Pts',(8.99199362652257,17.2922207948279,18.));
#36476=CARTESIAN_POINT('Ctrl Pts',(9.00877780436037,17.3701605263553,0.));
#36477=CARTESIAN_POINT('Ctrl Pts',(9.00877780436037,17.3701605263553,18.));
#36478=CARTESIAN_POINT('Ctrl Pts',(9.0241575097608,17.4486443043185,0.));
#36479=CARTESIAN_POINT('Ctrl Pts',(9.0241575097608,17.4486443043185,18.));
#36480=CARTESIAN_POINT('Ctrl Pts',(9.03814678971601,17.5276582702181,0.));
#36481=CARTESIAN_POINT('Ctrl Pts',(9.03814678971601,17.5276582702181,18.));
#36482=CARTESIAN_POINT('Ctrl Pts',(9.05086524971401,17.6071467783263,0.));
#36483=CARTESIAN_POINT('Ctrl Pts',(9.05086524971401,17.6071467783263,18.));
#36484=CARTESIAN_POINT('Ctrl Pts',(9.06248904941395,17.6870319618808,0.));
#36485=CARTESIAN_POINT('Ctrl Pts',(9.06248904941395,17.6870319618808,18.));
#36486=CARTESIAN_POINT('Ctrl Pts',(9.07319314215026,17.7672369091005,0.));
#36487=CARTESIAN_POINT('Ctrl Pts',(9.07319314215026,17.7672369091005,18.));
#36488=CARTESIAN_POINT('Ctrl Pts',(9.08308548608349,17.8477120247758,0.));
#36489=CARTESIAN_POINT('Ctrl Pts',(9.08308548608349,17.8477120247758,18.));
#36490=CARTESIAN_POINT('Ctrl Pts',(9.09219303320079,17.9284406141976,0.));
#36491=CARTESIAN_POINT('Ctrl Pts',(9.09219303320079,17.9284406141976,18.));
#36492=CARTESIAN_POINT('Ctrl Pts',(9.10049631917583,18.0094249416472,0.));
#36493=CARTESIAN_POINT('Ctrl Pts',(9.10049631917583,18.0094249416472,18.));
#36494=CARTESIAN_POINT('Ctrl Pts',(9.10795114540259,18.0906774757189,0.));
#36495=CARTESIAN_POINT('Ctrl Pts',(9.10795114540259,18.0906774757189,18.));
#36496=CARTESIAN_POINT('Ctrl Pts',(9.11451347590539,18.1722108451637,0.));
#36497=CARTESIAN_POINT('Ctrl Pts',(9.11451347590539,18.1722108451637,18.));
#36498=CARTESIAN_POINT('Ctrl Pts',(9.12016808144599,18.2540262849075,0.));
#36499=CARTESIAN_POINT('Ctrl Pts',(9.12016808144599,18.2540262849075,18.));
#36500=CARTESIAN_POINT('Ctrl Pts',(9.12493031448671,18.3361129010289,0.));
#36501=CARTESIAN_POINT('Ctrl Pts',(9.12493031448671,18.3361129010289,18.));
#36502=CARTESIAN_POINT('Ctrl Pts',(9.12883240135631,18.4184531695731,0.));
#36503=CARTESIAN_POINT('Ctrl Pts',(9.12883240135631,18.4184531695731,18.));
#36504=CARTESIAN_POINT('Ctrl Pts',(9.13191425549883,18.5010266156389,0.));
#36505=CARTESIAN_POINT('Ctrl Pts',(9.13191425549883,18.5010266156389,18.));
#36506=CARTESIAN_POINT('Ctrl Pts',(9.13421321934922,18.5838139250423,0.));
#36507=CARTESIAN_POINT('Ctrl Pts',(9.13421321934922,18.5838139250423,18.));
#36508=CARTESIAN_POINT('Ctrl Pts',(9.13575227582418,18.6668016710749,0.));
#36509=CARTESIAN_POINT('Ctrl Pts',(9.13575227582418,18.6668016710749,18.));
#36510=CARTESIAN_POINT('Ctrl Pts',(9.13654074021147,18.7499820263476,0.));
#36511=CARTESIAN_POINT('Ctrl Pts',(9.13654074021147,18.7499820263476,18.));
#36512=CARTESIAN_POINT('Ctrl Pts',(9.13657985367154,18.8333505052874,0.));
#36513=CARTESIAN_POINT('Ctrl Pts',(9.13657985367154,18.8333505052874,18.));
#36514=CARTESIAN_POINT('Ctrl Pts',(9.13586688858169,18.9169043053388,0.));
#36515=CARTESIAN_POINT('Ctrl Pts',(9.13586688858169,18.9169043053388,18.));
#36516=CARTESIAN_POINT('Ctrl Pts',(9.13439956903533,19.0006405223697,0.));
#36517=CARTESIAN_POINT('Ctrl Pts',(9.13439956903533,19.0006405223697,18.));
#36518=CARTESIAN_POINT('Ctrl Pts',(9.13218114462419,19.0845541036965,0.));
#36519=CARTESIAN_POINT('Ctrl Pts',(9.13218114462419,19.0845541036965,18.));
#36520=CARTESIAN_POINT('Ctrl Pts',(9.12921984349375,19.1686380639041,0.));
#36521=CARTESIAN_POINT('Ctrl Pts',(9.12921984349375,19.1686380639041,18.));
#36522=CARTESIAN_POINT('Ctrl Pts',(9.125526627856,19.2528843844341,0.));
#36523=CARTESIAN_POINT('Ctrl Pts',(9.125526627856,19.2528843844341,18.));
#36524=CARTESIAN_POINT('Ctrl Pts',(9.121113479412,19.3372847008483,0.));
#36525=CARTESIAN_POINT('Ctrl Pts',(9.121113479412,19.3372847008483,18.));
#36526=CARTESIAN_POINT('Ctrl Pts',(9.1159915924392,19.4218310275711,0.));
#36527=CARTESIAN_POINT('Ctrl Pts',(9.1159915924392,19.4218310275711,18.));
#36528=CARTESIAN_POINT('Ctrl Pts',(9.11016929611336,19.5065165934577,0.));
#36529=CARTESIAN_POINT('Ctrl Pts',(9.11016929611336,19.5065165934577,18.));
#36530=CARTESIAN_POINT('Ctrl Pts',(9.10365235736465,19.5913357132276,0.));
#36531=CARTESIAN_POINT('Ctrl Pts',(9.10365235736465,19.5913357132276,18.));
#36532=CARTESIAN_POINT('Ctrl Pts',(9.0964449428387,19.6762833927168,0.));
#36533=CARTESIAN_POINT('Ctrl Pts',(9.0964449428387,19.6762833927168,18.));
#36534=CARTESIAN_POINT('Ctrl Pts',(9.08855038355402,19.7613550146978,0.));
#36535=CARTESIAN_POINT('Ctrl Pts',(9.08855038355402,19.7613550146978,18.));
#36536=CARTESIAN_POINT('Ctrl Pts',(9.07997196979668,19.846546013708,0.));
#36537=CARTESIAN_POINT('Ctrl Pts',(9.07997196979668,19.846546013708,18.));
#36538=CARTESIAN_POINT('Ctrl Pts',(9.0707138821585,19.9318514954605,0.));
#36539=CARTESIAN_POINT('Ctrl Pts',(9.0707138821585,19.9318514954605,18.));
#36540=CARTESIAN_POINT('Ctrl Pts',(9.0607810967537,20.0172662790811,0.));
#36541=CARTESIAN_POINT('Ctrl Pts',(9.0607810967537,20.0172662790811,18.));
#36542=CARTESIAN_POINT('Ctrl Pts',(9.0501789809071,20.1027850670435,0.));
#36543=CARTESIAN_POINT('Ctrl Pts',(9.0501789809071,20.1027850670435,18.));
#36544=CARTESIAN_POINT('Ctrl Pts',(9.03891298737031,20.1884025764493,0.));
#36545=CARTESIAN_POINT('Ctrl Pts',(9.03891298737031,20.1884025764493,18.));
#36546=CARTESIAN_POINT('Ctrl Pts',(9.02698833758324,20.2741136736186,0.));
#36547=CARTESIAN_POINT('Ctrl Pts',(9.02698833758324,20.2741136736186,18.));
#36548=CARTESIAN_POINT('Ctrl Pts',(9.01440965049155,20.3599135373691,0.));
#36549=CARTESIAN_POINT('Ctrl Pts',(9.01440965049155,20.3599135373691,18.));
#36550=CARTESIAN_POINT('Ctrl Pts',(9.00118097039517,20.4457976315472,0.));
#36551=CARTESIAN_POINT('Ctrl Pts',(9.00118097039517,20.4457976315472,18.));
#36552=CARTESIAN_POINT('Ctrl Pts',(8.98730595457659,20.5317616031369,0.));
#36553=CARTESIAN_POINT('Ctrl Pts',(8.98730595457659,20.5317616031369,18.));
#36554=CARTESIAN_POINT('Ctrl Pts',(8.97278801890468,20.6178012000199,0.));
#36555=CARTESIAN_POINT('Ctrl Pts',(8.97278801890468,20.6178012000199,18.));
#36556=CARTESIAN_POINT('Ctrl Pts',(8.95763049112623,20.7039121898975,0.));
#36557=CARTESIAN_POINT('Ctrl Pts',(8.95763049112623,20.7039121898975,18.));
#36558=CARTESIAN_POINT('Ctrl Pts',(8.94183680111377,20.7900902537083,0.));
#36559=CARTESIAN_POINT('Ctrl Pts',(8.94183680111377,20.7900902537083,18.));
#36560=CARTESIAN_POINT('Ctrl Pts',(8.92541048738648,20.8763310073304,0.));
#36561=CARTESIAN_POINT('Ctrl Pts',(8.92541048738648,20.8763310073304,18.));
#36562=CARTESIAN_POINT('Ctrl Pts',(8.90835509843285,20.9626300944902,0.));
#36563=CARTESIAN_POINT('Ctrl Pts',(8.90835509843285,20.9626300944902,18.));
#36564=CARTESIAN_POINT('Ctrl Pts',(8.89067412773385,21.0489832630915,0.));
#36565=CARTESIAN_POINT('Ctrl Pts',(8.89067412773385,21.0489832630915,18.));
#36566=CARTESIAN_POINT('Ctrl Pts',(8.87237094640748,21.1353864352374,0.));
#36567=CARTESIAN_POINT('Ctrl Pts',(8.87237094640748,21.1353864352374,18.));
#36568=CARTESIAN_POINT('Ctrl Pts',(8.85344872418155,21.2218358113425,0.));
#36569=CARTESIAN_POINT('Ctrl Pts',(8.85344872418155,21.2218358113425,18.));
#36570=CARTESIAN_POINT('Ctrl Pts',(8.83391042911628,21.3083278326642,0.));
#36571=CARTESIAN_POINT('Ctrl Pts',(8.83391042911628,21.3083278326642,18.));
#36572=CARTESIAN_POINT('Ctrl Pts',(8.81375890120581,21.3948590173441,0.));
#36573=CARTESIAN_POINT('Ctrl Pts',(8.81375890120581,21.3948590173441,18.));
#36574=CARTESIAN_POINT('Ctrl Pts',(8.79299691277858,21.481425822209,0.));
#36575=CARTESIAN_POINT('Ctrl Pts',(8.79299691277858,21.481425822209,18.));
#36576=CARTESIAN_POINT('Ctrl Pts',(8.77162723103298,21.5680245138584,0.));
#36577=CARTESIAN_POINT('Ctrl Pts',(8.77162723103298,21.5680245138584,18.));
#36578=CARTESIAN_POINT('Ctrl Pts',(8.74965270266163,21.6546509866725,0.));
#36579=CARTESIAN_POINT('Ctrl Pts',(8.74965270266163,21.6546509866725,18.));
#36580=CARTESIAN_POINT('Ctrl Pts',(8.72707626956922,21.7413007707864,0.));
#36581=CARTESIAN_POINT('Ctrl Pts',(8.72707626956922,21.7413007707864,18.));
#36582=CARTESIAN_POINT('Ctrl Pts',(8.70390086252203,21.8279693631274,0.));
#36583=CARTESIAN_POINT('Ctrl Pts',(8.70390086252203,21.8279693631274,18.));
#36584=CARTESIAN_POINT('Ctrl Pts',(8.68012932645739,21.9146524902336,0.));
#36585=CARTESIAN_POINT('Ctrl Pts',(8.68012932645739,21.9146524902336,18.));
#36586=CARTESIAN_POINT('Ctrl Pts',(8.6557643376698,22.0013463859623,0.));
#36587=CARTESIAN_POINT('Ctrl Pts',(8.6557643376698,22.0013463859623,18.));
#36588=CARTESIAN_POINT('Ctrl Pts',(8.63080832792612,22.0880480931906,0.));
#36589=CARTESIAN_POINT('Ctrl Pts',(8.63080832792612,22.0880480931906,18.));
#36590=CARTESIAN_POINT('Ctrl Pts',(8.60526341207614,22.1747556651024,0.));
#36591=CARTESIAN_POINT('Ctrl Pts',(8.60526341207614,22.1747556651024,18.));
#36592=CARTESIAN_POINT('Ctrl Pts',(8.57913133085326,22.2614679221213,0.));
#36593=CARTESIAN_POINT('Ctrl Pts',(8.57913133085326,22.2614679221213,18.));
#36594=CARTESIAN_POINT('Ctrl Pts',(8.55775698160722,22.3308410047044,0.));
#36595=CARTESIAN_POINT('Ctrl Pts',(8.55775698160722,22.3308410047044,18.));
#36596=CARTESIAN_POINT('Ctrl Pts',(8.54146295656907,22.3828725698612,0.));
#36597=CARTESIAN_POINT('Ctrl Pts',(8.54146295656907,22.3828725698612,18.));
#36598=CARTESIAN_POINT('Ctrl Pts',(8.53048330625155,22.4175610589877,0.));
#36599=CARTESIAN_POINT('Ctrl Pts',(8.53048330625155,22.4175610589877,18.));
#36600=CARTESIAN_POINT('Ctrl Pts',(8.52496423935285,22.4349054983023,0.));
#36601=CARTESIAN_POINT('Ctrl Pts',(8.52496423935285,22.4349054983023,18.));
#36602=CARTESIAN_POINT('Ctrl Pts',(8.78085409196639,16.6164222996225,0.));
#36603=CARTESIAN_POINT('Ctrl Pts',(8.78817964150686,16.6302847808193,0.));
#36604=CARTESIAN_POINT('Ctrl Pts',(8.80233481798951,16.6582257921024,0.));
#36605=CARTESIAN_POINT('Ctrl Pts',(8.82207984677447,16.7007854423938,0.));
#36606=CARTESIAN_POINT('Ctrl Pts',(8.84558256033742,16.7587634618101,0.));
#36607=CARTESIAN_POINT('Ctrl Pts',(8.87112909692392,16.8329157811062,0.));
#36608=CARTESIAN_POINT('Ctrl Pts',(8.89394614661328,16.908275670167,0.));
#36609=CARTESIAN_POINT('Ctrl Pts',(8.91510993758932,16.9843788566346,0.));
#36610=CARTESIAN_POINT('Ctrl Pts',(8.93538377395243,17.0608897634975,0.));
#36611=CARTESIAN_POINT('Ctrl Pts',(8.95502702208203,17.1376822726252,0.));
#36612=CARTESIAN_POINT('Ctrl Pts',(8.97397941759265,17.2147637614528,0.));
#36613=CARTESIAN_POINT('Ctrl Pts',(8.99199362652257,17.2922207948279,0.));
#36614=CARTESIAN_POINT('Ctrl Pts',(9.00877780436037,17.3701605263553,0.));
#36615=CARTESIAN_POINT('Ctrl Pts',(9.0241575097608,17.4486443043185,0.));
#36616=CARTESIAN_POINT('Ctrl Pts',(9.03814678971601,17.5276582702181,0.));
#36617=CARTESIAN_POINT('Ctrl Pts',(9.05086524971401,17.6071467783263,0.));
#36618=CARTESIAN_POINT('Ctrl Pts',(9.06248904941395,17.6870319618808,0.));
#36619=CARTESIAN_POINT('Ctrl Pts',(9.07319314215026,17.7672369091005,0.));
#36620=CARTESIAN_POINT('Ctrl Pts',(9.08308548608349,17.8477120247758,0.));
#36621=CARTESIAN_POINT('Ctrl Pts',(9.09219303320079,17.9284406141976,0.));
#36622=CARTESIAN_POINT('Ctrl Pts',(9.10049631917583,18.0094249416472,0.));
#36623=CARTESIAN_POINT('Ctrl Pts',(9.10795114540259,18.0906774757189,0.));
#36624=CARTESIAN_POINT('Ctrl Pts',(9.11451347590539,18.1722108451637,0.));
#36625=CARTESIAN_POINT('Ctrl Pts',(9.12016808144599,18.2540262849075,0.));
#36626=CARTESIAN_POINT('Ctrl Pts',(9.12493031448671,18.3361129010289,0.));
#36627=CARTESIAN_POINT('Ctrl Pts',(9.12883240135631,18.4184531695731,0.));
#36628=CARTESIAN_POINT('Ctrl Pts',(9.13191425549883,18.5010266156389,0.));
#36629=CARTESIAN_POINT('Ctrl Pts',(9.13421321934922,18.5838139250423,0.));
#36630=CARTESIAN_POINT('Ctrl Pts',(9.13575227582418,18.6668016710749,0.));
#36631=CARTESIAN_POINT('Ctrl Pts',(9.13654074021147,18.7499820263476,0.));
#36632=CARTESIAN_POINT('Ctrl Pts',(9.13657985367154,18.8333505052874,0.));
#36633=CARTESIAN_POINT('Ctrl Pts',(9.13586688858169,18.9169043053388,0.));
#36634=CARTESIAN_POINT('Ctrl Pts',(9.13439956903533,19.0006405223697,0.));
#36635=CARTESIAN_POINT('Ctrl Pts',(9.13218114462419,19.0845541036965,0.));
#36636=CARTESIAN_POINT('Ctrl Pts',(9.12921984349375,19.1686380639041,0.));
#36637=CARTESIAN_POINT('Ctrl Pts',(9.125526627856,19.2528843844341,0.));
#36638=CARTESIAN_POINT('Ctrl Pts',(9.121113479412,19.3372847008483,0.));
#36639=CARTESIAN_POINT('Ctrl Pts',(9.1159915924392,19.4218310275711,0.));
#36640=CARTESIAN_POINT('Ctrl Pts',(9.11016929611336,19.5065165934577,0.));
#36641=CARTESIAN_POINT('Ctrl Pts',(9.10365235736465,19.5913357132276,0.));
#36642=CARTESIAN_POINT('Ctrl Pts',(9.0964449428387,19.6762833927168,0.));
#36643=CARTESIAN_POINT('Ctrl Pts',(9.08855038355402,19.7613550146978,0.));
#36644=CARTESIAN_POINT('Ctrl Pts',(9.07997196979668,19.846546013708,0.));
#36645=CARTESIAN_POINT('Ctrl Pts',(9.0707138821585,19.9318514954605,0.));
#36646=CARTESIAN_POINT('Ctrl Pts',(9.0607810967537,20.0172662790811,0.));
#36647=CARTESIAN_POINT('Ctrl Pts',(9.0501789809071,20.1027850670435,0.));
#36648=CARTESIAN_POINT('Ctrl Pts',(9.03891298737031,20.1884025764493,0.));
#36649=CARTESIAN_POINT('Ctrl Pts',(9.02698833758324,20.2741136736186,0.));
#36650=CARTESIAN_POINT('Ctrl Pts',(9.01440965049155,20.3599135373691,0.));
#36651=CARTESIAN_POINT('Ctrl Pts',(9.00118097039517,20.4457976315472,0.));
#36652=CARTESIAN_POINT('Ctrl Pts',(8.98730595457659,20.5317616031369,0.));
#36653=CARTESIAN_POINT('Ctrl Pts',(8.97278801890468,20.6178012000199,0.));
#36654=CARTESIAN_POINT('Ctrl Pts',(8.95763049112623,20.7039121898975,0.));
#36655=CARTESIAN_POINT('Ctrl Pts',(8.94183680111377,20.7900902537083,0.));
#36656=CARTESIAN_POINT('Ctrl Pts',(8.92541048738648,20.8763310073304,0.));
#36657=CARTESIAN_POINT('Ctrl Pts',(8.90835509843285,20.9626300944902,0.));
#36658=CARTESIAN_POINT('Ctrl Pts',(8.89067412773385,21.0489832630915,0.));
#36659=CARTESIAN_POINT('Ctrl Pts',(8.87237094640748,21.1353864352374,0.));
#36660=CARTESIAN_POINT('Ctrl Pts',(8.85344872418155,21.2218358113425,0.));
#36661=CARTESIAN_POINT('Ctrl Pts',(8.83391042911628,21.3083278326642,0.));
#36662=CARTESIAN_POINT('Ctrl Pts',(8.81375890120581,21.3948590173441,0.));
#36663=CARTESIAN_POINT('Ctrl Pts',(8.79299691277858,21.481425822209,0.));
#36664=CARTESIAN_POINT('Ctrl Pts',(8.77162723103298,21.5680245138584,0.));
#36665=CARTESIAN_POINT('Ctrl Pts',(8.74965270266163,21.6546509866725,0.));
#36666=CARTESIAN_POINT('Ctrl Pts',(8.72707626956922,21.7413007707864,0.));
#36667=CARTESIAN_POINT('Ctrl Pts',(8.70390086252203,21.8279693631274,0.));
#36668=CARTESIAN_POINT('Ctrl Pts',(8.68012932645739,21.9146524902336,0.));
#36669=CARTESIAN_POINT('Ctrl Pts',(8.6557643376698,22.0013463859623,0.));
#36670=CARTESIAN_POINT('Ctrl Pts',(8.63080832792612,22.0880480931906,0.));
#36671=CARTESIAN_POINT('Ctrl Pts',(8.60015442890614,22.1920971794848,0.));
#36672=CARTESIAN_POINT('Ctrl Pts',(8.57387555634004,22.2788106077804,0.));
#36673=CARTESIAN_POINT('Ctrl Pts',(8.55238412336295,22.3481844703457,0.));
#36674=CARTESIAN_POINT('Ctrl Pts',(8.53600237317213,22.4002166196189,0.));
#36675=CARTESIAN_POINT('Ctrl Pts',(8.52496423935285,22.4349054983023,0.));
#36676=CARTESIAN_POINT('Ctrl Pts',(8.78085409196639,16.6164222996225,15.));
#36677=CARTESIAN_POINT('Ctrl Pts',(8.78817964150686,16.6302847808193,15.));
#36678=CARTESIAN_POINT('Ctrl Pts',(8.80233481798951,16.6582257921024,15.));
#36679=CARTESIAN_POINT('Ctrl Pts',(8.82207984677447,16.7007854423938,15.));
#36680=CARTESIAN_POINT('Ctrl Pts',(8.84558256033742,16.7587634618101,15.));
#36681=CARTESIAN_POINT('Ctrl Pts',(8.87112909692392,16.8329157811062,15.));
#36682=CARTESIAN_POINT('Ctrl Pts',(8.89394614661328,16.908275670167,15.));
#36683=CARTESIAN_POINT('Ctrl Pts',(8.91510993758932,16.9843788566346,15.));
#36684=CARTESIAN_POINT('Ctrl Pts',(8.93538377395243,17.0608897634975,15.));
#36685=CARTESIAN_POINT('Ctrl Pts',(8.95502702208203,17.1376822726252,15.));
#36686=CARTESIAN_POINT('Ctrl Pts',(8.97397941759265,17.2147637614528,15.));
#36687=CARTESIAN_POINT('Ctrl Pts',(8.99199362652257,17.2922207948279,15.));
#36688=CARTESIAN_POINT('Ctrl Pts',(9.00877780436037,17.3701605263553,15.));
#36689=CARTESIAN_POINT('Ctrl Pts',(9.0241575097608,17.4486443043185,15.));
#36690=CARTESIAN_POINT('Ctrl Pts',(9.03814678971601,17.5276582702181,15.));
#36691=CARTESIAN_POINT('Ctrl Pts',(9.05086524971401,17.6071467783263,15.));
#36692=CARTESIAN_POINT('Ctrl Pts',(9.06248904941395,17.6870319618808,15.));
#36693=CARTESIAN_POINT('Ctrl Pts',(9.07319314215026,17.7672369091005,15.));
#36694=CARTESIAN_POINT('Ctrl Pts',(9.08308548608349,17.8477120247758,15.));
#36695=CARTESIAN_POINT('Ctrl Pts',(9.09219303320079,17.9284406141976,15.));
#36696=CARTESIAN_POINT('Ctrl Pts',(9.10049631917583,18.0094249416472,15.));
#36697=CARTESIAN_POINT('Ctrl Pts',(9.10795114540259,18.0906774757189,15.));
#36698=CARTESIAN_POINT('Ctrl Pts',(9.11451347590539,18.1722108451637,15.));
#36699=CARTESIAN_POINT('Ctrl Pts',(9.12016808144599,18.2540262849075,15.));
#36700=CARTESIAN_POINT('Ctrl Pts',(9.12493031448671,18.3361129010289,15.));
#36701=CARTESIAN_POINT('Ctrl Pts',(9.12883240135631,18.4184531695731,15.));
#36702=CARTESIAN_POINT('Ctrl Pts',(9.13191425549883,18.5010266156389,15.));
#36703=CARTESIAN_POINT('Ctrl Pts',(9.13421321934922,18.5838139250423,15.));
#36704=CARTESIAN_POINT('Ctrl Pts',(9.13575227582418,18.6668016710749,15.));
#36705=CARTESIAN_POINT('Ctrl Pts',(9.13654074021147,18.7499820263476,15.));
#36706=CARTESIAN_POINT('Ctrl Pts',(9.13657985367154,18.8333505052874,15.));
#36707=CARTESIAN_POINT('Ctrl Pts',(9.13586688858169,18.9169043053388,15.));
#36708=CARTESIAN_POINT('Ctrl Pts',(9.13439956903533,19.0006405223697,15.));
#36709=CARTESIAN_POINT('Ctrl Pts',(9.13218114462419,19.0845541036965,15.));
#36710=CARTESIAN_POINT('Ctrl Pts',(9.12921984349375,19.1686380639041,15.));
#36711=CARTESIAN_POINT('Ctrl Pts',(9.125526627856,19.2528843844341,15.));
#36712=CARTESIAN_POINT('Ctrl Pts',(9.121113479412,19.3372847008483,15.));
#36713=CARTESIAN_POINT('Ctrl Pts',(9.1159915924392,19.4218310275711,15.));
#36714=CARTESIAN_POINT('Ctrl Pts',(9.11016929611336,19.5065165934577,15.));
#36715=CARTESIAN_POINT('Ctrl Pts',(9.10365235736465,19.5913357132276,15.));
#36716=CARTESIAN_POINT('Ctrl Pts',(9.0964449428387,19.6762833927168,15.));
#36717=CARTESIAN_POINT('Ctrl Pts',(9.08855038355402,19.7613550146978,15.));
#36718=CARTESIAN_POINT('Ctrl Pts',(9.07997196979668,19.846546013708,15.));
#36719=CARTESIAN_POINT('Ctrl Pts',(9.0707138821585,19.9318514954605,15.));
#36720=CARTESIAN_POINT('Ctrl Pts',(9.0607810967537,20.0172662790811,15.));
#36721=CARTESIAN_POINT('Ctrl Pts',(9.0501789809071,20.1027850670435,15.));
#36722=CARTESIAN_POINT('Ctrl Pts',(9.03891298737031,20.1884025764493,15.));
#36723=CARTESIAN_POINT('Ctrl Pts',(9.02698833758324,20.2741136736186,15.));
#36724=CARTESIAN_POINT('Ctrl Pts',(9.01440965049155,20.3599135373691,15.));
#36725=CARTESIAN_POINT('Ctrl Pts',(9.00118097039517,20.4457976315472,15.));
#36726=CARTESIAN_POINT('Ctrl Pts',(8.98730595457659,20.5317616031369,15.));
#36727=CARTESIAN_POINT('Ctrl Pts',(8.97278801890468,20.6178012000199,15.));
#36728=CARTESIAN_POINT('Ctrl Pts',(8.95763049112623,20.7039121898975,15.));
#36729=CARTESIAN_POINT('Ctrl Pts',(8.94183680111377,20.7900902537083,15.));
#36730=CARTESIAN_POINT('Ctrl Pts',(8.92541048738648,20.8763310073304,15.));
#36731=CARTESIAN_POINT('Ctrl Pts',(8.90835509843285,20.9626300944902,15.));
#36732=CARTESIAN_POINT('Ctrl Pts',(8.89067412773385,21.0489832630915,15.));
#36733=CARTESIAN_POINT('Ctrl Pts',(8.87237094640748,21.1353864352374,15.));
#36734=CARTESIAN_POINT('Ctrl Pts',(8.85344872418155,21.2218358113425,15.));
#36735=CARTESIAN_POINT('Ctrl Pts',(8.83391042911628,21.3083278326642,15.));
#36736=CARTESIAN_POINT('Ctrl Pts',(8.81375890120581,21.3948590173441,15.));
#36737=CARTESIAN_POINT('Ctrl Pts',(8.79299691277858,21.481425822209,15.));
#36738=CARTESIAN_POINT('Ctrl Pts',(8.77162723103298,21.5680245138584,15.));
#36739=CARTESIAN_POINT('Ctrl Pts',(8.74965270266163,21.6546509866725,15.));
#36740=CARTESIAN_POINT('Ctrl Pts',(8.72707626956922,21.7413007707864,15.));
#36741=CARTESIAN_POINT('Ctrl Pts',(8.70390086252203,21.8279693631274,15.));
#36742=CARTESIAN_POINT('Ctrl Pts',(8.68012932645739,21.9146524902336,15.));
#36743=CARTESIAN_POINT('Ctrl Pts',(8.6557643376698,22.0013463859623,15.));
#36744=CARTESIAN_POINT('Ctrl Pts',(8.63080832792612,22.0880480931906,15.));
#36745=CARTESIAN_POINT('Ctrl Pts',(8.60015442890614,22.1920971794848,15.));
#36746=CARTESIAN_POINT('Ctrl Pts',(8.57387555634004,22.2788106077804,15.));
#36747=CARTESIAN_POINT('Ctrl Pts',(8.55238412336295,22.3481844703457,15.));
#36748=CARTESIAN_POINT('Ctrl Pts',(8.53600237317213,22.4002166196189,15.));
#36749=CARTESIAN_POINT('Ctrl Pts',(8.52496423935285,22.4349054983023,15.));
#36750=CARTESIAN_POINT('Ctrl Pts',(18.7025042402277,15.040489857191,0.));
#36751=CARTESIAN_POINT('Ctrl Pts',(18.7025042402277,15.040489857191,18.));
#36752=CARTESIAN_POINT('Ctrl Pts',(18.6843032127312,15.0403790752228,0.));
#36753=CARTESIAN_POINT('Ctrl Pts',(18.6843032127312,15.0403790752228,18.));
#36754=CARTESIAN_POINT('Ctrl Pts',(18.6479196005666,15.0401020105546,0.));
#36755=CARTESIAN_POINT('Ctrl Pts',(18.6479196005666,15.0401020105546,18.));
#36756=CARTESIAN_POINT('Ctrl Pts',(18.5933995108277,15.0395199113665,0.));
#36757=CARTESIAN_POINT('Ctrl Pts',(18.5933995108277,15.0395199113665,18.));
#36758=CARTESIAN_POINT('Ctrl Pts',(18.5208167514208,15.0384106640282,0.));
#36759=CARTESIAN_POINT('Ctrl Pts',(18.5208167514208,15.0384106640282,18.));
#36760=CARTESIAN_POINT('Ctrl Pts',(18.4302732371441,15.0364681891201,0.));
#36761=CARTESIAN_POINT('Ctrl Pts',(18.4302732371441,15.0364681891201,18.));
#36762=CARTESIAN_POINT('Ctrl Pts',(18.3399156227477,15.0339687345357,0.));
#36763=CARTESIAN_POINT('Ctrl Pts',(18.3399156227477,15.0339687345357,18.));
#36764=CARTESIAN_POINT('Ctrl Pts',(18.2497455679917,15.0309110092482,0.));
#36765=CARTESIAN_POINT('Ctrl Pts',(18.2497455679917,15.0309110092482,18.));
#36766=CARTESIAN_POINT('Ctrl Pts',(18.1597655779328,15.0272936035154,0.));
#36767=CARTESIAN_POINT('Ctrl Pts',(18.1597655779328,15.0272936035154,18.));
#36768=CARTESIAN_POINT('Ctrl Pts',(18.0699792164192,15.0231151183906,0.));
#36769=CARTESIAN_POINT('Ctrl Pts',(18.0699792164192,15.0231151183906,18.));
#36770=CARTESIAN_POINT('Ctrl Pts',(17.980390892286,15.0183741723687,0.));
#36771=CARTESIAN_POINT('Ctrl Pts',(17.980390892286,15.0183741723687,18.));
#36772=CARTESIAN_POINT('Ctrl Pts',(17.891005548971,15.0130693803259,0.));
#36773=CARTESIAN_POINT('Ctrl Pts',(17.891005548971,15.0130693803259,18.));
#36774=CARTESIAN_POINT('Ctrl Pts',(17.8018283748074,15.0071993464636,0.));
#36775=CARTESIAN_POINT('Ctrl Pts',(17.8018283748074,15.0071993464636,18.));
#36776=CARTESIAN_POINT('Ctrl Pts',(17.7128645299878,15.0007626541286,0.));
#36777=CARTESIAN_POINT('Ctrl Pts',(17.7128645299878,15.0007626541286,18.));
#36778=CARTESIAN_POINT('Ctrl Pts',(17.6241187988652,14.9937578646616,0.));
#36779=CARTESIAN_POINT('Ctrl Pts',(17.6241187988652,14.9937578646616,18.));
#36780=CARTESIAN_POINT('Ctrl Pts',(17.5355955872257,14.9861834999847,0.));
#36781=CARTESIAN_POINT('Ctrl Pts',(17.5355955872257,14.9861834999847,18.));
#36782=CARTESIAN_POINT('Ctrl Pts',(17.4472991215239,14.9780380183576,0.));
#36783=CARTESIAN_POINT('Ctrl Pts',(17.4472991215239,14.9780380183576,18.));
#36784=CARTESIAN_POINT('Ctrl Pts',(17.3592335908103,14.9693197947387,0.));
#36785=CARTESIAN_POINT('Ctrl Pts',(17.3592335908103,14.9693197947387,18.));
#36786=CARTESIAN_POINT('Ctrl Pts',(17.2714032968314,14.9600271060471,0.));
#36787=CARTESIAN_POINT('Ctrl Pts',(17.2714032968314,14.9600271060471,18.));
#36788=CARTESIAN_POINT('Ctrl Pts',(17.1838128327073,14.9501581118289,0.));
#36789=CARTESIAN_POINT('Ctrl Pts',(17.1838128327073,14.9501581118289,18.));
#36790=CARTESIAN_POINT('Ctrl Pts',(17.0964671184813,14.9397108660998,0.));
#36791=CARTESIAN_POINT('Ctrl Pts',(17.0964671184813,14.9397108660998,18.));
#36792=CARTESIAN_POINT('Ctrl Pts',(17.0093712776822,14.9286833603319,0.));
#36793=CARTESIAN_POINT('Ctrl Pts',(17.0093712776822,14.9286833603319,18.));
#36794=CARTESIAN_POINT('Ctrl Pts',(16.9225305499155,14.9170735658747,0.));
#36795=CARTESIAN_POINT('Ctrl Pts',(16.9225305499155,14.9170735658747,18.));
#36796=CARTESIAN_POINT('Ctrl Pts',(16.8359501981915,14.9048794721647,0.));
#36797=CARTESIAN_POINT('Ctrl Pts',(16.8359501981915,14.9048794721647,18.));
#36798=CARTESIAN_POINT('Ctrl Pts',(16.7496353900706,14.8920991518626,0.));
#36799=CARTESIAN_POINT('Ctrl Pts',(16.7496353900706,14.8920991518626,18.));
#36800=CARTESIAN_POINT('Ctrl Pts',(16.6635911790385,14.8787307479454,0.));
#36801=CARTESIAN_POINT('Ctrl Pts',(16.6635911790385,14.8787307479454,18.));
#36802=CARTESIAN_POINT('Ctrl Pts',(16.5778226646614,14.8647723257055,0.));
#36803=CARTESIAN_POINT('Ctrl Pts',(16.5778226646614,14.8647723257055,18.));
#36804=CARTESIAN_POINT('Ctrl Pts',(16.492335117066,14.8502217520165,0.));
#36805=CARTESIAN_POINT('Ctrl Pts',(16.492335117066,14.8502217520165,18.));
#36806=CARTESIAN_POINT('Ctrl Pts',(16.4071341001481,14.8350765822692,0.));
#36807=CARTESIAN_POINT('Ctrl Pts',(16.4071341001481,14.8350765822692,18.));
#36808=CARTESIAN_POINT('Ctrl Pts',(16.3222256264574,14.8193339134125,0.));
#36809=CARTESIAN_POINT('Ctrl Pts',(16.3222256264574,14.8193339134125,18.));
#36810=CARTESIAN_POINT('Ctrl Pts',(16.2376161919272,14.8029903659562,0.));
#36811=CARTESIAN_POINT('Ctrl Pts',(16.2376161919272,14.8029903659562,18.));
#36812=CARTESIAN_POINT('Ctrl Pts',(16.1533125058853,14.7860423865308,0.));
#36813=CARTESIAN_POINT('Ctrl Pts',(16.1533125058853,14.7860423865308,18.));
#36814=CARTESIAN_POINT('Ctrl Pts',(16.0693212651732,14.7684865075326,0.));
#36815=CARTESIAN_POINT('Ctrl Pts',(16.0693212651732,14.7684865075326,18.));
#36816=CARTESIAN_POINT('Ctrl Pts',(15.9856489347991,14.7503195973741,0.));
#36817=CARTESIAN_POINT('Ctrl Pts',(15.9856489347991,14.7503195973741,18.));
#36818=CARTESIAN_POINT('Ctrl Pts',(15.9023014613802,14.7315391924939,0.));
#36819=CARTESIAN_POINT('Ctrl Pts',(15.9023014613802,14.7315391924939,18.));
#36820=CARTESIAN_POINT('Ctrl Pts',(15.8192842036838,14.7121435744495,0.));
#36821=CARTESIAN_POINT('Ctrl Pts',(15.8192842036838,14.7121435744495,18.));
#36822=CARTESIAN_POINT('Ctrl Pts',(15.7366025822956,14.692131002056,0.));
#36823=CARTESIAN_POINT('Ctrl Pts',(15.7366025822956,14.692131002056,18.));
#36824=CARTESIAN_POINT('Ctrl Pts',(15.6542626345121,14.6714990558793,0.));
#36825=CARTESIAN_POINT('Ctrl Pts',(15.6542626345121,14.6714990558793,18.));
#36826=CARTESIAN_POINT('Ctrl Pts',(15.5722715494357,14.6502440080911,0.));
#36827=CARTESIAN_POINT('Ctrl Pts',(15.5722715494357,14.6502440080911,18.));
#36828=CARTESIAN_POINT('Ctrl Pts',(15.4906383406647,14.6283600295736,0.));
#36829=CARTESIAN_POINT('Ctrl Pts',(15.4906383406647,14.6283600295736,18.));
#36830=CARTESIAN_POINT('Ctrl Pts',(15.4093740621548,14.6058389416146,0.));
#36831=CARTESIAN_POINT('Ctrl Pts',(15.4093740621548,14.6058389416146,18.));
#36832=CARTESIAN_POINT('Ctrl Pts',(15.3284903715086,14.5826719336929,0.));
#36833=CARTESIAN_POINT('Ctrl Pts',(15.3284903715086,14.5826719336929,18.));
#36834=CARTESIAN_POINT('Ctrl Pts',(15.2479982823383,14.5588510579962,0.));
#36835=CARTESIAN_POINT('Ctrl Pts',(15.2479982823383,14.5588510579962,18.));
#36836=CARTESIAN_POINT('Ctrl Pts',(15.1679069808052,14.534370647705,0.));
#36837=CARTESIAN_POINT('Ctrl Pts',(15.1679069808052,14.534370647705,18.));
#36838=CARTESIAN_POINT('Ctrl Pts',(15.0882222764759,14.5092291736391,0.));
#36839=CARTESIAN_POINT('Ctrl Pts',(15.0882222764759,14.5092291736391,18.));
#36840=CARTESIAN_POINT('Ctrl Pts',(15.0089462280505,14.4834296977405,0.));
#36841=CARTESIAN_POINT('Ctrl Pts',(15.0089462280505,14.4834296977405,18.));
#36842=CARTESIAN_POINT('Ctrl Pts',(14.9300806580357,14.4569756801697,0.));
#36843=CARTESIAN_POINT('Ctrl Pts',(14.9300806580357,14.4569756801697,18.));
#36844=CARTESIAN_POINT('Ctrl Pts',(14.8516302160049,14.4298673266313,0.));
#36845=CARTESIAN_POINT('Ctrl Pts',(14.8516302160049,14.4298673266313,18.));
#36846=CARTESIAN_POINT('Ctrl Pts',(14.7736052248294,14.4020981965564,0.));
#36847=CARTESIAN_POINT('Ctrl Pts',(14.7736052248294,14.4020981965564,18.));
#36848=CARTESIAN_POINT('Ctrl Pts',(14.6960255561799,14.3736505809735,0.));
#36849=CARTESIAN_POINT('Ctrl Pts',(14.6960255561799,14.3736505809735,18.));
#36850=CARTESIAN_POINT('Ctrl Pts',(14.6189211183837,14.3444949335274,0.));
#36851=CARTESIAN_POINT('Ctrl Pts',(14.6189211183837,14.3444949335274,18.));
#36852=CARTESIAN_POINT('Ctrl Pts',(14.5423237181615,14.3145996213697,0.));
#36853=CARTESIAN_POINT('Ctrl Pts',(14.5423237181615,14.3145996213697,18.));
#36854=CARTESIAN_POINT('Ctrl Pts',(14.4662599802682,14.2839394106401,0.));
#36855=CARTESIAN_POINT('Ctrl Pts',(14.4662599802682,14.2839394106401,18.));
#36856=CARTESIAN_POINT('Ctrl Pts',(14.3907450096103,14.2525030666863,0.));
#36857=CARTESIAN_POINT('Ctrl Pts',(14.3907450096103,14.2525030666863,18.));
#36858=CARTESIAN_POINT('Ctrl Pts',(14.3157729256101,14.2203046917613,0.));
#36859=CARTESIAN_POINT('Ctrl Pts',(14.3157729256101,14.2203046917613,18.));
#36860=CARTESIAN_POINT('Ctrl Pts',(14.2413181097468,14.1873822640681,0.));
#36861=CARTESIAN_POINT('Ctrl Pts',(14.2413181097468,14.1873822640681,18.));
#36862=CARTESIAN_POINT('Ctrl Pts',(14.1673550455622,14.1537739659715,0.));
#36863=CARTESIAN_POINT('Ctrl Pts',(14.1673550455622,14.1537739659715,18.));
#36864=CARTESIAN_POINT('Ctrl Pts',(14.0938755647891,14.1194976094444,0.));
#36865=CARTESIAN_POINT('Ctrl Pts',(14.0938755647891,14.1194976094444,18.));
#36866=CARTESIAN_POINT('Ctrl Pts',(14.0209038736616,14.0845327205726,0.));
#36867=CARTESIAN_POINT('Ctrl Pts',(14.0209038736616,14.0845327205726,18.));
#36868=CARTESIAN_POINT('Ctrl Pts',(13.9485205009332,14.0487919508068,0.));
#36869=CARTESIAN_POINT('Ctrl Pts',(13.9485205009332,14.0487919508068,18.));
#36870=CARTESIAN_POINT('Ctrl Pts',(13.876852657608,14.0121326766855,0.));
#36871=CARTESIAN_POINT('Ctrl Pts',(13.876852657608,14.0121326766855,18.));
#36872=CARTESIAN_POINT('Ctrl Pts',(13.806028835706,13.9744114225699,0.));
#36873=CARTESIAN_POINT('Ctrl Pts',(13.806028835706,13.9744114225699,18.));
#36874=CARTESIAN_POINT('Ctrl Pts',(13.7361389175879,13.9355316323567,0.));
#36875=CARTESIAN_POINT('Ctrl Pts',(13.7361389175879,13.9355316323567,18.));
#36876=CARTESIAN_POINT('Ctrl Pts',(13.6672004242289,13.8954842290745,0.));
#36877=CARTESIAN_POINT('Ctrl Pts',(13.6672004242289,13.8954842290745,18.));
#36878=CARTESIAN_POINT('Ctrl Pts',(13.5991011046042,13.854416158639,0.));
#36879=CARTESIAN_POINT('Ctrl Pts',(13.5991011046042,13.854416158639,18.));
#36880=CARTESIAN_POINT('Ctrl Pts',(13.5316488646659,13.8125718693898,0.));
#36881=CARTESIAN_POINT('Ctrl Pts',(13.5316488646659,13.8125718693898,18.));
#36882=CARTESIAN_POINT('Ctrl Pts',(13.4646849459541,13.7701598398937,0.));
#36883=CARTESIAN_POINT('Ctrl Pts',(13.4646849459541,13.7701598398937,18.));
#36884=CARTESIAN_POINT('Ctrl Pts',(13.3981837093919,13.7272351052346,0.));
#36885=CARTESIAN_POINT('Ctrl Pts',(13.3981837093919,13.7272351052346,18.));
#36886=CARTESIAN_POINT('Ctrl Pts',(13.332345249068,13.6835899659728,0.));
#36887=CARTESIAN_POINT('Ctrl Pts',(13.332345249068,13.6835899659728,18.));
#36888=CARTESIAN_POINT('Ctrl Pts',(13.267724591625,13.6386021757691,0.));
#36889=CARTESIAN_POINT('Ctrl Pts',(13.267724591625,13.6386021757691,18.));
#36890=CARTESIAN_POINT('Ctrl Pts',(13.2050958591127,13.5913916488449,0.));
#36891=CARTESIAN_POINT('Ctrl Pts',(13.2050958591127,13.5913916488449,18.));
#36892=CARTESIAN_POINT('Ctrl Pts',(13.1572182238498,13.5511230466604,0.));
#36893=CARTESIAN_POINT('Ctrl Pts',(13.1572182238498,13.5511230466604,18.));
#36894=CARTESIAN_POINT('Ctrl Pts',(13.1228431405579,13.5191927531554,0.));
#36895=CARTESIAN_POINT('Ctrl Pts',(13.1228431405579,13.5191927531554,18.));
#36896=CARTESIAN_POINT('Ctrl Pts',(13.1006438497967,13.4970961329957,0.));
#36897=CARTESIAN_POINT('Ctrl Pts',(13.1006438497967,13.4970961329957,18.));
#36898=CARTESIAN_POINT('Ctrl Pts',(13.0897235660237,13.4858453790958,0.));
#36899=CARTESIAN_POINT('Ctrl Pts',(13.0897235660237,13.4858453790958,18.));
#36900=CARTESIAN_POINT('',(18.7025042402277,15.040489857191,0.));
#36901=CARTESIAN_POINT('Ctrl Pts',(13.0897235660237,13.4858453790958,0.));
#36902=CARTESIAN_POINT('Ctrl Pts',(13.1006438497967,13.4970961329957,0.));
#36903=CARTESIAN_POINT('Ctrl Pts',(13.1228431405579,13.5191927531554,0.));
#36904=CARTESIAN_POINT('Ctrl Pts',(13.1572182238498,13.5511230466604,0.));
#36905=CARTESIAN_POINT('Ctrl Pts',(13.2050958591127,13.5913916488449,0.));
#36906=CARTESIAN_POINT('Ctrl Pts',(13.267724591625,13.6386021757691,0.));
#36907=CARTESIAN_POINT('Ctrl Pts',(13.332345249068,13.6835899659728,0.));
#36908=CARTESIAN_POINT('Ctrl Pts',(13.3981837093919,13.7272351052346,0.));
#36909=CARTESIAN_POINT('Ctrl Pts',(13.4646849459541,13.7701598398937,0.));
#36910=CARTESIAN_POINT('Ctrl Pts',(13.5316488646659,13.8125718693898,0.));
#36911=CARTESIAN_POINT('Ctrl Pts',(13.5991011046042,13.854416158639,0.));
#36912=CARTESIAN_POINT('Ctrl Pts',(13.6672004242289,13.8954842290745,0.));
#36913=CARTESIAN_POINT('Ctrl Pts',(13.7361389175879,13.9355316323567,0.));
#36914=CARTESIAN_POINT('Ctrl Pts',(13.806028835706,13.9744114225699,0.));
#36915=CARTESIAN_POINT('Ctrl Pts',(13.876852657608,14.0121326766855,0.));
#36916=CARTESIAN_POINT('Ctrl Pts',(13.9485205009332,14.0487919508068,0.));
#36917=CARTESIAN_POINT('Ctrl Pts',(14.0209038736616,14.0845327205726,0.));
#36918=CARTESIAN_POINT('Ctrl Pts',(14.0938755647891,14.1194976094444,0.));
#36919=CARTESIAN_POINT('Ctrl Pts',(14.1673550455622,14.1537739659715,0.));
#36920=CARTESIAN_POINT('Ctrl Pts',(14.2413181097468,14.1873822640681,0.));
#36921=CARTESIAN_POINT('Ctrl Pts',(14.3157729256101,14.2203046917613,0.));
#36922=CARTESIAN_POINT('Ctrl Pts',(14.3907450096103,14.2525030666863,0.));
#36923=CARTESIAN_POINT('Ctrl Pts',(14.4662599802682,14.2839394106401,0.));
#36924=CARTESIAN_POINT('Ctrl Pts',(14.5423237181615,14.3145996213697,0.));
#36925=CARTESIAN_POINT('Ctrl Pts',(14.6189211183837,14.3444949335274,0.));
#36926=CARTESIAN_POINT('Ctrl Pts',(14.6960255561799,14.3736505809735,0.));
#36927=CARTESIAN_POINT('Ctrl Pts',(14.7736052248294,14.4020981965564,0.));
#36928=CARTESIAN_POINT('Ctrl Pts',(14.8516302160049,14.4298673266313,0.));
#36929=CARTESIAN_POINT('Ctrl Pts',(14.9300806580357,14.4569756801697,0.));
#36930=CARTESIAN_POINT('Ctrl Pts',(15.0089462280505,14.4834296977405,0.));
#36931=CARTESIAN_POINT('Ctrl Pts',(15.0882222764759,14.5092291736391,0.));
#36932=CARTESIAN_POINT('Ctrl Pts',(15.1679069808052,14.534370647705,0.));
#36933=CARTESIAN_POINT('Ctrl Pts',(15.2479982823383,14.5588510579962,0.));
#36934=CARTESIAN_POINT('Ctrl Pts',(15.3284903715086,14.5826719336929,0.));
#36935=CARTESIAN_POINT('Ctrl Pts',(15.4093740621548,14.6058389416146,0.));
#36936=CARTESIAN_POINT('Ctrl Pts',(15.4906383406647,14.6283600295736,0.));
#36937=CARTESIAN_POINT('Ctrl Pts',(15.5722715494357,14.6502440080911,0.));
#36938=CARTESIAN_POINT('Ctrl Pts',(15.6542626345121,14.6714990558793,0.));
#36939=CARTESIAN_POINT('Ctrl Pts',(15.7366025822956,14.692131002056,0.));
#36940=CARTESIAN_POINT('Ctrl Pts',(15.8192842036838,14.7121435744495,0.));
#36941=CARTESIAN_POINT('Ctrl Pts',(15.9023014613802,14.7315391924939,0.));
#36942=CARTESIAN_POINT('Ctrl Pts',(15.9856489347991,14.7503195973741,0.));
#36943=CARTESIAN_POINT('Ctrl Pts',(16.0693212651732,14.7684865075326,0.));
#36944=CARTESIAN_POINT('Ctrl Pts',(16.1533125058853,14.7860423865308,0.));
#36945=CARTESIAN_POINT('Ctrl Pts',(16.2376161919272,14.8029903659562,0.));
#36946=CARTESIAN_POINT('Ctrl Pts',(16.3222256264574,14.8193339134125,0.));
#36947=CARTESIAN_POINT('Ctrl Pts',(16.4071341001481,14.8350765822692,0.));
#36948=CARTESIAN_POINT('Ctrl Pts',(16.492335117066,14.8502217520165,0.));
#36949=CARTESIAN_POINT('Ctrl Pts',(16.5778226646614,14.8647723257055,0.));
#36950=CARTESIAN_POINT('Ctrl Pts',(16.6635911790385,14.8787307479454,0.));
#36951=CARTESIAN_POINT('Ctrl Pts',(16.7496353900706,14.8920991518626,0.));
#36952=CARTESIAN_POINT('Ctrl Pts',(16.8359501981915,14.9048794721647,0.));
#36953=CARTESIAN_POINT('Ctrl Pts',(16.9225305499155,14.9170735658747,0.));
#36954=CARTESIAN_POINT('Ctrl Pts',(17.0093712776822,14.9286833603319,0.));
#36955=CARTESIAN_POINT('Ctrl Pts',(17.0964671184813,14.9397108660998,0.));
#36956=CARTESIAN_POINT('Ctrl Pts',(17.1838128327073,14.9501581118289,0.));
#36957=CARTESIAN_POINT('Ctrl Pts',(17.2714032968314,14.9600271060471,0.));
#36958=CARTESIAN_POINT('Ctrl Pts',(17.3592335908103,14.9693197947387,0.));
#36959=CARTESIAN_POINT('Ctrl Pts',(17.4472991215239,14.9780380183576,0.));
#36960=CARTESIAN_POINT('Ctrl Pts',(17.5355955872257,14.9861834999847,0.));
#36961=CARTESIAN_POINT('Ctrl Pts',(17.6241187988652,14.9937578646616,0.));
#36962=CARTESIAN_POINT('Ctrl Pts',(17.7128645299878,15.0007626541286,0.));
#36963=CARTESIAN_POINT('Ctrl Pts',(17.8018283748074,15.0071993464636,0.));
#36964=CARTESIAN_POINT('Ctrl Pts',(17.891005548971,15.0130693803259,0.));
#36965=CARTESIAN_POINT('Ctrl Pts',(17.980390892286,15.0183741723687,0.));
#36966=CARTESIAN_POINT('Ctrl Pts',(18.0699792164192,15.0231151183906,0.));
#36967=CARTESIAN_POINT('Ctrl Pts',(18.1597655779328,15.0272936035154,0.));
#36968=CARTESIAN_POINT('Ctrl Pts',(18.2497455679917,15.0309110092482,0.));
#36969=CARTESIAN_POINT('Ctrl Pts',(18.3399156227477,15.0339687345357,0.));
#36970=CARTESIAN_POINT('Ctrl Pts',(18.4483447600234,15.036968080037,0.));
#36971=CARTESIAN_POINT('Ctrl Pts',(18.5389347492702,15.038771310026,0.));
#36972=CARTESIAN_POINT('Ctrl Pts',(18.6115544313469,15.0397694451467,0.));
#36973=CARTESIAN_POINT('Ctrl Pts',(18.6661021851765,15.0402682932586,0.));
#36974=CARTESIAN_POINT('Ctrl Pts',(18.7025042402277,15.040489857191,0.));
#36975=CARTESIAN_POINT('',(18.7025042402277,15.040489857191,15.));
#36976=CARTESIAN_POINT('Ctrl Pts',(18.7025042402277,15.040489857191,15.));
#36977=CARTESIAN_POINT('Ctrl Pts',(18.6843032127312,15.0403790752228,15.));
#36978=CARTESIAN_POINT('Ctrl Pts',(18.6479196005666,15.0401020105546,15.));
#36979=CARTESIAN_POINT('Ctrl Pts',(18.5933995108277,15.0395199113665,15.));
#36980=CARTESIAN_POINT('Ctrl Pts',(18.5208167514208,15.0384106640282,15.));
#36981=CARTESIAN_POINT('Ctrl Pts',(18.4302732371441,15.0364681891201,15.));
#36982=CARTESIAN_POINT('Ctrl Pts',(18.3399156227477,15.0339687345357,15.));
#36983=CARTESIAN_POINT('Ctrl Pts',(18.2497455679917,15.0309110092482,15.));
#36984=CARTESIAN_POINT('Ctrl Pts',(18.1597655779328,15.0272936035154,15.));
#36985=CARTESIAN_POINT('Ctrl Pts',(18.0699792164192,15.0231151183906,15.));
#36986=CARTESIAN_POINT('Ctrl Pts',(17.980390892286,15.0183741723687,15.));
#36987=CARTESIAN_POINT('Ctrl Pts',(17.891005548971,15.0130693803259,15.));
#36988=CARTESIAN_POINT('Ctrl Pts',(17.8018283748074,15.0071993464636,15.));
#36989=CARTESIAN_POINT('Ctrl Pts',(17.7128645299878,15.0007626541286,15.));
#36990=CARTESIAN_POINT('Ctrl Pts',(17.6241187988652,14.9937578646616,15.));
#36991=CARTESIAN_POINT('Ctrl Pts',(17.5355955872257,14.9861834999847,15.));
#36992=CARTESIAN_POINT('Ctrl Pts',(17.4472991215239,14.9780380183576,15.));
#36993=CARTESIAN_POINT('Ctrl Pts',(17.3592335908103,14.9693197947387,15.));
#36994=CARTESIAN_POINT('Ctrl Pts',(17.2714032968314,14.9600271060471,15.));
#36995=CARTESIAN_POINT('Ctrl Pts',(17.1838128327073,14.9501581118289,15.));
#36996=CARTESIAN_POINT('Ctrl Pts',(17.0964671184813,14.9397108660998,15.));
#36997=CARTESIAN_POINT('Ctrl Pts',(17.0093712776822,14.9286833603319,15.));
#36998=CARTESIAN_POINT('Ctrl Pts',(16.9225305499155,14.9170735658747,15.));
#36999=CARTESIAN_POINT('Ctrl Pts',(16.8359501981915,14.9048794721647,15.));
#37000=CARTESIAN_POINT('Ctrl Pts',(16.7496353900706,14.8920991518626,15.));
#37001=CARTESIAN_POINT('Ctrl Pts',(16.6635911790385,14.8787307479454,15.));
#37002=CARTESIAN_POINT('Ctrl Pts',(16.5778226646614,14.8647723257055,15.));
#37003=CARTESIAN_POINT('Ctrl Pts',(16.492335117066,14.8502217520165,15.));
#37004=CARTESIAN_POINT('Ctrl Pts',(16.4071341001481,14.8350765822692,15.));
#37005=CARTESIAN_POINT('Ctrl Pts',(16.3222256264574,14.8193339134125,15.));
#37006=CARTESIAN_POINT('Ctrl Pts',(16.2376161919272,14.8029903659562,15.));
#37007=CARTESIAN_POINT('Ctrl Pts',(16.1533125058853,14.7860423865308,15.));
#37008=CARTESIAN_POINT('Ctrl Pts',(16.0693212651732,14.7684865075326,15.));
#37009=CARTESIAN_POINT('Ctrl Pts',(15.9856489347991,14.7503195973741,15.));
#37010=CARTESIAN_POINT('Ctrl Pts',(15.9023014613802,14.7315391924939,15.));
#37011=CARTESIAN_POINT('Ctrl Pts',(15.8192842036838,14.7121435744495,15.));
#37012=CARTESIAN_POINT('Ctrl Pts',(15.7366025822956,14.692131002056,15.));
#37013=CARTESIAN_POINT('Ctrl Pts',(15.6542626345121,14.6714990558793,15.));
#37014=CARTESIAN_POINT('Ctrl Pts',(15.5722715494357,14.6502440080911,15.));
#37015=CARTESIAN_POINT('Ctrl Pts',(15.4906383406647,14.6283600295736,15.));
#37016=CARTESIAN_POINT('Ctrl Pts',(15.4093740621548,14.6058389416146,15.));
#37017=CARTESIAN_POINT('Ctrl Pts',(15.3284903715086,14.5826719336929,15.));
#37018=CARTESIAN_POINT('Ctrl Pts',(15.2479982823383,14.5588510579962,15.));
#37019=CARTESIAN_POINT('Ctrl Pts',(15.1679069808052,14.534370647705,15.));
#37020=CARTESIAN_POINT('Ctrl Pts',(15.0882222764759,14.5092291736391,15.));
#37021=CARTESIAN_POINT('Ctrl Pts',(15.0089462280505,14.4834296977405,15.));
#37022=CARTESIAN_POINT('Ctrl Pts',(14.9300806580357,14.4569756801697,15.));
#37023=CARTESIAN_POINT('Ctrl Pts',(14.8516302160049,14.4298673266313,15.));
#37024=CARTESIAN_POINT('Ctrl Pts',(14.7736052248294,14.4020981965564,15.));
#37025=CARTESIAN_POINT('Ctrl Pts',(14.6960255561799,14.3736505809735,15.));
#37026=CARTESIAN_POINT('Ctrl Pts',(14.6189211183837,14.3444949335274,15.));
#37027=CARTESIAN_POINT('Ctrl Pts',(14.5423237181615,14.3145996213697,15.));
#37028=CARTESIAN_POINT('Ctrl Pts',(14.4662599802682,14.2839394106401,15.));
#37029=CARTESIAN_POINT('Ctrl Pts',(14.3907450096103,14.2525030666863,15.));
#37030=CARTESIAN_POINT('Ctrl Pts',(14.3157729256101,14.2203046917613,15.));
#37031=CARTESIAN_POINT('Ctrl Pts',(14.2413181097468,14.1873822640681,15.));
#37032=CARTESIAN_POINT('Ctrl Pts',(14.1673550455622,14.1537739659715,15.));
#37033=CARTESIAN_POINT('Ctrl Pts',(14.0938755647891,14.1194976094444,15.));
#37034=CARTESIAN_POINT('Ctrl Pts',(14.0209038736616,14.0845327205726,15.));
#37035=CARTESIAN_POINT('Ctrl Pts',(13.9485205009332,14.0487919508068,15.));
#37036=CARTESIAN_POINT('Ctrl Pts',(13.876852657608,14.0121326766855,15.));
#37037=CARTESIAN_POINT('Ctrl Pts',(13.806028835706,13.9744114225699,15.));
#37038=CARTESIAN_POINT('Ctrl Pts',(13.7361389175879,13.9355316323567,15.));
#37039=CARTESIAN_POINT('Ctrl Pts',(13.6672004242289,13.8954842290745,15.));
#37040=CARTESIAN_POINT('Ctrl Pts',(13.5991011046042,13.854416158639,15.));
#37041=CARTESIAN_POINT('Ctrl Pts',(13.5316488646659,13.8125718693898,15.));
#37042=CARTESIAN_POINT('Ctrl Pts',(13.4646849459541,13.7701598398937,15.));
#37043=CARTESIAN_POINT('Ctrl Pts',(13.3981837093919,13.7272351052346,15.));
#37044=CARTESIAN_POINT('Ctrl Pts',(13.332345249068,13.6835899659728,15.));
#37045=CARTESIAN_POINT('Ctrl Pts',(13.267724591625,13.6386021757691,15.));
#37046=CARTESIAN_POINT('Ctrl Pts',(13.2050958591127,13.5913916488449,15.));
#37047=CARTESIAN_POINT('Ctrl Pts',(13.1572182238498,13.5511230466604,15.));
#37048=CARTESIAN_POINT('Ctrl Pts',(13.1228431405579,13.5191927531554,15.));
#37049=CARTESIAN_POINT('Ctrl Pts',(13.1006438497967,13.4970961329957,15.));
#37050=CARTESIAN_POINT('Ctrl Pts',(13.0897235660237,13.4858453790958,15.));
#37051=CARTESIAN_POINT('',(18.7025042402277,15.040489857191,0.));
#37052=CARTESIAN_POINT('Origin',(9.34524724197225E-14,6.78114261146376E-14,
0.));
#37053=CARTESIAN_POINT('',(20.0837475345526,13.1393715591102,0.));
#37054=CARTESIAN_POINT('Origin',(9.34524724197225E-14,6.78114261146376E-14,
0.));
#37055=CARTESIAN_POINT('',(20.0837475345526,13.1393715591102,15.));
#37056=CARTESIAN_POINT('Origin',(9.34524724197225E-14,6.78114261146376E-14,
15.));
#37057=CARTESIAN_POINT('',(20.0837475345526,13.1393715591102,0.));
#37058=CARTESIAN_POINT('Ctrl Pts',(16.8707481591095,8.28171148831561,0.));
#37059=CARTESIAN_POINT('Ctrl Pts',(16.8707481591095,8.28171148831561,18.));
#37060=CARTESIAN_POINT('Ctrl Pts',(16.8848228151885,8.28862062120315,0.));
#37061=CARTESIAN_POINT('Ctrl Pts',(16.8848228151885,8.28862062120315,18.));
#37062=CARTESIAN_POINT('Ctrl Pts',(16.9126979078877,8.30290517019115,0.));
#37063=CARTESIAN_POINT('Ctrl Pts',(16.9126979078877,8.30290517019115,18.));
#37064=CARTESIAN_POINT('Ctrl Pts',(16.9536879065132,8.32573081382562,0.));
#37065=CARTESIAN_POINT('Ctrl Pts',(16.9536879065132,8.32573081382562,18.));
#37066=CARTESIAN_POINT('Ctrl Pts',(17.0067806259695,8.35882146841243,0.));
#37067=CARTESIAN_POINT('Ctrl Pts',(17.0067806259695,8.35882146841243,18.));
#37068=CARTESIAN_POINT('Ctrl Pts',(17.071033847921,8.40379607744266,0.));
#37069=CARTESIAN_POINT('Ctrl Pts',(17.071033847921,8.40379607744266,18.));
#37070=CARTESIAN_POINT('Ctrl Pts',(17.1337886602855,8.45135198307876,0.));
#37071=CARTESIAN_POINT('Ctrl Pts',(17.1337886602855,8.45135198307876,18.));
#37072=CARTESIAN_POINT('Ctrl Pts',(17.1956428575086,8.50048099003882,0.));
#37073=CARTESIAN_POINT('Ctrl Pts',(17.1956428575086,8.50048099003882,18.));
#37074=CARTESIAN_POINT('Ctrl Pts',(17.2570167183611,8.55046295192433,0.));
#37075=CARTESIAN_POINT('Ctrl Pts',(17.2570167183611,8.55046295192433,18.));
#37076=CARTESIAN_POINT('Ctrl Pts',(17.3180459442745,8.60104338529165,0.));
#37077=CARTESIAN_POINT('Ctrl Pts',(17.3180459442745,8.60104338529165,18.));
#37078=CARTESIAN_POINT('Ctrl Pts',(17.3786861166843,8.65226368112816,0.));
#37079=CARTESIAN_POINT('Ctrl Pts',(17.3786861166843,8.65226368112816,18.));
#37080=CARTESIAN_POINT('Ctrl Pts',(17.438788019753,8.70433925112174,0.));
#37081=CARTESIAN_POINT('Ctrl Pts',(17.438788019753,8.70433925112174,18.));
#37082=CARTESIAN_POINT('Ctrl Pts',(17.4981785296199,8.75752832625954,0.));
#37083=CARTESIAN_POINT('Ctrl Pts',(17.4981785296199,8.75752832625954,18.));
#37084=CARTESIAN_POINT('Ctrl Pts',(17.5567525798882,8.8119830723955,0.));
#37085=CARTESIAN_POINT('Ctrl Pts',(17.5567525798882,8.8119830723955,18.));
#37086=CARTESIAN_POINT('Ctrl Pts',(17.614513388992,8.86768402115343,0.));
#37087=CARTESIAN_POINT('Ctrl Pts',(17.614513388992,8.86768402115343,18.));
#37088=CARTESIAN_POINT('Ctrl Pts',(17.6715250120654,8.92451585185175,0.));
#37089=CARTESIAN_POINT('Ctrl Pts',(17.6715250120654,8.92451585185175,18.));
#37090=CARTESIAN_POINT('Ctrl Pts',(17.7278841963319,8.98231202490685,0.));
#37091=CARTESIAN_POINT('Ctrl Pts',(17.7278841963319,8.98231202490685,18.));
#37092=CARTESIAN_POINT('Ctrl Pts',(17.7836872744016,9.04090748239097,0.));
#37093=CARTESIAN_POINT('Ctrl Pts',(17.7836872744016,9.04090748239097,18.));
#37094=CARTESIAN_POINT('Ctrl Pts',(17.8389924349283,9.10019864472208,0.));
#37095=CARTESIAN_POINT('Ctrl Pts',(17.8389924349283,9.10019864472208,18.));
#37096=CARTESIAN_POINT('Ctrl Pts',(17.8938116696237,9.16015616361609,0.));
#37097=CARTESIAN_POINT('Ctrl Pts',(17.8938116696237,9.16015616361609,18.));
#37098=CARTESIAN_POINT('Ctrl Pts',(17.9481305624284,9.22079331175917,0.));
#37099=CARTESIAN_POINT('Ctrl Pts',(17.9481305624284,9.22079331175917,18.));
#37100=CARTESIAN_POINT('Ctrl Pts',(18.0019206847747,9.2821461557447,0.));
#37101=CARTESIAN_POINT('Ctrl Pts',(18.0019206847747,9.2821461557447,18.));
#37102=CARTESIAN_POINT('Ctrl Pts',(18.0551538338035,9.34425079614396,0.));
#37103=CARTESIAN_POINT('Ctrl Pts',(18.0551538338035,9.34425079614396,18.));
#37104=CARTESIAN_POINT('Ctrl Pts',(18.1078184146735,9.40711718355464,0.));
#37105=CARTESIAN_POINT('Ctrl Pts',(18.1078184146735,9.40711718355464,18.));
#37106=CARTESIAN_POINT('Ctrl Pts',(18.1599204445014,9.47072748065831,0.));
#37107=CARTESIAN_POINT('Ctrl Pts',(18.1599204445014,9.47072748065831,18.));
#37108=CARTESIAN_POINT('Ctrl Pts',(18.2114756946126,9.53504856811685,0.));
#37109=CARTESIAN_POINT('Ctrl Pts',(18.2114756946126,9.53504856811685,18.));
#37110=CARTESIAN_POINT('Ctrl Pts',(18.2625044208165,9.60004042085347,0.));
#37111=CARTESIAN_POINT('Ctrl Pts',(18.2625044208165,9.60004042085347,18.));
#37112=CARTESIAN_POINT('Ctrl Pts',(18.3130254811852,9.66566546403259,0.));
#37113=CARTESIAN_POINT('Ctrl Pts',(18.3130254811852,9.66566546403259,18.));
#37114=CARTESIAN_POINT('Ctrl Pts',(18.3630495772677,9.73189932619939,0.));
#37115=CARTESIAN_POINT('Ctrl Pts',(18.3630495772677,9.73189932619939,18.));
#37116=CARTESIAN_POINT('Ctrl Pts',(18.4125796444662,9.79873019947433,0.));
#37117=CARTESIAN_POINT('Ctrl Pts',(18.4125796444662,9.79873019947433,18.));
#37118=CARTESIAN_POINT('Ctrl Pts',(18.461614050347,9.86615372541684,0.));
#37119=CARTESIAN_POINT('Ctrl Pts',(18.461614050347,9.86615372541684,18.));
#37120=CARTESIAN_POINT('Ctrl Pts',(18.5101489409161,9.93416923996828,0.));
#37121=CARTESIAN_POINT('Ctrl Pts',(18.5101489409161,9.93416923996828,18.));
#37122=CARTESIAN_POINT('Ctrl Pts',(18.5581807679204,10.0027757313807,0.));
#37123=CARTESIAN_POINT('Ctrl Pts',(18.5581807679204,10.0027757313807,18.));
#37124=CARTESIAN_POINT('Ctrl Pts',(18.605709190442,10.0719672018851,0.));
#37125=CARTESIAN_POINT('Ctrl Pts',(18.605709190442,10.0719672018851,18.));
#37126=CARTESIAN_POINT('Ctrl Pts',(18.6527367592664,10.1417331637795,0.));
#37127=CARTESIAN_POINT('Ctrl Pts',(18.6527367592664,10.1417331637795,18.));
#37128=CARTESIAN_POINT('Ctrl Pts',(18.699267629819,10.2120606864872,0.));
#37129=CARTESIAN_POINT('Ctrl Pts',(18.699267629819,10.2120606864872,18.));
#37130=CARTESIAN_POINT('Ctrl Pts',(18.7453065790062,10.2829359603685,0.));
#37131=CARTESIAN_POINT('Ctrl Pts',(18.7453065790062,10.2829359603685,18.));
#37132=CARTESIAN_POINT('Ctrl Pts',(18.7908579693851,10.3543459451258,0.));
#37133=CARTESIAN_POINT('Ctrl Pts',(18.7908579693851,10.3543459451258,18.));
#37134=CARTESIAN_POINT('Ctrl Pts',(18.8359245594214,10.4262802670211,0.));
#37135=CARTESIAN_POINT('Ctrl Pts',(18.8359245594214,10.4262802670211,18.));
#37136=CARTESIAN_POINT('Ctrl Pts',(18.8805076729356,10.4987309368494,0.));
#37137=CARTESIAN_POINT('Ctrl Pts',(18.8805076729356,10.4987309368494,18.));
#37138=CARTESIAN_POINT('Ctrl Pts',(18.9246077453188,10.5716914651544,0.));
#37139=CARTESIAN_POINT('Ctrl Pts',(18.9246077453188,10.5716914651544,18.));
#37140=CARTESIAN_POINT('Ctrl Pts',(18.9682247574834,10.6451561585969,0.));
#37141=CARTESIAN_POINT('Ctrl Pts',(18.9682247574834,10.6451561585969,18.));
#37142=CARTESIAN_POINT('Ctrl Pts',(19.0113586878152,10.7191193896586,0.));
#37143=CARTESIAN_POINT('Ctrl Pts',(19.0113586878152,10.7191193896586,18.));
#37144=CARTESIAN_POINT('Ctrl Pts',(19.0540100416943,10.7935747414879,0.));
#37145=CARTESIAN_POINT('Ctrl Pts',(19.0540100416943,10.7935747414879,18.));
#37146=CARTESIAN_POINT('Ctrl Pts',(19.0961797996403,10.868515097783,0.));
#37147=CARTESIAN_POINT('Ctrl Pts',(19.0961797996403,10.868515097783,18.));
#37148=CARTESIAN_POINT('Ctrl Pts',(19.1378691901023,10.9439330179206,0.));
#37149=CARTESIAN_POINT('Ctrl Pts',(19.1378691901023,10.9439330179206,18.));
#37150=CARTESIAN_POINT('Ctrl Pts',(19.1790795192393,11.0198210228993,0.));
#37151=CARTESIAN_POINT('Ctrl Pts',(19.1790795192393,11.0198210228993,18.));
#37152=CARTESIAN_POINT('Ctrl Pts',(19.2198119937835,11.0961718903994,0.));
#37153=CARTESIAN_POINT('Ctrl Pts',(19.2198119937835,11.0961718903994,18.));
#37154=CARTESIAN_POINT('Ctrl Pts',(19.2600675167206,11.1729790050543,0.));
#37155=CARTESIAN_POINT('Ctrl Pts',(19.2600675167206,11.1729790050543,18.));
#37156=CARTESIAN_POINT('Ctrl Pts',(19.2998466936739,11.2502363198588,0.));
#37157=CARTESIAN_POINT('Ctrl Pts',(19.2998466936739,11.2502363198588,18.));
#37158=CARTESIAN_POINT('Ctrl Pts',(19.3391499248083,11.3279381634523,0.));
#37159=CARTESIAN_POINT('Ctrl Pts',(19.3391499248083,11.3279381634523,18.));
#37160=CARTESIAN_POINT('Ctrl Pts',(19.3779774742876,11.4060790880015,0.));
#37161=CARTESIAN_POINT('Ctrl Pts',(19.3779774742876,11.4060790880015,18.));
#37162=CARTESIAN_POINT('Ctrl Pts',(19.4163295466324,11.4846537135043,0.));
#37163=CARTESIAN_POINT('Ctrl Pts',(19.4163295466324,11.4846537135043,18.));
#37164=CARTESIAN_POINT('Ctrl Pts',(19.4542063779876,11.5636565297382,0.));
#37165=CARTESIAN_POINT('Ctrl Pts',(19.4542063779876,11.5636565297382,18.));
#37166=CARTESIAN_POINT('Ctrl Pts',(19.4916082541529,11.6430819099846,0.));
#37167=CARTESIAN_POINT('Ctrl Pts',(19.4916082541529,11.6430819099846,18.));
#37168=CARTESIAN_POINT('Ctrl Pts',(19.5285354853626,11.722924244195,0.));
#37169=CARTESIAN_POINT('Ctrl Pts',(19.5285354853626,11.722924244195,18.));
#37170=CARTESIAN_POINT('Ctrl Pts',(19.5649883985826,11.8031780389346,0.));
#37171=CARTESIAN_POINT('Ctrl Pts',(19.5649883985826,11.8031780389346,18.));
#37172=CARTESIAN_POINT('Ctrl Pts',(19.6009673241771,11.8838380136222,0.));
#37173=CARTESIAN_POINT('Ctrl Pts',(19.6009673241771,11.8838380136222,18.));
#37174=CARTESIAN_POINT('Ctrl Pts',(19.6364725931695,11.9648992312094,0.));
#37175=CARTESIAN_POINT('Ctrl Pts',(19.6364725931695,11.9648992312094,18.));
#37176=CARTESIAN_POINT('Ctrl Pts',(19.6715045149944,12.0463570680308,0.));
#37177=CARTESIAN_POINT('Ctrl Pts',(19.6715045149944,12.0463570680308,18.));
#37178=CARTESIAN_POINT('Ctrl Pts',(19.7060633406705,12.1282070378972,0.));
#37179=CARTESIAN_POINT('Ctrl Pts',(19.7060633406705,12.1282070378972,18.));
#37180=CARTESIAN_POINT('Ctrl Pts',(19.7401492304335,12.2104446447874,0.));
#37181=CARTESIAN_POINT('Ctrl Pts',(19.7401492304335,12.2104446447874,18.));
#37182=CARTESIAN_POINT('Ctrl Pts',(19.7737622285562,12.2930652417986,0.));
#37183=CARTESIAN_POINT('Ctrl Pts',(19.7737622285562,12.2930652417986,18.));
#37184=CARTESIAN_POINT('Ctrl Pts',(19.8069022248387,12.3760638341708,0.));
#37185=CARTESIAN_POINT('Ctrl Pts',(19.8069022248387,12.3760638341708,18.));
#37186=CARTESIAN_POINT('Ctrl Pts',(19.839568972011,12.4594350764989,0.));
#37187=CARTESIAN_POINT('Ctrl Pts',(19.839568972011,12.4594350764989,18.));
#37188=CARTESIAN_POINT('Ctrl Pts',(19.8717621942733,12.5431736030595,0.));
#37189=CARTESIAN_POINT('Ctrl Pts',(19.8717621942733,12.5431736030595,18.));
#37190=CARTESIAN_POINT('Ctrl Pts',(19.9034816813503,12.6272742843372,0.));
#37191=CARTESIAN_POINT('Ctrl Pts',(19.9034816813503,12.6272742843372,18.));
#37192=CARTESIAN_POINT('Ctrl Pts',(19.9347273847264,12.7117325003719,0.));
#37193=CARTESIAN_POINT('Ctrl Pts',(19.9347273847264,12.7117325003719,18.));
#37194=CARTESIAN_POINT('Ctrl Pts',(19.9654995335894,12.7965444294443,0.));
#37195=CARTESIAN_POINT('Ctrl Pts',(19.9654995335894,12.7965444294443,18.));
#37196=CARTESIAN_POINT('Ctrl Pts',(19.9957986945787,12.8817072534696,0.));
#37197=CARTESIAN_POINT('Ctrl Pts',(19.9957986945787,12.8817072534696,18.));
#37198=CARTESIAN_POINT('Ctrl Pts',(20.0256255826397,12.9672189949731,0.));
#37199=CARTESIAN_POINT('Ctrl Pts',(20.0256255826397,12.9672189949731,18.));
#37200=CARTESIAN_POINT('Ctrl Pts',(20.0491098457044,13.0359065249991,0.));
#37201=CARTESIAN_POINT('Ctrl Pts',(20.0491098457044,13.0359065249991,18.));
#37202=CARTESIAN_POINT('Ctrl Pts',(20.0665110891946,13.0875783330728,0.));
#37203=CARTESIAN_POINT('Ctrl Pts',(20.0665110891946,13.0875783330728,18.));
#37204=CARTESIAN_POINT('Ctrl Pts',(20.0780177478283,13.1220955868173,0.));
#37205=CARTESIAN_POINT('Ctrl Pts',(20.0780177478283,13.1220955868173,18.));
#37206=CARTESIAN_POINT('Ctrl Pts',(20.0837475345526,13.1393715591102,0.));
#37207=CARTESIAN_POINT('Ctrl Pts',(20.0837475345526,13.1393715591102,18.));
#37208=CARTESIAN_POINT('Ctrl Pts',(16.8707481591095,8.28171148831561,0.));
#37209=CARTESIAN_POINT('Ctrl Pts',(16.8848228151885,8.28862062120315,0.));
#37210=CARTESIAN_POINT('Ctrl Pts',(16.9126979078877,8.30290517019115,0.));
#37211=CARTESIAN_POINT('Ctrl Pts',(16.9536879065132,8.32573081382562,0.));
#37212=CARTESIAN_POINT('Ctrl Pts',(17.0067806259695,8.35882146841243,0.));
#37213=CARTESIAN_POINT('Ctrl Pts',(17.071033847921,8.40379607744266,0.));
#37214=CARTESIAN_POINT('Ctrl Pts',(17.1337886602855,8.45135198307876,0.));
#37215=CARTESIAN_POINT('Ctrl Pts',(17.1956428575086,8.50048099003882,0.));
#37216=CARTESIAN_POINT('Ctrl Pts',(17.2570167183611,8.55046295192433,0.));
#37217=CARTESIAN_POINT('Ctrl Pts',(17.3180459442745,8.60104338529165,0.));
#37218=CARTESIAN_POINT('Ctrl Pts',(17.3786861166843,8.65226368112816,0.));
#37219=CARTESIAN_POINT('Ctrl Pts',(17.438788019753,8.70433925112174,0.));
#37220=CARTESIAN_POINT('Ctrl Pts',(17.4981785296199,8.75752832625954,0.));
#37221=CARTESIAN_POINT('Ctrl Pts',(17.5567525798882,8.8119830723955,0.));
#37222=CARTESIAN_POINT('Ctrl Pts',(17.614513388992,8.86768402115343,0.));
#37223=CARTESIAN_POINT('Ctrl Pts',(17.6715250120654,8.92451585185175,0.));
#37224=CARTESIAN_POINT('Ctrl Pts',(17.7278841963319,8.98231202490685,0.));
#37225=CARTESIAN_POINT('Ctrl Pts',(17.7836872744016,9.04090748239097,0.));
#37226=CARTESIAN_POINT('Ctrl Pts',(17.8389924349283,9.10019864472208,0.));
#37227=CARTESIAN_POINT('Ctrl Pts',(17.8938116696237,9.16015616361609,0.));
#37228=CARTESIAN_POINT('Ctrl Pts',(17.9481305624284,9.22079331175917,0.));
#37229=CARTESIAN_POINT('Ctrl Pts',(18.0019206847747,9.2821461557447,0.));
#37230=CARTESIAN_POINT('Ctrl Pts',(18.0551538338035,9.34425079614396,0.));
#37231=CARTESIAN_POINT('Ctrl Pts',(18.1078184146735,9.40711718355464,0.));
#37232=CARTESIAN_POINT('Ctrl Pts',(18.1599204445014,9.47072748065831,0.));
#37233=CARTESIAN_POINT('Ctrl Pts',(18.2114756946126,9.53504856811685,0.));
#37234=CARTESIAN_POINT('Ctrl Pts',(18.2625044208165,9.60004042085347,0.));
#37235=CARTESIAN_POINT('Ctrl Pts',(18.3130254811852,9.66566546403259,0.));
#37236=CARTESIAN_POINT('Ctrl Pts',(18.3630495772677,9.73189932619939,0.));
#37237=CARTESIAN_POINT('Ctrl Pts',(18.4125796444662,9.79873019947433,0.));
#37238=CARTESIAN_POINT('Ctrl Pts',(18.461614050347,9.86615372541684,0.));
#37239=CARTESIAN_POINT('Ctrl Pts',(18.5101489409161,9.93416923996828,0.));
#37240=CARTESIAN_POINT('Ctrl Pts',(18.5581807679204,10.0027757313807,0.));
#37241=CARTESIAN_POINT('Ctrl Pts',(18.605709190442,10.0719672018851,0.));
#37242=CARTESIAN_POINT('Ctrl Pts',(18.6527367592664,10.1417331637795,0.));
#37243=CARTESIAN_POINT('Ctrl Pts',(18.699267629819,10.2120606864872,0.));
#37244=CARTESIAN_POINT('Ctrl Pts',(18.7453065790062,10.2829359603685,0.));
#37245=CARTESIAN_POINT('Ctrl Pts',(18.7908579693851,10.3543459451258,0.));
#37246=CARTESIAN_POINT('Ctrl Pts',(18.8359245594214,10.4262802670211,0.));
#37247=CARTESIAN_POINT('Ctrl Pts',(18.8805076729356,10.4987309368494,0.));
#37248=CARTESIAN_POINT('Ctrl Pts',(18.9246077453188,10.5716914651544,0.));
#37249=CARTESIAN_POINT('Ctrl Pts',(18.9682247574834,10.6451561585969,0.));
#37250=CARTESIAN_POINT('Ctrl Pts',(19.0113586878152,10.7191193896586,0.));
#37251=CARTESIAN_POINT('Ctrl Pts',(19.0540100416943,10.7935747414879,0.));
#37252=CARTESIAN_POINT('Ctrl Pts',(19.0961797996403,10.868515097783,0.));
#37253=CARTESIAN_POINT('Ctrl Pts',(19.1378691901023,10.9439330179206,0.));
#37254=CARTESIAN_POINT('Ctrl Pts',(19.1790795192393,11.0198210228993,0.));
#37255=CARTESIAN_POINT('Ctrl Pts',(19.2198119937835,11.0961718903994,0.));
#37256=CARTESIAN_POINT('Ctrl Pts',(19.2600675167206,11.1729790050543,0.));
#37257=CARTESIAN_POINT('Ctrl Pts',(19.2998466936739,11.2502363198588,0.));
#37258=CARTESIAN_POINT('Ctrl Pts',(19.3391499248083,11.3279381634523,0.));
#37259=CARTESIAN_POINT('Ctrl Pts',(19.3779774742876,11.4060790880015,0.));
#37260=CARTESIAN_POINT('Ctrl Pts',(19.4163295466324,11.4846537135043,0.));
#37261=CARTESIAN_POINT('Ctrl Pts',(19.4542063779876,11.5636565297382,0.));
#37262=CARTESIAN_POINT('Ctrl Pts',(19.4916082541529,11.6430819099846,0.));
#37263=CARTESIAN_POINT('Ctrl Pts',(19.5285354853626,11.722924244195,0.));
#37264=CARTESIAN_POINT('Ctrl Pts',(19.5649883985826,11.8031780389346,0.));
#37265=CARTESIAN_POINT('Ctrl Pts',(19.6009673241771,11.8838380136222,0.));
#37266=CARTESIAN_POINT('Ctrl Pts',(19.6364725931695,11.9648992312094,0.));
#37267=CARTESIAN_POINT('Ctrl Pts',(19.6715045149944,12.0463570680308,0.));
#37268=CARTESIAN_POINT('Ctrl Pts',(19.7060633406705,12.1282070378972,0.));
#37269=CARTESIAN_POINT('Ctrl Pts',(19.7401492304335,12.2104446447874,0.));
#37270=CARTESIAN_POINT('Ctrl Pts',(19.7737622285562,12.2930652417986,0.));
#37271=CARTESIAN_POINT('Ctrl Pts',(19.8069022248387,12.3760638341708,0.));
#37272=CARTESIAN_POINT('Ctrl Pts',(19.839568972011,12.4594350764989,0.));
#37273=CARTESIAN_POINT('Ctrl Pts',(19.8717621942733,12.5431736030595,0.));
#37274=CARTESIAN_POINT('Ctrl Pts',(19.9034816813503,12.6272742843372,0.));
#37275=CARTESIAN_POINT('Ctrl Pts',(19.9347273847264,12.7117325003719,0.));
#37276=CARTESIAN_POINT('Ctrl Pts',(19.9654995335894,12.7965444294443,0.));
#37277=CARTESIAN_POINT('Ctrl Pts',(20.0018585267766,12.8987398182747,0.));
#37278=CARTESIAN_POINT('Ctrl Pts',(20.0315673466055,12.9843387891477,0.));
#37279=CARTESIAN_POINT('Ctrl Pts',(20.054957345404,13.0530957702829,0.));
#37280=CARTESIAN_POINT('Ctrl Pts',(20.0722879610899,13.1048196144678,0.));
#37281=CARTESIAN_POINT('Ctrl Pts',(20.0837475345526,13.1393715591102,0.));
#37282=CARTESIAN_POINT('Ctrl Pts',(16.8707481591095,8.28171148831561,15.));
#37283=CARTESIAN_POINT('Ctrl Pts',(16.8848228151885,8.28862062120315,15.));
#37284=CARTESIAN_POINT('Ctrl Pts',(16.9126979078877,8.30290517019115,15.));
#37285=CARTESIAN_POINT('Ctrl Pts',(16.9536879065132,8.32573081382562,15.));
#37286=CARTESIAN_POINT('Ctrl Pts',(17.0067806259695,8.35882146841243,15.));
#37287=CARTESIAN_POINT('Ctrl Pts',(17.071033847921,8.40379607744266,15.));
#37288=CARTESIAN_POINT('Ctrl Pts',(17.1337886602855,8.45135198307876,15.));
#37289=CARTESIAN_POINT('Ctrl Pts',(17.1956428575086,8.50048099003882,15.));
#37290=CARTESIAN_POINT('Ctrl Pts',(17.2570167183611,8.55046295192433,15.));
#37291=CARTESIAN_POINT('Ctrl Pts',(17.3180459442745,8.60104338529165,15.));
#37292=CARTESIAN_POINT('Ctrl Pts',(17.3786861166843,8.65226368112816,15.));
#37293=CARTESIAN_POINT('Ctrl Pts',(17.438788019753,8.70433925112174,15.));
#37294=CARTESIAN_POINT('Ctrl Pts',(17.4981785296199,8.75752832625954,15.));
#37295=CARTESIAN_POINT('Ctrl Pts',(17.5567525798882,8.8119830723955,15.));
#37296=CARTESIAN_POINT('Ctrl Pts',(17.614513388992,8.86768402115343,15.));
#37297=CARTESIAN_POINT('Ctrl Pts',(17.6715250120654,8.92451585185175,15.));
#37298=CARTESIAN_POINT('Ctrl Pts',(17.7278841963319,8.98231202490685,15.));
#37299=CARTESIAN_POINT('Ctrl Pts',(17.7836872744016,9.04090748239097,15.));
#37300=CARTESIAN_POINT('Ctrl Pts',(17.8389924349283,9.10019864472208,15.));
#37301=CARTESIAN_POINT('Ctrl Pts',(17.8938116696237,9.16015616361609,15.));
#37302=CARTESIAN_POINT('Ctrl Pts',(17.9481305624284,9.22079331175917,15.));
#37303=CARTESIAN_POINT('Ctrl Pts',(18.0019206847747,9.2821461557447,15.));
#37304=CARTESIAN_POINT('Ctrl Pts',(18.0551538338035,9.34425079614396,15.));
#37305=CARTESIAN_POINT('Ctrl Pts',(18.1078184146735,9.40711718355464,15.));
#37306=CARTESIAN_POINT('Ctrl Pts',(18.1599204445014,9.47072748065831,15.));
#37307=CARTESIAN_POINT('Ctrl Pts',(18.2114756946126,9.53504856811685,15.));
#37308=CARTESIAN_POINT('Ctrl Pts',(18.2625044208165,9.60004042085347,15.));
#37309=CARTESIAN_POINT('Ctrl Pts',(18.3130254811852,9.66566546403259,15.));
#37310=CARTESIAN_POINT('Ctrl Pts',(18.3630495772677,9.73189932619939,15.));
#37311=CARTESIAN_POINT('Ctrl Pts',(18.4125796444662,9.79873019947433,15.));
#37312=CARTESIAN_POINT('Ctrl Pts',(18.461614050347,9.86615372541684,15.));
#37313=CARTESIAN_POINT('Ctrl Pts',(18.5101489409161,9.93416923996828,15.));
#37314=CARTESIAN_POINT('Ctrl Pts',(18.5581807679204,10.0027757313807,15.));
#37315=CARTESIAN_POINT('Ctrl Pts',(18.605709190442,10.0719672018851,15.));
#37316=CARTESIAN_POINT('Ctrl Pts',(18.6527367592664,10.1417331637795,15.));
#37317=CARTESIAN_POINT('Ctrl Pts',(18.699267629819,10.2120606864872,15.));
#37318=CARTESIAN_POINT('Ctrl Pts',(18.7453065790062,10.2829359603685,15.));
#37319=CARTESIAN_POINT('Ctrl Pts',(18.7908579693851,10.3543459451258,15.));
#37320=CARTESIAN_POINT('Ctrl Pts',(18.8359245594214,10.4262802670211,15.));
#37321=CARTESIAN_POINT('Ctrl Pts',(18.8805076729356,10.4987309368494,15.));
#37322=CARTESIAN_POINT('Ctrl Pts',(18.9246077453188,10.5716914651544,15.));
#37323=CARTESIAN_POINT('Ctrl Pts',(18.9682247574834,10.6451561585969,15.));
#37324=CARTESIAN_POINT('Ctrl Pts',(19.0113586878152,10.7191193896586,15.));
#37325=CARTESIAN_POINT('Ctrl Pts',(19.0540100416943,10.7935747414879,15.));
#37326=CARTESIAN_POINT('Ctrl Pts',(19.0961797996403,10.868515097783,15.));
#37327=CARTESIAN_POINT('Ctrl Pts',(19.1378691901023,10.9439330179206,15.));
#37328=CARTESIAN_POINT('Ctrl Pts',(19.1790795192393,11.0198210228993,15.));
#37329=CARTESIAN_POINT('Ctrl Pts',(19.2198119937835,11.0961718903994,15.));
#37330=CARTESIAN_POINT('Ctrl Pts',(19.2600675167206,11.1729790050543,15.));
#37331=CARTESIAN_POINT('Ctrl Pts',(19.2998466936739,11.2502363198588,15.));
#37332=CARTESIAN_POINT('Ctrl Pts',(19.3391499248083,11.3279381634523,15.));
#37333=CARTESIAN_POINT('Ctrl Pts',(19.3779774742876,11.4060790880015,15.));
#37334=CARTESIAN_POINT('Ctrl Pts',(19.4163295466324,11.4846537135043,15.));
#37335=CARTESIAN_POINT('Ctrl Pts',(19.4542063779876,11.5636565297382,15.));
#37336=CARTESIAN_POINT('Ctrl Pts',(19.4916082541529,11.6430819099846,15.));
#37337=CARTESIAN_POINT('Ctrl Pts',(19.5285354853626,11.722924244195,15.));
#37338=CARTESIAN_POINT('Ctrl Pts',(19.5649883985826,11.8031780389346,15.));
#37339=CARTESIAN_POINT('Ctrl Pts',(19.6009673241771,11.8838380136222,15.));
#37340=CARTESIAN_POINT('Ctrl Pts',(19.6364725931695,11.9648992312094,15.));
#37341=CARTESIAN_POINT('Ctrl Pts',(19.6715045149944,12.0463570680308,15.));
#37342=CARTESIAN_POINT('Ctrl Pts',(19.7060633406705,12.1282070378972,15.));
#37343=CARTESIAN_POINT('Ctrl Pts',(19.7401492304335,12.2104446447874,15.));
#37344=CARTESIAN_POINT('Ctrl Pts',(19.7737622285562,12.2930652417986,15.));
#37345=CARTESIAN_POINT('Ctrl Pts',(19.8069022248387,12.3760638341708,15.));
#37346=CARTESIAN_POINT('Ctrl Pts',(19.839568972011,12.4594350764989,15.));
#37347=CARTESIAN_POINT('Ctrl Pts',(19.8717621942733,12.5431736030595,15.));
#37348=CARTESIAN_POINT('Ctrl Pts',(19.9034816813503,12.6272742843372,15.));
#37349=CARTESIAN_POINT('Ctrl Pts',(19.9347273847264,12.7117325003719,15.));
#37350=CARTESIAN_POINT('Ctrl Pts',(19.9654995335894,12.7965444294443,15.));
#37351=CARTESIAN_POINT('Ctrl Pts',(20.0018585267766,12.8987398182747,15.));
#37352=CARTESIAN_POINT('Ctrl Pts',(20.0315673466055,12.9843387891477,15.));
#37353=CARTESIAN_POINT('Ctrl Pts',(20.054957345404,13.0530957702829,15.));
#37354=CARTESIAN_POINT('Ctrl Pts',(20.0722879610899,13.1048196144678,15.));
#37355=CARTESIAN_POINT('Ctrl Pts',(20.0837475345526,13.1393715591102,15.));
#37356=CARTESIAN_POINT('Origin',(0.,0.,0.));
#37357=CARTESIAN_POINT('Origin',(0.,0.,0.));
#37358=CARTESIAN_POINT('Origin',(0.,0.,0.));
#37359=CARTESIAN_POINT('Origin',(0.,0.,0.));
#37360=CARTESIAN_POINT('Origin',(0.,0.,0.));
#37361=CARTESIAN_POINT('Origin',(0.,0.,0.));
#37362=CARTESIAN_POINT('Origin',(0.,0.,0.));
#37363=CARTESIAN_POINT('Origin',(0.,0.,0.));
#37364=CARTESIAN_POINT('',(14.9562571344462,3.5508810918317,0.));
#37365=CARTESIAN_POINT('Origin',(0.,0.,0.));
#37366=CARTESIAN_POINT('',(16.1003491021971,2.79663061332403,0.));
#37367=CARTESIAN_POINT('Origin',(15.9292116709051,3.78187778008512,0.));
#37368=CARTESIAN_POINT('',(18.5165898451125,3.2163316265074,0.));
#37369=CARTESIAN_POINT('',(15.135366975784,2.62901321950806,0.));
#37370=CARTESIAN_POINT('',(23.9712218930251,1.17495572484827,0.));
#37371=CARTESIAN_POINT('Ctrl Pts',(18.5165898451125,3.2163316265074,0.));
#37372=CARTESIAN_POINT('Ctrl Pts',(18.5320375674878,3.2190148958593,0.));
#37373=CARTESIAN_POINT('Ctrl Pts',(18.5629852384321,3.22384302136592,0.));
#37374=CARTESIAN_POINT('Ctrl Pts',(18.6095634206219,3.2294700044416,0.));
#37375=CARTESIAN_POINT('Ctrl Pts',(18.6719665316945,3.23390622002644,0.));
#37376=CARTESIAN_POINT('Ctrl Pts',(18.7503838921122,3.23528809328097,0.));
#37377=CARTESIAN_POINT('Ctrl Pts',(18.8291062617862,3.23370091065669,0.));
#37378=CARTESIAN_POINT('Ctrl Pts',(18.908024664264,3.23031169402939,0.));
#37379=CARTESIAN_POINT('Ctrl Pts',(18.987055820781,3.22595008773715,0.));
#37380=CARTESIAN_POINT('Ctrl Pts',(19.0661599344864,3.22090173651085,0.));
#37381=CARTESIAN_POINT('Ctrl Pts',(19.1453253990185,3.21510704576117,0.));
#37382=CARTESIAN_POINT('Ctrl Pts',(19.2245581120423,3.2083040369031,0.));
#37383=CARTESIAN_POINT('Ctrl Pts',(19.3038697977783,3.2001820370274,0.));
#37384=CARTESIAN_POINT('Ctrl Pts',(19.3832648965708,3.19055618489382,0.));
#37385=CARTESIAN_POINT('Ctrl Pts',(19.4627345689632,3.17944412249754,0.));
#37386=CARTESIAN_POINT('Ctrl Pts',(19.5422628528517,3.16697679689294,0.));
#37387=CARTESIAN_POINT('Ctrl Pts',(19.6218301288731,3.15334580802458,0.));
#37388=CARTESIAN_POINT('Ctrl Pts',(19.7014173131304,3.13874131344865,0.));
#37389=CARTESIAN_POINT('Ctrl Pts',(19.7810105986827,3.1232813132398,0.));
#37390=CARTESIAN_POINT('Ctrl Pts',(19.8606024365399,3.10699659920993,0.));
#37391=CARTESIAN_POINT('Ctrl Pts',(19.9401889653541,3.08986795998319,0.));
#37392=CARTESIAN_POINT('Ctrl Pts',(20.0197683853426,3.07184950717982,0.));
#37393=CARTESIAN_POINT('Ctrl Pts',(20.0993390992966,3.05289545759951,0.));
#37394=CARTESIAN_POINT('Ctrl Pts',(20.178897575607,3.03299094576288,0.));
#37395=CARTESIAN_POINT('Ctrl Pts',(20.2584381977107,3.01215393913612,0.));
#37396=CARTESIAN_POINT('Ctrl Pts',(20.3379542578194,2.99042050197904,0.));
#37397=CARTESIAN_POINT('Ctrl Pts',(20.4174386170774,2.96783492132513,0.));
#37398=CARTESIAN_POINT('Ctrl Pts',(20.4968844460513,2.94443868035154,0.));
#37399=CARTESIAN_POINT('Ctrl Pts',(20.5762860772943,2.92025778619206,0.));
#37400=CARTESIAN_POINT('Ctrl Pts',(20.6556389450993,2.89530351700805,0.));
#37401=CARTESIAN_POINT('Ctrl Pts',(20.7349391669725,2.86957843933153,0.));
#37402=CARTESIAN_POINT('Ctrl Pts',(20.8141832346435,2.84308082507644,0.));
#37403=CARTESIAN_POINT('Ctrl Pts',(20.8933676828246,2.81580940715318,0.));
#37404=CARTESIAN_POINT('Ctrl Pts',(20.9724887103073,2.78776883747222,0.));
#37405=CARTESIAN_POINT('Ctrl Pts',(21.0515422162039,2.7589691000769,0.));
#37406=CARTESIAN_POINT('Ctrl Pts',(21.1305239619219,2.72942309852119,0.));
#37407=CARTESIAN_POINT('Ctrl Pts',(21.2094296949571,2.69914481283353,0.));
#37408=CARTESIAN_POINT('Ctrl Pts',(21.2882552797978,2.668147357083,0.));
#37409=CARTESIAN_POINT('Ctrl Pts',(21.3669968505594,2.6364407451853,0.));
#37410=CARTESIAN_POINT('Ctrl Pts',(21.4456507822983,2.60403221866523,0.));
#37411=CARTESIAN_POINT('Ctrl Pts',(21.5242136128466,2.5709272835198,0.));
#37412=CARTESIAN_POINT('Ctrl Pts',(21.6026819803014,2.53713053453766,0.));
#37413=CARTESIAN_POINT('Ctrl Pts',(21.6810525594039,2.50264651177235,0.));
#37414=CARTESIAN_POINT('Ctrl Pts',(21.7593219872847,2.46748070362075,0.));
#37415=CARTESIAN_POINT('Ctrl Pts',(21.8374868743435,2.43163944362692,0.));
#37416=CARTESIAN_POINT('Ctrl Pts',(21.9155438409279,2.39512947344577,0.));
#37417=CARTESIAN_POINT('Ctrl Pts',(21.9934895476958,2.35795761145761,0.));
#37418=CARTESIAN_POINT('Ctrl Pts',(22.0713207257413,2.32013040994125,0.));
#37419=CARTESIAN_POINT('Ctrl Pts',(22.1490342171802,2.28165375160231,0.));
#37420=CARTESIAN_POINT('Ctrl Pts',(22.2266269576315,2.24253288454712,0.));
#37421=CARTESIAN_POINT('Ctrl Pts',(22.3040959372933,2.20277263221399,0.));
#37422=CARTESIAN_POINT('Ctrl Pts',(22.3814381677224,2.16237755726404,0.));
#37423=CARTESIAN_POINT('Ctrl Pts',(22.4586506520939,2.1213521324248,0.));
#37424=CARTESIAN_POINT('Ctrl Pts',(22.5357303426251,2.07970095436224,0.));
#37425=CARTESIAN_POINT('Ctrl Pts',(22.6126741632309,2.03742874317627,0.));
#37426=CARTESIAN_POINT('Ctrl Pts',(22.6894790673923,1.99454021984253,0.));
#37427=CARTESIAN_POINT('Ctrl Pts',(22.7661420906702,1.95104002082891,0.));
#37428=CARTESIAN_POINT('Ctrl Pts',(22.8426603964871,1.90693261239855,0.));
#37429=CARTESIAN_POINT('Ctrl Pts',(22.9190313507225,1.86222218327819,0.));
#37430=CARTESIAN_POINT('Ctrl Pts',(22.9952524859917,1.81691265597281,0.));
#37431=CARTESIAN_POINT('Ctrl Pts',(23.0713213684573,1.77100780743078,0.));
#37432=CARTESIAN_POINT('Ctrl Pts',(23.1472354850579,1.72451136919382,0.));
#37433=CARTESIAN_POINT('Ctrl Pts',(23.2229921402299,1.67742712670823,0.));
#37434=CARTESIAN_POINT('Ctrl Pts',(23.2985883089733,1.62975905604583,0.));
#37435=CARTESIAN_POINT('Ctrl Pts',(23.3740206492924,1.58151133638847,0.));
#37436=CARTESIAN_POINT('Ctrl Pts',(23.4492857841673,1.53268814658653,0.));
#37437=CARTESIAN_POINT('Ctrl Pts',(23.5243805284282,1.48329351290851,0.));
#37438=CARTESIAN_POINT('Ctrl Pts',(23.5993021272808,1.4333311444639,0.));
#37439=CARTESIAN_POINT('Ctrl Pts',(23.6740485197917,1.38280426780156,0.));
#37440=CARTESIAN_POINT('Ctrl Pts',(23.7635325055853,1.32149774147467,0.));
#37441=CARTESIAN_POINT('Ctrl Pts',(23.8378812584003,1.2697091254959,0.));
#37442=CARTESIAN_POINT('Ctrl Pts',(23.89721850443,1.22783185562043,0.));
#37443=CARTESIAN_POINT('Ctrl Pts',(23.9416417798466,1.19617306697386,0.));
#37444=CARTESIAN_POINT('Ctrl Pts',(23.9712218930251,1.17495572484832,0.));
#37445=CARTESIAN_POINT('',(23.9712218930251,-1.17495572484832,0.));
#37446=CARTESIAN_POINT('Origin',(1.15463194561016E-13,-6.93889390390723E-17,
0.));
#37447=CARTESIAN_POINT('',(18.5165898451125,-3.2163316265074,0.));
#37448=CARTESIAN_POINT('Ctrl Pts',(18.5165898451125,-3.2163316265074,0.));
#37449=CARTESIAN_POINT('Ctrl Pts',(18.5320375674878,-3.2190148958593,0.));
#37450=CARTESIAN_POINT('Ctrl Pts',(18.5629852384321,-3.22384302136592,0.));
#37451=CARTESIAN_POINT('Ctrl Pts',(18.6095634206219,-3.2294700044416,0.));
#37452=CARTESIAN_POINT('Ctrl Pts',(18.6719665316945,-3.23390622002644,0.));
#37453=CARTESIAN_POINT('Ctrl Pts',(18.7503838921122,-3.23528809328097,0.));
#37454=CARTESIAN_POINT('Ctrl Pts',(18.8291062617862,-3.23370091065669,0.));
#37455=CARTESIAN_POINT('Ctrl Pts',(18.908024664264,-3.23031169402939,0.));
#37456=CARTESIAN_POINT('Ctrl Pts',(18.987055820781,-3.22595008773715,0.));
#37457=CARTESIAN_POINT('Ctrl Pts',(19.0661599344864,-3.22090173651085,0.));
#37458=CARTESIAN_POINT('Ctrl Pts',(19.1453253990185,-3.21510704576117,0.));
#37459=CARTESIAN_POINT('Ctrl Pts',(19.2245581120423,-3.2083040369031,0.));
#37460=CARTESIAN_POINT('Ctrl Pts',(19.3038697977783,-3.2001820370274,0.));
#37461=CARTESIAN_POINT('Ctrl Pts',(19.3832648965708,-3.19055618489382,0.));
#37462=CARTESIAN_POINT('Ctrl Pts',(19.4627345689632,-3.17944412249754,0.));
#37463=CARTESIAN_POINT('Ctrl Pts',(19.5422628528517,-3.16697679689294,0.));
#37464=CARTESIAN_POINT('Ctrl Pts',(19.6218301288731,-3.15334580802458,0.));
#37465=CARTESIAN_POINT('Ctrl Pts',(19.7014173131304,-3.13874131344865,0.));
#37466=CARTESIAN_POINT('Ctrl Pts',(19.7810105986827,-3.1232813132398,0.));
#37467=CARTESIAN_POINT('Ctrl Pts',(19.8606024365399,-3.10699659920993,0.));
#37468=CARTESIAN_POINT('Ctrl Pts',(19.9401889653541,-3.08986795998319,0.));
#37469=CARTESIAN_POINT('Ctrl Pts',(20.0197683853426,-3.07184950717982,0.));
#37470=CARTESIAN_POINT('Ctrl Pts',(20.0993390992966,-3.05289545759951,0.));
#37471=CARTESIAN_POINT('Ctrl Pts',(20.178897575607,-3.03299094576288,0.));
#37472=CARTESIAN_POINT('Ctrl Pts',(20.2584381977107,-3.01215393913612,0.));
#37473=CARTESIAN_POINT('Ctrl Pts',(20.3379542578194,-2.99042050197904,0.));
#37474=CARTESIAN_POINT('Ctrl Pts',(20.4174386170774,-2.96783492132513,0.));
#37475=CARTESIAN_POINT('Ctrl Pts',(20.4968844460513,-2.94443868035154,0.));
#37476=CARTESIAN_POINT('Ctrl Pts',(20.5762860772943,-2.92025778619206,0.));
#37477=CARTESIAN_POINT('Ctrl Pts',(20.6556389450993,-2.89530351700805,0.));
#37478=CARTESIAN_POINT('Ctrl Pts',(20.7349391669725,-2.86957843933153,0.));
#37479=CARTESIAN_POINT('Ctrl Pts',(20.8141832346435,-2.84308082507644,0.));
#37480=CARTESIAN_POINT('Ctrl Pts',(20.8933676828246,-2.81580940715318,0.));
#37481=CARTESIAN_POINT('Ctrl Pts',(20.9724887103073,-2.78776883747222,0.));
#37482=CARTESIAN_POINT('Ctrl Pts',(21.0515422162039,-2.7589691000769,0.));
#37483=CARTESIAN_POINT('Ctrl Pts',(21.1305239619219,-2.72942309852119,0.));
#37484=CARTESIAN_POINT('Ctrl Pts',(21.2094296949571,-2.69914481283353,0.));
#37485=CARTESIAN_POINT('Ctrl Pts',(21.2882552797978,-2.668147357083,0.));
#37486=CARTESIAN_POINT('Ctrl Pts',(21.3669968505594,-2.6364407451853,0.));
#37487=CARTESIAN_POINT('Ctrl Pts',(21.4456507822983,-2.60403221866523,0.));
#37488=CARTESIAN_POINT('Ctrl Pts',(21.5242136128466,-2.5709272835198,0.));
#37489=CARTESIAN_POINT('Ctrl Pts',(21.6026819803014,-2.53713053453766,0.));
#37490=CARTESIAN_POINT('Ctrl Pts',(21.6810525594039,-2.50264651177235,0.));
#37491=CARTESIAN_POINT('Ctrl Pts',(21.7593219872847,-2.46748070362075,0.));
#37492=CARTESIAN_POINT('Ctrl Pts',(21.8374868743435,-2.43163944362692,0.));
#37493=CARTESIAN_POINT('Ctrl Pts',(21.9155438409279,-2.39512947344577,0.));
#37494=CARTESIAN_POINT('Ctrl Pts',(21.9934895476958,-2.35795761145761,0.));
#37495=CARTESIAN_POINT('Ctrl Pts',(22.0713207257413,-2.32013040994125,0.));
#37496=CARTESIAN_POINT('Ctrl Pts',(22.1490342171802,-2.28165375160231,0.));
#37497=CARTESIAN_POINT('Ctrl Pts',(22.2266269576315,-2.24253288454712,0.));
#37498=CARTESIAN_POINT('Ctrl Pts',(22.3040959372933,-2.20277263221399,0.));
#37499=CARTESIAN_POINT('Ctrl Pts',(22.3814381677224,-2.16237755726404,0.));
#37500=CARTESIAN_POINT('Ctrl Pts',(22.4586506520939,-2.1213521324248,0.));
#37501=CARTESIAN_POINT('Ctrl Pts',(22.5357303426251,-2.07970095436224,0.));
#37502=CARTESIAN_POINT('Ctrl Pts',(22.6126741632309,-2.03742874317627,0.));
#37503=CARTESIAN_POINT('Ctrl Pts',(22.6894790673923,-1.99454021984253,0.));
#37504=CARTESIAN_POINT('Ctrl Pts',(22.7661420906702,-1.95104002082891,0.));
#37505=CARTESIAN_POINT('Ctrl Pts',(22.8426603964871,-1.90693261239855,0.));
#37506=CARTESIAN_POINT('Ctrl Pts',(22.9190313507225,-1.86222218327819,0.));
#37507=CARTESIAN_POINT('Ctrl Pts',(22.9952524859917,-1.81691265597281,0.));
#37508=CARTESIAN_POINT('Ctrl Pts',(23.0713213684573,-1.77100780743078,0.));
#37509=CARTESIAN_POINT('Ctrl Pts',(23.1472354850579,-1.72451136919382,0.));
#37510=CARTESIAN_POINT('Ctrl Pts',(23.2229921402299,-1.67742712670823,0.));
#37511=CARTESIAN_POINT('Ctrl Pts',(23.2985883089733,-1.62975905604583,0.));
#37512=CARTESIAN_POINT('Ctrl Pts',(23.3740206492924,-1.58151133638847,0.));
#37513=CARTESIAN_POINT('Ctrl Pts',(23.4492857841673,-1.53268814658653,0.));
#37514=CARTESIAN_POINT('Ctrl Pts',(23.5243805284282,-1.48329351290851,0.));
#37515=CARTESIAN_POINT('Ctrl Pts',(23.5993021272808,-1.4333311444639,0.));
#37516=CARTESIAN_POINT('Ctrl Pts',(23.6740485197917,-1.38280426780156,0.));
#37517=CARTESIAN_POINT('Ctrl Pts',(23.7635325055853,-1.32149774147467,0.));
#37518=CARTESIAN_POINT('Ctrl Pts',(23.8378812584003,-1.2697091254959,0.));
#37519=CARTESIAN_POINT('Ctrl Pts',(23.89721850443,-1.22783185562043,0.));
#37520=CARTESIAN_POINT('Ctrl Pts',(23.9416417798466,-1.19617306697386,0.));
#37521=CARTESIAN_POINT('Ctrl Pts',(23.9712218930251,-1.17495572484832,0.));
#37522=CARTESIAN_POINT('',(16.1003491021971,-2.79663061332403,0.));
#37523=CARTESIAN_POINT('',(15.135366975784,-2.62901321950806,0.));
#37524=CARTESIAN_POINT('',(14.9562571344462,-3.5508810918317,0.));
#37525=CARTESIAN_POINT('Origin',(15.9292116709051,-3.78187778008512,0.));
#37526=CARTESIAN_POINT('Origin',(0.,0.,0.));
#37527=CARTESIAN_POINT('Origin',(0.,0.,0.));
#37528=CARTESIAN_POINT('Origin',(0.,0.,15.));
#37529=CARTESIAN_POINT('',(14.9562571344462,-3.5508810918317,15.));
#37530=CARTESIAN_POINT('Origin',(0.,0.,15.));
#37531=CARTESIAN_POINT('',(16.1003491021971,-2.79663061332403,15.));
#37532=CARTESIAN_POINT('Origin',(15.9292116709051,-3.78187778008512,15.));
#37533=CARTESIAN_POINT('',(18.5165898451125,-3.2163316265074,15.));
#37534=CARTESIAN_POINT('',(15.135366975784,-2.62901321950806,15.));
#37535=CARTESIAN_POINT('',(23.9712218930251,-1.17495572484832,15.));
#37536=CARTESIAN_POINT('Ctrl Pts',(18.5165898451125,-3.2163316265074,15.));
#37537=CARTESIAN_POINT('Ctrl Pts',(18.5320375674878,-3.2190148958593,15.));
#37538=CARTESIAN_POINT('Ctrl Pts',(18.5629852384321,-3.22384302136592,15.));
#37539=CARTESIAN_POINT('Ctrl Pts',(18.6095634206219,-3.2294700044416,15.));
#37540=CARTESIAN_POINT('Ctrl Pts',(18.6719665316945,-3.23390622002644,15.));
#37541=CARTESIAN_POINT('Ctrl Pts',(18.7503838921122,-3.23528809328097,15.));
#37542=CARTESIAN_POINT('Ctrl Pts',(18.8291062617862,-3.23370091065669,15.));
#37543=CARTESIAN_POINT('Ctrl Pts',(18.908024664264,-3.23031169402939,15.));
#37544=CARTESIAN_POINT('Ctrl Pts',(18.987055820781,-3.22595008773715,15.));
#37545=CARTESIAN_POINT('Ctrl Pts',(19.0661599344864,-3.22090173651085,15.));
#37546=CARTESIAN_POINT('Ctrl Pts',(19.1453253990185,-3.21510704576117,15.));
#37547=CARTESIAN_POINT('Ctrl Pts',(19.2245581120423,-3.2083040369031,15.));
#37548=CARTESIAN_POINT('Ctrl Pts',(19.3038697977783,-3.2001820370274,15.));
#37549=CARTESIAN_POINT('Ctrl Pts',(19.3832648965708,-3.19055618489382,15.));
#37550=CARTESIAN_POINT('Ctrl Pts',(19.4627345689632,-3.17944412249754,15.));
#37551=CARTESIAN_POINT('Ctrl Pts',(19.5422628528517,-3.16697679689294,15.));
#37552=CARTESIAN_POINT('Ctrl Pts',(19.6218301288731,-3.15334580802458,15.));
#37553=CARTESIAN_POINT('Ctrl Pts',(19.7014173131304,-3.13874131344865,15.));
#37554=CARTESIAN_POINT('Ctrl Pts',(19.7810105986827,-3.1232813132398,15.));
#37555=CARTESIAN_POINT('Ctrl Pts',(19.8606024365399,-3.10699659920993,15.));
#37556=CARTESIAN_POINT('Ctrl Pts',(19.9401889653541,-3.08986795998319,15.));
#37557=CARTESIAN_POINT('Ctrl Pts',(20.0197683853426,-3.07184950717982,15.));
#37558=CARTESIAN_POINT('Ctrl Pts',(20.0993390992966,-3.05289545759951,15.));
#37559=CARTESIAN_POINT('Ctrl Pts',(20.178897575607,-3.03299094576288,15.));
#37560=CARTESIAN_POINT('Ctrl Pts',(20.2584381977107,-3.01215393913612,15.));
#37561=CARTESIAN_POINT('Ctrl Pts',(20.3379542578194,-2.99042050197904,15.));
#37562=CARTESIAN_POINT('Ctrl Pts',(20.4174386170774,-2.96783492132513,15.));
#37563=CARTESIAN_POINT('Ctrl Pts',(20.4968844460513,-2.94443868035154,15.));
#37564=CARTESIAN_POINT('Ctrl Pts',(20.5762860772943,-2.92025778619206,15.));
#37565=CARTESIAN_POINT('Ctrl Pts',(20.6556389450993,-2.89530351700805,15.));
#37566=CARTESIAN_POINT('Ctrl Pts',(20.7349391669725,-2.86957843933153,15.));
#37567=CARTESIAN_POINT('Ctrl Pts',(20.8141832346435,-2.84308082507644,15.));
#37568=CARTESIAN_POINT('Ctrl Pts',(20.8933676828246,-2.81580940715318,15.));
#37569=CARTESIAN_POINT('Ctrl Pts',(20.9724887103073,-2.78776883747222,15.));
#37570=CARTESIAN_POINT('Ctrl Pts',(21.0515422162039,-2.7589691000769,15.));
#37571=CARTESIAN_POINT('Ctrl Pts',(21.1305239619219,-2.72942309852119,15.));
#37572=CARTESIAN_POINT('Ctrl Pts',(21.2094296949571,-2.69914481283353,15.));
#37573=CARTESIAN_POINT('Ctrl Pts',(21.2882552797978,-2.668147357083,15.));
#37574=CARTESIAN_POINT('Ctrl Pts',(21.3669968505594,-2.6364407451853,15.));
#37575=CARTESIAN_POINT('Ctrl Pts',(21.4456507822983,-2.60403221866523,15.));
#37576=CARTESIAN_POINT('Ctrl Pts',(21.5242136128466,-2.5709272835198,15.));
#37577=CARTESIAN_POINT('Ctrl Pts',(21.6026819803014,-2.53713053453766,15.));
#37578=CARTESIAN_POINT('Ctrl Pts',(21.6810525594039,-2.50264651177235,15.));
#37579=CARTESIAN_POINT('Ctrl Pts',(21.7593219872847,-2.46748070362075,15.));
#37580=CARTESIAN_POINT('Ctrl Pts',(21.8374868743435,-2.43163944362692,15.));
#37581=CARTESIAN_POINT('Ctrl Pts',(21.9155438409279,-2.39512947344577,15.));
#37582=CARTESIAN_POINT('Ctrl Pts',(21.9934895476958,-2.35795761145761,15.));
#37583=CARTESIAN_POINT('Ctrl Pts',(22.0713207257413,-2.32013040994125,15.));
#37584=CARTESIAN_POINT('Ctrl Pts',(22.1490342171802,-2.28165375160231,15.));
#37585=CARTESIAN_POINT('Ctrl Pts',(22.2266269576315,-2.24253288454712,15.));
#37586=CARTESIAN_POINT('Ctrl Pts',(22.3040959372933,-2.20277263221399,15.));
#37587=CARTESIAN_POINT('Ctrl Pts',(22.3814381677224,-2.16237755726404,15.));
#37588=CARTESIAN_POINT('Ctrl Pts',(22.4586506520939,-2.1213521324248,15.));
#37589=CARTESIAN_POINT('Ctrl Pts',(22.5357303426251,-2.07970095436224,15.));
#37590=CARTESIAN_POINT('Ctrl Pts',(22.6126741632309,-2.03742874317627,15.));
#37591=CARTESIAN_POINT('Ctrl Pts',(22.6894790673923,-1.99454021984253,15.));
#37592=CARTESIAN_POINT('Ctrl Pts',(22.7661420906702,-1.95104002082891,15.));
#37593=CARTESIAN_POINT('Ctrl Pts',(22.8426603964871,-1.90693261239855,15.));
#37594=CARTESIAN_POINT('Ctrl Pts',(22.9190313507225,-1.86222218327819,15.));
#37595=CARTESIAN_POINT('Ctrl Pts',(22.9952524859917,-1.81691265597281,15.));
#37596=CARTESIAN_POINT('Ctrl Pts',(23.0713213684573,-1.77100780743078,15.));
#37597=CARTESIAN_POINT('Ctrl Pts',(23.1472354850579,-1.72451136919382,15.));
#37598=CARTESIAN_POINT('Ctrl Pts',(23.2229921402299,-1.67742712670823,15.));
#37599=CARTESIAN_POINT('Ctrl Pts',(23.2985883089733,-1.62975905604583,15.));
#37600=CARTESIAN_POINT('Ctrl Pts',(23.3740206492924,-1.58151133638847,15.));
#37601=CARTESIAN_POINT('Ctrl Pts',(23.4492857841673,-1.53268814658653,15.));
#37602=CARTESIAN_POINT('Ctrl Pts',(23.5243805284282,-1.48329351290851,15.));
#37603=CARTESIAN_POINT('Ctrl Pts',(23.5993021272808,-1.4333311444639,15.));
#37604=CARTESIAN_POINT('Ctrl Pts',(23.6740485197917,-1.38280426780156,15.));
#37605=CARTESIAN_POINT('Ctrl Pts',(23.7635325055853,-1.32149774147467,15.));
#37606=CARTESIAN_POINT('Ctrl Pts',(23.8378812584003,-1.2697091254959,15.));
#37607=CARTESIAN_POINT('Ctrl Pts',(23.89721850443,-1.22783185562043,15.));
#37608=CARTESIAN_POINT('Ctrl Pts',(23.9416417798466,-1.19617306697386,15.));
#37609=CARTESIAN_POINT('Ctrl Pts',(23.9712218930251,-1.17495572484832,15.));
#37610=CARTESIAN_POINT('',(23.9712218930251,1.17495572484827,15.));
#37611=CARTESIAN_POINT('Origin',(1.15463194561016E-13,-6.93889390390723E-17,
15.));
#37612=CARTESIAN_POINT('',(18.5165898451125,3.2163316265074,15.));
#37613=CARTESIAN_POINT('Ctrl Pts',(23.9712218930251,1.17495572484832,15.));
#37614=CARTESIAN_POINT('Ctrl Pts',(23.9564318364582,1.18556439589232,15.));
#37615=CARTESIAN_POINT('Ctrl Pts',(23.9268340213744,1.20672599652272,15.));
#37616=CARTESIAN_POINT('Ctrl Pts',(23.8823841929226,1.2383011730893,15.));
#37617=CARTESIAN_POINT('Ctrl Pts',(23.8230115078373,1.28006684869166,15.));
#37618=CARTESIAN_POINT('Ctrl Pts',(23.748618507953,1.33171549586249,15.));
#37619=CARTESIAN_POINT('Ctrl Pts',(23.6740485197917,1.38280426780156,15.));
#37620=CARTESIAN_POINT('Ctrl Pts',(23.5993021272808,1.4333311444639,15.));
#37621=CARTESIAN_POINT('Ctrl Pts',(23.5243805284282,1.48329351290851,15.));
#37622=CARTESIAN_POINT('Ctrl Pts',(23.4492857841673,1.53268814658653,15.));
#37623=CARTESIAN_POINT('Ctrl Pts',(23.3740206492924,1.58151133638847,15.));
#37624=CARTESIAN_POINT('Ctrl Pts',(23.2985883089733,1.62975905604583,15.));
#37625=CARTESIAN_POINT('Ctrl Pts',(23.2229921402299,1.67742712670823,15.));
#37626=CARTESIAN_POINT('Ctrl Pts',(23.1472354850579,1.72451136919382,15.));
#37627=CARTESIAN_POINT('Ctrl Pts',(23.0713213684573,1.77100780743078,15.));
#37628=CARTESIAN_POINT('Ctrl Pts',(22.9952524859917,1.81691265597281,15.));
#37629=CARTESIAN_POINT('Ctrl Pts',(22.9190313507225,1.86222218327819,15.));
#37630=CARTESIAN_POINT('Ctrl Pts',(22.8426603964871,1.90693261239855,15.));
#37631=CARTESIAN_POINT('Ctrl Pts',(22.7661420906702,1.95104002082891,15.));
#37632=CARTESIAN_POINT('Ctrl Pts',(22.6894790673923,1.99454021984253,15.));
#37633=CARTESIAN_POINT('Ctrl Pts',(22.6126741632309,2.03742874317627,15.));
#37634=CARTESIAN_POINT('Ctrl Pts',(22.5357303426251,2.07970095436224,15.));
#37635=CARTESIAN_POINT('Ctrl Pts',(22.4586506520939,2.1213521324248,15.));
#37636=CARTESIAN_POINT('Ctrl Pts',(22.3814381677224,2.16237755726404,15.));
#37637=CARTESIAN_POINT('Ctrl Pts',(22.3040959372933,2.20277263221399,15.));
#37638=CARTESIAN_POINT('Ctrl Pts',(22.2266269576315,2.24253288454712,15.));
#37639=CARTESIAN_POINT('Ctrl Pts',(22.1490342171802,2.28165375160231,15.));
#37640=CARTESIAN_POINT('Ctrl Pts',(22.0713207257413,2.32013040994125,15.));
#37641=CARTESIAN_POINT('Ctrl Pts',(21.9934895476958,2.35795761145761,15.));
#37642=CARTESIAN_POINT('Ctrl Pts',(21.9155438409279,2.39512947344577,15.));
#37643=CARTESIAN_POINT('Ctrl Pts',(21.8374868743435,2.43163944362692,15.));
#37644=CARTESIAN_POINT('Ctrl Pts',(21.7593219872847,2.46748070362075,15.));
#37645=CARTESIAN_POINT('Ctrl Pts',(21.6810525594039,2.50264651177235,15.));
#37646=CARTESIAN_POINT('Ctrl Pts',(21.6026819803014,2.53713053453766,15.));
#37647=CARTESIAN_POINT('Ctrl Pts',(21.5242136128466,2.5709272835198,15.));
#37648=CARTESIAN_POINT('Ctrl Pts',(21.4456507822983,2.60403221866523,15.));
#37649=CARTESIAN_POINT('Ctrl Pts',(21.3669968505594,2.6364407451853,15.));
#37650=CARTESIAN_POINT('Ctrl Pts',(21.2882552797978,2.668147357083,15.));
#37651=CARTESIAN_POINT('Ctrl Pts',(21.2094296949571,2.69914481283353,15.));
#37652=CARTESIAN_POINT('Ctrl Pts',(21.1305239619219,2.72942309852119,15.));
#37653=CARTESIAN_POINT('Ctrl Pts',(21.0515422162039,2.7589691000769,15.));
#37654=CARTESIAN_POINT('Ctrl Pts',(20.9724887103073,2.78776883747222,15.));
#37655=CARTESIAN_POINT('Ctrl Pts',(20.8933676828246,2.81580940715318,15.));
#37656=CARTESIAN_POINT('Ctrl Pts',(20.8141832346435,2.84308082507644,15.));
#37657=CARTESIAN_POINT('Ctrl Pts',(20.7349391669725,2.86957843933153,15.));
#37658=CARTESIAN_POINT('Ctrl Pts',(20.6556389450993,2.89530351700805,15.));
#37659=CARTESIAN_POINT('Ctrl Pts',(20.5762860772943,2.92025778619206,15.));
#37660=CARTESIAN_POINT('Ctrl Pts',(20.4968844460513,2.94443868035154,15.));
#37661=CARTESIAN_POINT('Ctrl Pts',(20.4174386170774,2.96783492132513,15.));
#37662=CARTESIAN_POINT('Ctrl Pts',(20.3379542578194,2.99042050197904,15.));
#37663=CARTESIAN_POINT('Ctrl Pts',(20.2584381977107,3.01215393913612,15.));
#37664=CARTESIAN_POINT('Ctrl Pts',(20.178897575607,3.03299094576288,15.));
#37665=CARTESIAN_POINT('Ctrl Pts',(20.0993390992966,3.05289545759951,15.));
#37666=CARTESIAN_POINT('Ctrl Pts',(20.0197683853426,3.07184950717982,15.));
#37667=CARTESIAN_POINT('Ctrl Pts',(19.9401889653541,3.08986795998319,15.));
#37668=CARTESIAN_POINT('Ctrl Pts',(19.8606024365399,3.10699659920993,15.));
#37669=CARTESIAN_POINT('Ctrl Pts',(19.7810105986827,3.1232813132398,15.));
#37670=CARTESIAN_POINT('Ctrl Pts',(19.7014173131304,3.13874131344865,15.));
#37671=CARTESIAN_POINT('Ctrl Pts',(19.6218301288731,3.15334580802458,15.));
#37672=CARTESIAN_POINT('Ctrl Pts',(19.5422628528517,3.16697679689294,15.));
#37673=CARTESIAN_POINT('Ctrl Pts',(19.4627345689632,3.17944412249754,15.));
#37674=CARTESIAN_POINT('Ctrl Pts',(19.3832648965708,3.19055618489382,15.));
#37675=CARTESIAN_POINT('Ctrl Pts',(19.3038697977783,3.2001820370274,15.));
#37676=CARTESIAN_POINT('Ctrl Pts',(19.2245581120423,3.2083040369031,15.));
#37677=CARTESIAN_POINT('Ctrl Pts',(19.1453253990185,3.21510704576117,15.));
#37678=CARTESIAN_POINT('Ctrl Pts',(19.0661599344864,3.22090173651085,15.));
#37679=CARTESIAN_POINT('Ctrl Pts',(18.987055820781,3.22595008773715,15.));
#37680=CARTESIAN_POINT('Ctrl Pts',(18.908024664264,3.23031169402939,15.));
#37681=CARTESIAN_POINT('Ctrl Pts',(18.8291062617862,3.23370091065669,15.));
#37682=CARTESIAN_POINT('Ctrl Pts',(18.7503838921122,3.23528809328097,15.));
#37683=CARTESIAN_POINT('Ctrl Pts',(18.6719665316945,3.23390622002644,15.));
#37684=CARTESIAN_POINT('Ctrl Pts',(18.6095634206219,3.2294700044416,15.));
#37685=CARTESIAN_POINT('Ctrl Pts',(18.5629852384321,3.22384302136592,15.));
#37686=CARTESIAN_POINT('Ctrl Pts',(18.5320375674878,3.2190148958593,15.));
#37687=CARTESIAN_POINT('Ctrl Pts',(18.5165898451125,3.2163316265074,15.));
#37688=CARTESIAN_POINT('',(16.1003491021971,2.79663061332403,15.));
#37689=CARTESIAN_POINT('',(15.135366975784,2.62901321950806,15.));
#37690=CARTESIAN_POINT('',(14.9562571344462,3.5508810918317,15.));
#37691=CARTESIAN_POINT('Origin',(15.9292116709051,3.78187778008512,15.));
#37692=CARTESIAN_POINT('Origin',(0.,0.,15.));
#37693=CARTESIAN_POINT('Origin',(0.,0.,15.));
#37694=CARTESIAN_POINT('Origin',(0.,0.,15.));
#37695=CARTESIAN_POINT('Origin',(0.,0.,15.));
#37696=CARTESIAN_POINT('Origin',(0.,0.,15.));
#37697=CARTESIAN_POINT('Origin',(0.,0.,15.));
#37698=CARTESIAN_POINT('Origin',(0.,0.,15.));
#37699=CARTESIAN_POINT('Origin',(0.,0.,15.));
#37700=CARTESIAN_POINT('Origin',(0.,0.,15.));
#37701=CARTESIAN_POINT('Origin',(0.,0.,0.));
#37702=CARTESIAN_POINT('',(14.9562571344462,3.5508810918317,0.));
#37703=CARTESIAN_POINT('Origin',(0.,0.,0.));
#37704=CARTESIAN_POINT('Origin',(0.,0.,0.));
#37705=CARTESIAN_POINT('Origin',(0.,0.,0.));
#37706=CARTESIAN_POINT('Origin',(0.,0.,0.));
#37707=CARTESIAN_POINT('Origin',(0.,0.,0.));
#37708=CARTESIAN_POINT('Origin',(0.,0.,0.));
#37709=CARTESIAN_POINT('Origin',(0.,0.,0.));
#37710=CARTESIAN_POINT('Origin',(0.,0.,0.));
#37711=CARTESIAN_POINT('Origin',(15.9292116709051,3.78187778008512,0.));
#37712=CARTESIAN_POINT('',(16.1003491021971,2.79663061332403,0.));
#37713=CARTESIAN_POINT('Origin',(18.5165898451125,3.2163316265074,0.));
#37714=CARTESIAN_POINT('',(18.5165898451125,3.2163316265074,0.));
#37715=CARTESIAN_POINT('Origin',(15.9292116709051,-3.78187778008512,0.));
#37716=CARTESIAN_POINT('',(16.1003491021971,-2.79663061332403,0.));
#37717=CARTESIAN_POINT('',(14.9562571344462,-3.5508810918317,0.));
#37718=CARTESIAN_POINT('Origin',(15.135366975784,-2.62901321950806,0.));
#37719=CARTESIAN_POINT('',(18.5165898451125,-3.2163316265074,0.));
#37720=CARTESIAN_POINT('Ctrl Pts',(23.9712218930251,1.17495572484832,0.));
#37721=CARTESIAN_POINT('Ctrl Pts',(23.9712218930251,1.17495572484832,18.));
#37722=CARTESIAN_POINT('Ctrl Pts',(23.9564318364582,1.18556439589232,0.));
#37723=CARTESIAN_POINT('Ctrl Pts',(23.9564318364582,1.18556439589232,18.));
#37724=CARTESIAN_POINT('Ctrl Pts',(23.9268340213744,1.20672599652272,0.));
#37725=CARTESIAN_POINT('Ctrl Pts',(23.9268340213744,1.20672599652272,18.));
#37726=CARTESIAN_POINT('Ctrl Pts',(23.8823841929226,1.2383011730893,0.));
#37727=CARTESIAN_POINT('Ctrl Pts',(23.8823841929226,1.2383011730893,18.));
#37728=CARTESIAN_POINT('Ctrl Pts',(23.8230115078373,1.28006684869166,0.));
#37729=CARTESIAN_POINT('Ctrl Pts',(23.8230115078373,1.28006684869166,18.));
#37730=CARTESIAN_POINT('Ctrl Pts',(23.748618507953,1.33171549586249,0.));
#37731=CARTESIAN_POINT('Ctrl Pts',(23.748618507953,1.33171549586249,18.));
#37732=CARTESIAN_POINT('Ctrl Pts',(23.6740485197917,1.38280426780156,0.));
#37733=CARTESIAN_POINT('Ctrl Pts',(23.6740485197917,1.38280426780156,18.));
#37734=CARTESIAN_POINT('Ctrl Pts',(23.5993021272808,1.4333311444639,0.));
#37735=CARTESIAN_POINT('Ctrl Pts',(23.5993021272808,1.4333311444639,18.));
#37736=CARTESIAN_POINT('Ctrl Pts',(23.5243805284282,1.48329351290851,0.));
#37737=CARTESIAN_POINT('Ctrl Pts',(23.5243805284282,1.48329351290851,18.));
#37738=CARTESIAN_POINT('Ctrl Pts',(23.4492857841673,1.53268814658653,0.));
#37739=CARTESIAN_POINT('Ctrl Pts',(23.4492857841673,1.53268814658653,18.));
#37740=CARTESIAN_POINT('Ctrl Pts',(23.3740206492924,1.58151133638847,0.));
#37741=CARTESIAN_POINT('Ctrl Pts',(23.3740206492924,1.58151133638847,18.));
#37742=CARTESIAN_POINT('Ctrl Pts',(23.2985883089733,1.62975905604583,0.));
#37743=CARTESIAN_POINT('Ctrl Pts',(23.2985883089733,1.62975905604583,18.));
#37744=CARTESIAN_POINT('Ctrl Pts',(23.2229921402299,1.67742712670823,0.));
#37745=CARTESIAN_POINT('Ctrl Pts',(23.2229921402299,1.67742712670823,18.));
#37746=CARTESIAN_POINT('Ctrl Pts',(23.1472354850579,1.72451136919382,0.));
#37747=CARTESIAN_POINT('Ctrl Pts',(23.1472354850579,1.72451136919382,18.));
#37748=CARTESIAN_POINT('Ctrl Pts',(23.0713213684573,1.77100780743078,0.));
#37749=CARTESIAN_POINT('Ctrl Pts',(23.0713213684573,1.77100780743078,18.));
#37750=CARTESIAN_POINT('Ctrl Pts',(22.9952524859917,1.81691265597281,0.));
#37751=CARTESIAN_POINT('Ctrl Pts',(22.9952524859917,1.81691265597281,18.));
#37752=CARTESIAN_POINT('Ctrl Pts',(22.9190313507225,1.86222218327819,0.));
#37753=CARTESIAN_POINT('Ctrl Pts',(22.9190313507225,1.86222218327819,18.));
#37754=CARTESIAN_POINT('Ctrl Pts',(22.8426603964871,1.90693261239855,0.));
#37755=CARTESIAN_POINT('Ctrl Pts',(22.8426603964871,1.90693261239855,18.));
#37756=CARTESIAN_POINT('Ctrl Pts',(22.7661420906702,1.95104002082891,0.));
#37757=CARTESIAN_POINT('Ctrl Pts',(22.7661420906702,1.95104002082891,18.));
#37758=CARTESIAN_POINT('Ctrl Pts',(22.6894790673923,1.99454021984253,0.));
#37759=CARTESIAN_POINT('Ctrl Pts',(22.6894790673923,1.99454021984253,18.));
#37760=CARTESIAN_POINT('Ctrl Pts',(22.6126741632309,2.03742874317627,0.));
#37761=CARTESIAN_POINT('Ctrl Pts',(22.6126741632309,2.03742874317627,18.));
#37762=CARTESIAN_POINT('Ctrl Pts',(22.5357303426251,2.07970095436224,0.));
#37763=CARTESIAN_POINT('Ctrl Pts',(22.5357303426251,2.07970095436224,18.));
#37764=CARTESIAN_POINT('Ctrl Pts',(22.4586506520939,2.1213521324248,0.));
#37765=CARTESIAN_POINT('Ctrl Pts',(22.4586506520939,2.1213521324248,18.));
#37766=CARTESIAN_POINT('Ctrl Pts',(22.3814381677224,2.16237755726404,0.));
#37767=CARTESIAN_POINT('Ctrl Pts',(22.3814381677224,2.16237755726404,18.));
#37768=CARTESIAN_POINT('Ctrl Pts',(22.3040959372933,2.20277263221399,0.));
#37769=CARTESIAN_POINT('Ctrl Pts',(22.3040959372933,2.20277263221399,18.));
#37770=CARTESIAN_POINT('Ctrl Pts',(22.2266269576315,2.24253288454712,0.));
#37771=CARTESIAN_POINT('Ctrl Pts',(22.2266269576315,2.24253288454712,18.));
#37772=CARTESIAN_POINT('Ctrl Pts',(22.1490342171802,2.28165375160231,0.));
#37773=CARTESIAN_POINT('Ctrl Pts',(22.1490342171802,2.28165375160231,18.));
#37774=CARTESIAN_POINT('Ctrl Pts',(22.0713207257413,2.32013040994125,0.));
#37775=CARTESIAN_POINT('Ctrl Pts',(22.0713207257413,2.32013040994125,18.));
#37776=CARTESIAN_POINT('Ctrl Pts',(21.9934895476958,2.35795761145761,0.));
#37777=CARTESIAN_POINT('Ctrl Pts',(21.9934895476958,2.35795761145761,18.));
#37778=CARTESIAN_POINT('Ctrl Pts',(21.9155438409279,2.39512947344577,0.));
#37779=CARTESIAN_POINT('Ctrl Pts',(21.9155438409279,2.39512947344577,18.));
#37780=CARTESIAN_POINT('Ctrl Pts',(21.8374868743435,2.43163944362692,0.));
#37781=CARTESIAN_POINT('Ctrl Pts',(21.8374868743435,2.43163944362692,18.));
#37782=CARTESIAN_POINT('Ctrl Pts',(21.7593219872847,2.46748070362075,0.));
#37783=CARTESIAN_POINT('Ctrl Pts',(21.7593219872847,2.46748070362075,18.));
#37784=CARTESIAN_POINT('Ctrl Pts',(21.6810525594039,2.50264651177235,0.));
#37785=CARTESIAN_POINT('Ctrl Pts',(21.6810525594039,2.50264651177235,18.));
#37786=CARTESIAN_POINT('Ctrl Pts',(21.6026819803014,2.53713053453766,0.));
#37787=CARTESIAN_POINT('Ctrl Pts',(21.6026819803014,2.53713053453766,18.));
#37788=CARTESIAN_POINT('Ctrl Pts',(21.5242136128466,2.5709272835198,0.));
#37789=CARTESIAN_POINT('Ctrl Pts',(21.5242136128466,2.5709272835198,18.));
#37790=CARTESIAN_POINT('Ctrl Pts',(21.4456507822983,2.60403221866523,0.));
#37791=CARTESIAN_POINT('Ctrl Pts',(21.4456507822983,2.60403221866523,18.));
#37792=CARTESIAN_POINT('Ctrl Pts',(21.3669968505594,2.6364407451853,0.));
#37793=CARTESIAN_POINT('Ctrl Pts',(21.3669968505594,2.6364407451853,18.));
#37794=CARTESIAN_POINT('Ctrl Pts',(21.2882552797978,2.668147357083,0.));
#37795=CARTESIAN_POINT('Ctrl Pts',(21.2882552797978,2.668147357083,18.));
#37796=CARTESIAN_POINT('Ctrl Pts',(21.2094296949571,2.69914481283353,0.));
#37797=CARTESIAN_POINT('Ctrl Pts',(21.2094296949571,2.69914481283353,18.));
#37798=CARTESIAN_POINT('Ctrl Pts',(21.1305239619219,2.72942309852119,0.));
#37799=CARTESIAN_POINT('Ctrl Pts',(21.1305239619219,2.72942309852119,18.));
#37800=CARTESIAN_POINT('Ctrl Pts',(21.0515422162039,2.7589691000769,0.));
#37801=CARTESIAN_POINT('Ctrl Pts',(21.0515422162039,2.7589691000769,18.));
#37802=CARTESIAN_POINT('Ctrl Pts',(20.9724887103073,2.78776883747222,0.));
#37803=CARTESIAN_POINT('Ctrl Pts',(20.9724887103073,2.78776883747222,18.));
#37804=CARTESIAN_POINT('Ctrl Pts',(20.8933676828246,2.81580940715318,0.));
#37805=CARTESIAN_POINT('Ctrl Pts',(20.8933676828246,2.81580940715318,18.));
#37806=CARTESIAN_POINT('Ctrl Pts',(20.8141832346435,2.84308082507644,0.));
#37807=CARTESIAN_POINT('Ctrl Pts',(20.8141832346435,2.84308082507644,18.));
#37808=CARTESIAN_POINT('Ctrl Pts',(20.7349391669725,2.86957843933153,0.));
#37809=CARTESIAN_POINT('Ctrl Pts',(20.7349391669725,2.86957843933153,18.));
#37810=CARTESIAN_POINT('Ctrl Pts',(20.6556389450993,2.89530351700805,0.));
#37811=CARTESIAN_POINT('Ctrl Pts',(20.6556389450993,2.89530351700805,18.));
#37812=CARTESIAN_POINT('Ctrl Pts',(20.5762860772943,2.92025778619206,0.));
#37813=CARTESIAN_POINT('Ctrl Pts',(20.5762860772943,2.92025778619206,18.));
#37814=CARTESIAN_POINT('Ctrl Pts',(20.4968844460513,2.94443868035154,0.));
#37815=CARTESIAN_POINT('Ctrl Pts',(20.4968844460513,2.94443868035154,18.));
#37816=CARTESIAN_POINT('Ctrl Pts',(20.4174386170774,2.96783492132513,0.));
#37817=CARTESIAN_POINT('Ctrl Pts',(20.4174386170774,2.96783492132513,18.));
#37818=CARTESIAN_POINT('Ctrl Pts',(20.3379542578194,2.99042050197904,0.));
#37819=CARTESIAN_POINT('Ctrl Pts',(20.3379542578194,2.99042050197904,18.));
#37820=CARTESIAN_POINT('Ctrl Pts',(20.2584381977107,3.01215393913612,0.));
#37821=CARTESIAN_POINT('Ctrl Pts',(20.2584381977107,3.01215393913612,18.));
#37822=CARTESIAN_POINT('Ctrl Pts',(20.178897575607,3.03299094576288,0.));
#37823=CARTESIAN_POINT('Ctrl Pts',(20.178897575607,3.03299094576288,18.));
#37824=CARTESIAN_POINT('Ctrl Pts',(20.0993390992966,3.05289545759951,0.));
#37825=CARTESIAN_POINT('Ctrl Pts',(20.0993390992966,3.05289545759951,18.));
#37826=CARTESIAN_POINT('Ctrl Pts',(20.0197683853426,3.07184950717982,0.));
#37827=CARTESIAN_POINT('Ctrl Pts',(20.0197683853426,3.07184950717982,18.));
#37828=CARTESIAN_POINT('Ctrl Pts',(19.9401889653541,3.08986795998319,0.));
#37829=CARTESIAN_POINT('Ctrl Pts',(19.9401889653541,3.08986795998319,18.));
#37830=CARTESIAN_POINT('Ctrl Pts',(19.8606024365399,3.10699659920993,0.));
#37831=CARTESIAN_POINT('Ctrl Pts',(19.8606024365399,3.10699659920993,18.));
#37832=CARTESIAN_POINT('Ctrl Pts',(19.7810105986827,3.1232813132398,0.));
#37833=CARTESIAN_POINT('Ctrl Pts',(19.7810105986827,3.1232813132398,18.));
#37834=CARTESIAN_POINT('Ctrl Pts',(19.7014173131304,3.13874131344865,0.));
#37835=CARTESIAN_POINT('Ctrl Pts',(19.7014173131304,3.13874131344865,18.));
#37836=CARTESIAN_POINT('Ctrl Pts',(19.6218301288731,3.15334580802458,0.));
#37837=CARTESIAN_POINT('Ctrl Pts',(19.6218301288731,3.15334580802458,18.));
#37838=CARTESIAN_POINT('Ctrl Pts',(19.5422628528517,3.16697679689294,0.));
#37839=CARTESIAN_POINT('Ctrl Pts',(19.5422628528517,3.16697679689294,18.));
#37840=CARTESIAN_POINT('Ctrl Pts',(19.4627345689632,3.17944412249754,0.));
#37841=CARTESIAN_POINT('Ctrl Pts',(19.4627345689632,3.17944412249754,18.));
#37842=CARTESIAN_POINT('Ctrl Pts',(19.3832648965708,3.19055618489382,0.));
#37843=CARTESIAN_POINT('Ctrl Pts',(19.3832648965708,3.19055618489382,18.));
#37844=CARTESIAN_POINT('Ctrl Pts',(19.3038697977783,3.2001820370274,0.));
#37845=CARTESIAN_POINT('Ctrl Pts',(19.3038697977783,3.2001820370274,18.));
#37846=CARTESIAN_POINT('Ctrl Pts',(19.2245581120423,3.2083040369031,0.));
#37847=CARTESIAN_POINT('Ctrl Pts',(19.2245581120423,3.2083040369031,18.));
#37848=CARTESIAN_POINT('Ctrl Pts',(19.1453253990185,3.21510704576117,0.));
#37849=CARTESIAN_POINT('Ctrl Pts',(19.1453253990185,3.21510704576117,18.));
#37850=CARTESIAN_POINT('Ctrl Pts',(19.0661599344864,3.22090173651085,0.));
#37851=CARTESIAN_POINT('Ctrl Pts',(19.0661599344864,3.22090173651085,18.));
#37852=CARTESIAN_POINT('Ctrl Pts',(18.987055820781,3.22595008773715,0.));
#37853=CARTESIAN_POINT('Ctrl Pts',(18.987055820781,3.22595008773715,18.));
#37854=CARTESIAN_POINT('Ctrl Pts',(18.908024664264,3.23031169402939,0.));
#37855=CARTESIAN_POINT('Ctrl Pts',(18.908024664264,3.23031169402939,18.));
#37856=CARTESIAN_POINT('Ctrl Pts',(18.8291062617862,3.23370091065669,0.));
#37857=CARTESIAN_POINT('Ctrl Pts',(18.8291062617862,3.23370091065669,18.));
#37858=CARTESIAN_POINT('Ctrl Pts',(18.7503838921122,3.23528809328097,0.));
#37859=CARTESIAN_POINT('Ctrl Pts',(18.7503838921122,3.23528809328097,18.));
#37860=CARTESIAN_POINT('Ctrl Pts',(18.6719665316945,3.23390622002644,0.));
#37861=CARTESIAN_POINT('Ctrl Pts',(18.6719665316945,3.23390622002644,18.));
#37862=CARTESIAN_POINT('Ctrl Pts',(18.6095634206219,3.2294700044416,0.));
#37863=CARTESIAN_POINT('Ctrl Pts',(18.6095634206219,3.2294700044416,18.));
#37864=CARTESIAN_POINT('Ctrl Pts',(18.5629852384321,3.22384302136592,0.));
#37865=CARTESIAN_POINT('Ctrl Pts',(18.5629852384321,3.22384302136592,18.));
#37866=CARTESIAN_POINT('Ctrl Pts',(18.5320375674878,3.2190148958593,0.));
#37867=CARTESIAN_POINT('Ctrl Pts',(18.5320375674878,3.2190148958593,18.));
#37868=CARTESIAN_POINT('Ctrl Pts',(18.5165898451125,3.2163316265074,0.));
#37869=CARTESIAN_POINT('Ctrl Pts',(18.5165898451125,3.2163316265074,18.));
#37870=CARTESIAN_POINT('',(23.9712218930251,1.17495572484827,0.));
#37871=CARTESIAN_POINT('Origin',(1.15463194561016E-13,-6.93889390390723E-17,
0.));
#37872=CARTESIAN_POINT('',(23.9712218930251,-1.17495572484832,0.));
#37873=CARTESIAN_POINT('Ctrl Pts',(18.5165898451125,-3.2163316265074,0.));
#37874=CARTESIAN_POINT('Ctrl Pts',(18.5165898451125,-3.2163316265074,18.));
#37875=CARTESIAN_POINT('Ctrl Pts',(18.5320375674878,-3.2190148958593,0.));
#37876=CARTESIAN_POINT('Ctrl Pts',(18.5320375674878,-3.2190148958593,18.));
#37877=CARTESIAN_POINT('Ctrl Pts',(18.5629852384321,-3.22384302136592,0.));
#37878=CARTESIAN_POINT('Ctrl Pts',(18.5629852384321,-3.22384302136592,18.));
#37879=CARTESIAN_POINT('Ctrl Pts',(18.6095634206219,-3.2294700044416,0.));
#37880=CARTESIAN_POINT('Ctrl Pts',(18.6095634206219,-3.2294700044416,18.));
#37881=CARTESIAN_POINT('Ctrl Pts',(18.6719665316945,-3.23390622002644,0.));
#37882=CARTESIAN_POINT('Ctrl Pts',(18.6719665316945,-3.23390622002644,18.));
#37883=CARTESIAN_POINT('Ctrl Pts',(18.7503838921122,-3.23528809328097,0.));
#37884=CARTESIAN_POINT('Ctrl Pts',(18.7503838921122,-3.23528809328097,18.));
#37885=CARTESIAN_POINT('Ctrl Pts',(18.8291062617862,-3.23370091065669,0.));
#37886=CARTESIAN_POINT('Ctrl Pts',(18.8291062617862,-3.23370091065669,18.));
#37887=CARTESIAN_POINT('Ctrl Pts',(18.908024664264,-3.23031169402939,0.));
#37888=CARTESIAN_POINT('Ctrl Pts',(18.908024664264,-3.23031169402939,18.));
#37889=CARTESIAN_POINT('Ctrl Pts',(18.987055820781,-3.22595008773715,0.));
#37890=CARTESIAN_POINT('Ctrl Pts',(18.987055820781,-3.22595008773715,18.));
#37891=CARTESIAN_POINT('Ctrl Pts',(19.0661599344864,-3.22090173651085,0.));
#37892=CARTESIAN_POINT('Ctrl Pts',(19.0661599344864,-3.22090173651085,18.));
#37893=CARTESIAN_POINT('Ctrl Pts',(19.1453253990185,-3.21510704576117,0.));
#37894=CARTESIAN_POINT('Ctrl Pts',(19.1453253990185,-3.21510704576117,18.));
#37895=CARTESIAN_POINT('Ctrl Pts',(19.2245581120423,-3.2083040369031,0.));
#37896=CARTESIAN_POINT('Ctrl Pts',(19.2245581120423,-3.2083040369031,18.));
#37897=CARTESIAN_POINT('Ctrl Pts',(19.3038697977783,-3.2001820370274,0.));
#37898=CARTESIAN_POINT('Ctrl Pts',(19.3038697977783,-3.2001820370274,18.));
#37899=CARTESIAN_POINT('Ctrl Pts',(19.3832648965708,-3.19055618489382,0.));
#37900=CARTESIAN_POINT('Ctrl Pts',(19.3832648965708,-3.19055618489382,18.));
#37901=CARTESIAN_POINT('Ctrl Pts',(19.4627345689632,-3.17944412249754,0.));
#37902=CARTESIAN_POINT('Ctrl Pts',(19.4627345689632,-3.17944412249754,18.));
#37903=CARTESIAN_POINT('Ctrl Pts',(19.5422628528517,-3.16697679689294,0.));
#37904=CARTESIAN_POINT('Ctrl Pts',(19.5422628528517,-3.16697679689294,18.));
#37905=CARTESIAN_POINT('Ctrl Pts',(19.6218301288731,-3.15334580802458,0.));
#37906=CARTESIAN_POINT('Ctrl Pts',(19.6218301288731,-3.15334580802458,18.));
#37907=CARTESIAN_POINT('Ctrl Pts',(19.7014173131304,-3.13874131344865,0.));
#37908=CARTESIAN_POINT('Ctrl Pts',(19.7014173131304,-3.13874131344865,18.));
#37909=CARTESIAN_POINT('Ctrl Pts',(19.7810105986827,-3.1232813132398,0.));
#37910=CARTESIAN_POINT('Ctrl Pts',(19.7810105986827,-3.1232813132398,18.));
#37911=CARTESIAN_POINT('Ctrl Pts',(19.8606024365399,-3.10699659920993,0.));
#37912=CARTESIAN_POINT('Ctrl Pts',(19.8606024365399,-3.10699659920993,18.));
#37913=CARTESIAN_POINT('Ctrl Pts',(19.9401889653541,-3.08986795998319,0.));
#37914=CARTESIAN_POINT('Ctrl Pts',(19.9401889653541,-3.08986795998319,18.));
#37915=CARTESIAN_POINT('Ctrl Pts',(20.0197683853426,-3.07184950717982,0.));
#37916=CARTESIAN_POINT('Ctrl Pts',(20.0197683853426,-3.07184950717982,18.));
#37917=CARTESIAN_POINT('Ctrl Pts',(20.0993390992966,-3.05289545759951,0.));
#37918=CARTESIAN_POINT('Ctrl Pts',(20.0993390992966,-3.05289545759951,18.));
#37919=CARTESIAN_POINT('Ctrl Pts',(20.178897575607,-3.03299094576288,0.));
#37920=CARTESIAN_POINT('Ctrl Pts',(20.178897575607,-3.03299094576288,18.));
#37921=CARTESIAN_POINT('Ctrl Pts',(20.2584381977107,-3.01215393913612,0.));
#37922=CARTESIAN_POINT('Ctrl Pts',(20.2584381977107,-3.01215393913612,18.));
#37923=CARTESIAN_POINT('Ctrl Pts',(20.3379542578194,-2.99042050197904,0.));
#37924=CARTESIAN_POINT('Ctrl Pts',(20.3379542578194,-2.99042050197904,18.));
#37925=CARTESIAN_POINT('Ctrl Pts',(20.4174386170774,-2.96783492132513,0.));
#37926=CARTESIAN_POINT('Ctrl Pts',(20.4174386170774,-2.96783492132513,18.));
#37927=CARTESIAN_POINT('Ctrl Pts',(20.4968844460513,-2.94443868035154,0.));
#37928=CARTESIAN_POINT('Ctrl Pts',(20.4968844460513,-2.94443868035154,18.));
#37929=CARTESIAN_POINT('Ctrl Pts',(20.5762860772943,-2.92025778619206,0.));
#37930=CARTESIAN_POINT('Ctrl Pts',(20.5762860772943,-2.92025778619206,18.));
#37931=CARTESIAN_POINT('Ctrl Pts',(20.6556389450993,-2.89530351700805,0.));
#37932=CARTESIAN_POINT('Ctrl Pts',(20.6556389450993,-2.89530351700805,18.));
#37933=CARTESIAN_POINT('Ctrl Pts',(20.7349391669725,-2.86957843933153,0.));
#37934=CARTESIAN_POINT('Ctrl Pts',(20.7349391669725,-2.86957843933153,18.));
#37935=CARTESIAN_POINT('Ctrl Pts',(20.8141832346435,-2.84308082507644,0.));
#37936=CARTESIAN_POINT('Ctrl Pts',(20.8141832346435,-2.84308082507644,18.));
#37937=CARTESIAN_POINT('Ctrl Pts',(20.8933676828246,-2.81580940715318,0.));
#37938=CARTESIAN_POINT('Ctrl Pts',(20.8933676828246,-2.81580940715318,18.));
#37939=CARTESIAN_POINT('Ctrl Pts',(20.9724887103073,-2.78776883747222,0.));
#37940=CARTESIAN_POINT('Ctrl Pts',(20.9724887103073,-2.78776883747222,18.));
#37941=CARTESIAN_POINT('Ctrl Pts',(21.0515422162039,-2.7589691000769,0.));
#37942=CARTESIAN_POINT('Ctrl Pts',(21.0515422162039,-2.7589691000769,18.));
#37943=CARTESIAN_POINT('Ctrl Pts',(21.1305239619219,-2.72942309852119,0.));
#37944=CARTESIAN_POINT('Ctrl Pts',(21.1305239619219,-2.72942309852119,18.));
#37945=CARTESIAN_POINT('Ctrl Pts',(21.2094296949571,-2.69914481283353,0.));
#37946=CARTESIAN_POINT('Ctrl Pts',(21.2094296949571,-2.69914481283353,18.));
#37947=CARTESIAN_POINT('Ctrl Pts',(21.2882552797978,-2.668147357083,0.));
#37948=CARTESIAN_POINT('Ctrl Pts',(21.2882552797978,-2.668147357083,18.));
#37949=CARTESIAN_POINT('Ctrl Pts',(21.3669968505594,-2.6364407451853,0.));
#37950=CARTESIAN_POINT('Ctrl Pts',(21.3669968505594,-2.6364407451853,18.));
#37951=CARTESIAN_POINT('Ctrl Pts',(21.4456507822983,-2.60403221866523,0.));
#37952=CARTESIAN_POINT('Ctrl Pts',(21.4456507822983,-2.60403221866523,18.));
#37953=CARTESIAN_POINT('Ctrl Pts',(21.5242136128466,-2.5709272835198,0.));
#37954=CARTESIAN_POINT('Ctrl Pts',(21.5242136128466,-2.5709272835198,18.));
#37955=CARTESIAN_POINT('Ctrl Pts',(21.6026819803014,-2.53713053453766,0.));
#37956=CARTESIAN_POINT('Ctrl Pts',(21.6026819803014,-2.53713053453766,18.));
#37957=CARTESIAN_POINT('Ctrl Pts',(21.6810525594039,-2.50264651177235,0.));
#37958=CARTESIAN_POINT('Ctrl Pts',(21.6810525594039,-2.50264651177235,18.));
#37959=CARTESIAN_POINT('Ctrl Pts',(21.7593219872847,-2.46748070362075,0.));
#37960=CARTESIAN_POINT('Ctrl Pts',(21.7593219872847,-2.46748070362075,18.));
#37961=CARTESIAN_POINT('Ctrl Pts',(21.8374868743435,-2.43163944362692,0.));
#37962=CARTESIAN_POINT('Ctrl Pts',(21.8374868743435,-2.43163944362692,18.));
#37963=CARTESIAN_POINT('Ctrl Pts',(21.9155438409279,-2.39512947344577,0.));
#37964=CARTESIAN_POINT('Ctrl Pts',(21.9155438409279,-2.39512947344577,18.));
#37965=CARTESIAN_POINT('Ctrl Pts',(21.9934895476958,-2.35795761145761,0.));
#37966=CARTESIAN_POINT('Ctrl Pts',(21.9934895476958,-2.35795761145761,18.));
#37967=CARTESIAN_POINT('Ctrl Pts',(22.0713207257413,-2.32013040994125,0.));
#37968=CARTESIAN_POINT('Ctrl Pts',(22.0713207257413,-2.32013040994125,18.));
#37969=CARTESIAN_POINT('Ctrl Pts',(22.1490342171802,-2.28165375160231,0.));
#37970=CARTESIAN_POINT('Ctrl Pts',(22.1490342171802,-2.28165375160231,18.));
#37971=CARTESIAN_POINT('Ctrl Pts',(22.2266269576315,-2.24253288454712,0.));
#37972=CARTESIAN_POINT('Ctrl Pts',(22.2266269576315,-2.24253288454712,18.));
#37973=CARTESIAN_POINT('Ctrl Pts',(22.3040959372933,-2.20277263221399,0.));
#37974=CARTESIAN_POINT('Ctrl Pts',(22.3040959372933,-2.20277263221399,18.));
#37975=CARTESIAN_POINT('Ctrl Pts',(22.3814381677224,-2.16237755726404,0.));
#37976=CARTESIAN_POINT('Ctrl Pts',(22.3814381677224,-2.16237755726404,18.));
#37977=CARTESIAN_POINT('Ctrl Pts',(22.4586506520939,-2.1213521324248,0.));
#37978=CARTESIAN_POINT('Ctrl Pts',(22.4586506520939,-2.1213521324248,18.));
#37979=CARTESIAN_POINT('Ctrl Pts',(22.5357303426251,-2.07970095436224,0.));
#37980=CARTESIAN_POINT('Ctrl Pts',(22.5357303426251,-2.07970095436224,18.));
#37981=CARTESIAN_POINT('Ctrl Pts',(22.6126741632309,-2.03742874317627,0.));
#37982=CARTESIAN_POINT('Ctrl Pts',(22.6126741632309,-2.03742874317627,18.));
#37983=CARTESIAN_POINT('Ctrl Pts',(22.6894790673923,-1.99454021984253,0.));
#37984=CARTESIAN_POINT('Ctrl Pts',(22.6894790673923,-1.99454021984253,18.));
#37985=CARTESIAN_POINT('Ctrl Pts',(22.7661420906702,-1.95104002082891,0.));
#37986=CARTESIAN_POINT('Ctrl Pts',(22.7661420906702,-1.95104002082891,18.));
#37987=CARTESIAN_POINT('Ctrl Pts',(22.8426603964871,-1.90693261239855,0.));
#37988=CARTESIAN_POINT('Ctrl Pts',(22.8426603964871,-1.90693261239855,18.));
#37989=CARTESIAN_POINT('Ctrl Pts',(22.9190313507225,-1.86222218327819,0.));
#37990=CARTESIAN_POINT('Ctrl Pts',(22.9190313507225,-1.86222218327819,18.));
#37991=CARTESIAN_POINT('Ctrl Pts',(22.9952524859917,-1.81691265597281,0.));
#37992=CARTESIAN_POINT('Ctrl Pts',(22.9952524859917,-1.81691265597281,18.));
#37993=CARTESIAN_POINT('Ctrl Pts',(23.0713213684573,-1.77100780743078,0.));
#37994=CARTESIAN_POINT('Ctrl Pts',(23.0713213684573,-1.77100780743078,18.));
#37995=CARTESIAN_POINT('Ctrl Pts',(23.1472354850579,-1.72451136919382,0.));
#37996=CARTESIAN_POINT('Ctrl Pts',(23.1472354850579,-1.72451136919382,18.));
#37997=CARTESIAN_POINT('Ctrl Pts',(23.2229921402299,-1.67742712670823,0.));
#37998=CARTESIAN_POINT('Ctrl Pts',(23.2229921402299,-1.67742712670823,18.));
#37999=CARTESIAN_POINT('Ctrl Pts',(23.2985883089733,-1.62975905604583,0.));
#38000=CARTESIAN_POINT('Ctrl Pts',(23.2985883089733,-1.62975905604583,18.));
#38001=CARTESIAN_POINT('Ctrl Pts',(23.3740206492924,-1.58151133638847,0.));
#38002=CARTESIAN_POINT('Ctrl Pts',(23.3740206492924,-1.58151133638847,18.));
#38003=CARTESIAN_POINT('Ctrl Pts',(23.4492857841673,-1.53268814658653,0.));
#38004=CARTESIAN_POINT('Ctrl Pts',(23.4492857841673,-1.53268814658653,18.));
#38005=CARTESIAN_POINT('Ctrl Pts',(23.5243805284282,-1.48329351290851,0.));
#38006=CARTESIAN_POINT('Ctrl Pts',(23.5243805284282,-1.48329351290851,18.));
#38007=CARTESIAN_POINT('Ctrl Pts',(23.5993021272808,-1.4333311444639,0.));
#38008=CARTESIAN_POINT('Ctrl Pts',(23.5993021272808,-1.4333311444639,18.));
#38009=CARTESIAN_POINT('Ctrl Pts',(23.6740485197917,-1.38280426780156,0.));
#38010=CARTESIAN_POINT('Ctrl Pts',(23.6740485197917,-1.38280426780156,18.));
#38011=CARTESIAN_POINT('Ctrl Pts',(23.748618507953,-1.33171549586249,0.));
#38012=CARTESIAN_POINT('Ctrl Pts',(23.748618507953,-1.33171549586249,18.));
#38013=CARTESIAN_POINT('Ctrl Pts',(23.8230115078373,-1.28006684869166,0.));
#38014=CARTESIAN_POINT('Ctrl Pts',(23.8230115078373,-1.28006684869166,18.));
#38015=CARTESIAN_POINT('Ctrl Pts',(23.8823841929226,-1.2383011730893,0.));
#38016=CARTESIAN_POINT('Ctrl Pts',(23.8823841929226,-1.2383011730893,18.));
#38017=CARTESIAN_POINT('Ctrl Pts',(23.9268340213744,-1.20672599652272,0.));
#38018=CARTESIAN_POINT('Ctrl Pts',(23.9268340213744,-1.20672599652272,18.));
#38019=CARTESIAN_POINT('Ctrl Pts',(23.9564318364582,-1.18556439589232,0.));
#38020=CARTESIAN_POINT('Ctrl Pts',(23.9564318364582,-1.18556439589232,18.));
#38021=CARTESIAN_POINT('Ctrl Pts',(23.9712218930251,-1.17495572484832,0.));
#38022=CARTESIAN_POINT('Ctrl Pts',(23.9712218930251,-1.17495572484832,18.));
#38023=CARTESIAN_POINT('Origin',(0.,0.,0.));
#38024=CARTESIAN_POINT('',(0.,0.,0.));
#38025=CARTESIAN_POINT('Origin',(0.,1.73472347597681E-15,-6.67403582113016E-15));
#38026=CARTESIAN_POINT('',(1.52656933693714E-15,12.4653846153846,3.0875));
#38027=CARTESIAN_POINT('Origin',(0.,6.26866080313552E-16,3.0875));
#38028=CARTESIAN_POINT('',(-1.52656933693714E-15,12.4653846153846,-3.0875));
#38029=CARTESIAN_POINT('Origin',(-1.74512168878498E-15,14.25,-4.05635328795269E-15));
#38030=CARTESIAN_POINT('Origin',(0.,1.76119517802379E-15,-3.0875));
#38031=CARTESIAN_POINT('Origin',(0.,1.56496838953657E-16,5.64807088834312));
#38032=CARTESIAN_POINT('',(9.67029207191279E-16,7.64278544417155,5.99278544417156));
#38033=CARTESIAN_POINT('',(-9.35971273077467E-16,-7.64278544417155,5.99278544417156));
#38034=CARTESIAN_POINT('Origin',(0.,9.31738023414375E-17,5.99278544417156));
#38035=CARTESIAN_POINT('Origin',(0.,9.31738023414375E-17,5.99278544417156));
#38036=CARTESIAN_POINT('',(-9.18485099360515E-16,-7.5,5.64807088834312));
#38037=CARTESIAN_POINT('Origin',(-9.78186630818948E-16,-7.9875,5.64807088834312));
#38038=CARTESIAN_POINT('',(9.18485099360515E-16,7.5,5.64807088834312));
#38039=CARTESIAN_POINT('Origin',(0.,1.56496838953657E-16,5.64807088834312));
#38040=CARTESIAN_POINT('Origin',(0.,1.56496838953657E-16,5.64807088834312));
#38041=CARTESIAN_POINT('Origin',(0.,2.23156441938368E-15,-5.64807088834312));
#38042=CARTESIAN_POINT('',(9.18485099360515E-16,7.5,-5.64807088834312));
#38043=CARTESIAN_POINT('',(-9.18485099360515E-16,-7.5,-5.64807088834312));
#38044=CARTESIAN_POINT('Origin',(0.,2.23156441938368E-15,-5.64807088834312));
#38045=CARTESIAN_POINT('Origin',(0.,2.23156441938368E-15,-5.64807088834312));
#38046=CARTESIAN_POINT('',(-9.35971273077467E-16,-7.64278544417155,-5.99278544417156));
#38047=CARTESIAN_POINT('Origin',(-9.78186630818948E-16,-7.9875,-5.64807088834312));
#38048=CARTESIAN_POINT('Origin',(0.,2.2948874559959E-15,-5.99278544417156));
#38049=CARTESIAN_POINT('Origin',(0.,-9.99635681210842E-31,6.5));
#38050=CARTESIAN_POINT('',(-9.98087141305092E-16,8.14999999999999,6.50000000000001));
#38051=CARTESIAN_POINT('',(-9.98087141305092E-16,8.14999999999999,6.5));
#38052=CARTESIAN_POINT('Origin',(0.,-9.99635681210842E-31,6.5));
#38053=CARTESIAN_POINT('Origin',(0.,0.,6.5));
#38054=CARTESIAN_POINT('',(-9.18485099360515E-16,7.5,6.5));
#38055=CARTESIAN_POINT('Origin',(0.,2.26865819542047E-15,-5.85));
#38056=CARTESIAN_POINT('',(-9.98087141305091E-16,-8.14999999999998,-6.50000000000001));
#38057=CARTESIAN_POINT('',(-9.18485099360515E-16,-7.5,-5.85));
#38058=CARTESIAN_POINT('Origin',(0.,2.38806125833734E-15,-6.50000000000001));
#38059=CARTESIAN_POINT('Origin',(0.,0.,6.5));
#38060=CARTESIAN_POINT('',(-1.52656933693714E-15,12.4653846153846,-6.50000000000001));
#38061=CARTESIAN_POINT('',(-1.52656933693714E-15,12.4653846153846,6.5));
#38062=CARTESIAN_POINT('Origin',(0.,2.38806125833734E-15,-6.50000000000001));
#38063=CARTESIAN_POINT('Origin',(0.,0.,6.5));
#38064=CARTESIAN_POINT('',(-1.52656933693714E-15,12.4653846153846,6.50000000000001));
#38065=CARTESIAN_POINT('Origin',(0.,-1.17267830746035E-30,6.50000000000001));
#38066=CARTESIAN_POINT('',(-1.52656933693714E-15,12.4653846153846,6.5));
#38067=CARTESIAN_POINT('Origin',(0.,8.14999999999999,6.50000000000001));
#38068=CARTESIAN_POINT('Origin',(0.,8.14999999999999,-6.50000000000001));
#38069=CARTESIAN_POINT('Origin',(0.,14.25,-4.07195060716495E-15));
#38070=CARTESIAN_POINT('',(-3.56616156686793,14.25,-4.07195060716495E-15));
#38071=CARTESIAN_POINT('',(3.56616156686793,14.25,-4.07195060716495E-15));
#38072=CARTESIAN_POINT('Origin',(0.,14.25,-4.07195060716495E-15));
#38073=CARTESIAN_POINT('Origin',(11.1410986251694,8.88472967648693,-5.05753477640253E-15));
#38074=CARTESIAN_POINT('',(8.91763325644669,11.6728670610318,-4.54536224786764E-15));
#38075=CARTESIAN_POINT('',(13.3645639938921,6.09659229194206,-5.56970730493742E-15));
#38076=CARTESIAN_POINT('Origin',(11.1410986251694,8.88472967648693,-5.05753477640253E-15));
#38077=CARTESIAN_POINT('Origin',(13.892722748591,-3.17092330887753,-7.27212230242621E-15));
#38078=CARTESIAN_POINT('',(14.6862683510896,0.305827142012077,-6.6334536057588E-15));
#38079=CARTESIAN_POINT('',(13.0991771460924,-6.64767375976714,-7.91079099909362E-15));
#38080=CARTESIAN_POINT('Origin',(13.892722748591,-3.17092330887753,-7.27212230242621E-15));
#38081=CARTESIAN_POINT('Origin',(6.18284328242512,-12.8388063676095,-9.04808360878726E-15));
#38082=CARTESIAN_POINT('',(9.39584383208325,-11.2915068526795,-8.76384929904507E-15));
#38083=CARTESIAN_POINT('',(2.96984273276699,-14.3861058825395,-9.33231791852945E-15));
#38084=CARTESIAN_POINT('Origin',(6.18284328242512,-12.8388063676095,-9.04808360878726E-15));
#38085=CARTESIAN_POINT('Origin',(-6.1828432824253,-12.8388063676094,-9.04808360878725E-15));
#38086=CARTESIAN_POINT('',(-2.9698427327672,-14.3861058825394,-9.33231791852944E-15));
#38087=CARTESIAN_POINT('',(-9.39584383208341,-11.2915068526794,-8.76384929904506E-15));
#38088=CARTESIAN_POINT('Origin',(-6.1828432824253,-12.8388063676094,-9.04808360878725E-15));
#38089=CARTESIAN_POINT('Origin',(-13.892722748591,-3.17092330887735,-7.27212230242617E-15));
#38090=CARTESIAN_POINT('',(-13.0991771460925,-6.64767375976697,-7.91079099909359E-15));
#38091=CARTESIAN_POINT('',(-14.6862683510895,0.30582714201227,-6.63345360575876E-15));
#38092=CARTESIAN_POINT('Origin',(-13.892722748591,-3.17092330887735,-7.27212230242617E-15));
#38093=CARTESIAN_POINT('Origin',(-11.1410986251693,8.88472967648709,-5.0575347764025E-15));
#38094=CARTESIAN_POINT('',(-13.3645639938921,6.09659229194225,-5.56970730493739E-15));
#38095=CARTESIAN_POINT('',(-8.91763325644655,11.6728670610319,-4.54536224786761E-15));
#38096=CARTESIAN_POINT('Origin',(-11.1410986251693,8.88472967648709,-5.0575347764025E-15));
#38097=CARTESIAN_POINT('Origin',(0.,1.07462756625201E-17,6.44149999999999));
#38098=CARTESIAN_POINT('',(-1.99949495950787E-15,-16.3271153846154,6.49999999999999));
#38099=CARTESIAN_POINT('Origin',(0.,2.01169401222323E-30,6.49999999999999));
#38100=CARTESIAN_POINT('',(-1.99233077573286E-15,-16.2686153846154,6.44149999999999));
#38101=CARTESIAN_POINT('Origin',(-1.99949495950788E-15,-16.3271153846154,
6.44149999999999));
#38102=CARTESIAN_POINT('',(1.99233077573286E-15,16.2686153846154,6.44149999999999));
#38103=CARTESIAN_POINT('Origin',(0.,1.07462756625199E-17,6.44149999999999));
#38104=CARTESIAN_POINT('Origin',(0.,1.07462756625199E-17,6.44149999999999));
#38105=CARTESIAN_POINT('Origin',(0.,1.30149338579385E-16,5.7915));
#38106=CARTESIAN_POINT('',(-1.96367404063281E-15,16.0346153846154,5.7915));
#38107=CARTESIAN_POINT('Origin',(0.,1.30149338579385E-16,5.7915));
#38108=CARTESIAN_POINT('',(-1.97083822440782E-15,16.0931153846154,5.85));
#38109=CARTESIAN_POINT('Origin',(-1.97083822440783E-15,16.0931153846154,
5.7915));
#38110=CARTESIAN_POINT('Origin',(0.,1.19403062916867E-16,5.85));
#38111=CARTESIAN_POINT('Origin',(0.,2.37731498267482E-15,-6.44150000000001));
#38112=CARTESIAN_POINT('',(-1.99949495950787E-15,16.3271153846154,-6.5));
#38113=CARTESIAN_POINT('Origin',(0.,2.38806125833734E-15,-6.50000000000001));
#38114=CARTESIAN_POINT('',(-1.99233077573286E-15,16.2686153846154,-6.4415));
#38115=CARTESIAN_POINT('Origin',(-1.99949495950788E-15,16.3271153846154,
-6.44150000000001));
#38116=CARTESIAN_POINT('Origin',(0.,2.37731498267482E-15,-6.44150000000001));
#38117=CARTESIAN_POINT('Origin',(0.,2.25791191975795E-15,-5.7915));
#38118=CARTESIAN_POINT('',(1.96367404063281E-15,16.0346153846154,-5.7915));
#38119=CARTESIAN_POINT('',(-1.96367404063282E-15,-16.0346153846154,-5.7915));
#38120=CARTESIAN_POINT('Origin',(0.,2.25791191975795E-15,-5.7915));
#38121=CARTESIAN_POINT('Origin',(0.,2.25791191975795E-15,-5.7915));
#38122=CARTESIAN_POINT('',(-1.97083822440782E-15,-16.0931153846154,-5.85000000000001));
#38123=CARTESIAN_POINT('Origin',(-1.97083822440783E-15,-16.0931153846154,
-5.7915));
#38124=CARTESIAN_POINT('Origin',(0.,2.26865819542047E-15,-5.85));
#38125=CARTESIAN_POINT('Origin',(0.,0.,6.5));
#38126=CARTESIAN_POINT('',(-2.16636878649169E-15,17.6897435897436,5.85));
#38127=CARTESIAN_POINT('Origin',(0.,1.19403062916867E-16,5.85));
#38128=CARTESIAN_POINT('',(-2.16636878649169E-15,17.6897435897436,6.084));
#38129=CARTESIAN_POINT('',(-2.16636878649169E-15,17.6897435897436,6.5));
#38130=CARTESIAN_POINT('Origin',(0.,7.6417960266795E-17,6.084));
#38131=CARTESIAN_POINT('Origin',(0.,0.,6.5));
#38132=CARTESIAN_POINT('',(-1.99233077573286E-15,16.2686153846154,6.084));
#38133=CARTESIAN_POINT('Origin',(0.,7.6417960266795E-17,6.084));
#38134=CARTESIAN_POINT('',(-1.99233077573286E-15,16.2686153846154,6.5));
#38135=CARTESIAN_POINT('Origin',(0.,0.,6.5));
#38136=CARTESIAN_POINT('',(-1.96367404063281E-15,16.0346153846154,-3.0875));
#38137=CARTESIAN_POINT('',(-1.96367404063282E-15,16.0346153846154,6.5));
#38138=CARTESIAN_POINT('Origin',(0.,1.76119517802379E-15,-3.08750000000001));
#38139=CARTESIAN_POINT('Origin',(0.,1.73472347597681E-15,-6.67403582113016E-15));
#38140=CARTESIAN_POINT('',(-1.96367404063281E-15,16.0346153846154,3.0875));
#38141=CARTESIAN_POINT('Origin',(-1.74512168878498E-15,14.25,-4.05635328795269E-15));
#38142=CARTESIAN_POINT('Origin',(0.,6.26866080313552E-16,3.08749999999999));
#38143=CARTESIAN_POINT('Origin',(0.,0.,6.5));
#38144=CARTESIAN_POINT('',(-1.96367404063282E-15,16.0346153846154,6.5));
#38145=CARTESIAN_POINT('Origin',(0.,0.,6.5));
#38146=CARTESIAN_POINT('',(-1.99233077573286E-15,16.2686153846154,-6.084));
#38147=CARTESIAN_POINT('',(-1.99233077573286E-15,16.2686153846154,6.5));
#38148=CARTESIAN_POINT('Origin',(0.,2.31164329807054E-15,-6.084));
#38149=CARTESIAN_POINT('Origin',(0.,0.,6.5));
#38150=CARTESIAN_POINT('',(-2.16636878649169E-15,17.6897435897436,-6.084));
#38151=CARTESIAN_POINT('Origin',(0.,2.31164329807054E-15,-6.084));
#38152=CARTESIAN_POINT('',(-2.16636878649169E-15,17.6897435897436,-5.85));
#38153=CARTESIAN_POINT('',(-2.16636878649169E-15,17.6897435897436,6.5));
#38154=CARTESIAN_POINT('Origin',(0.,2.26865819542047E-15,-5.85));
#38155=CARTESIAN_POINT('Origin',(0.,2.38806125833734E-15,-6.50000000000001));
#38156=CARTESIAN_POINT('',(-2.57175827820944E-15,21.,-5.85));
#38157=CARTESIAN_POINT('Origin',(0.,2.26865819542047E-15,-5.85000000000001));
#38158=CARTESIAN_POINT('',(-2.49215623626487E-15,20.35,-6.5));
#38159=CARTESIAN_POINT('',(-2.49215623626486E-15,20.35,-6.50000000000001));
#38160=CARTESIAN_POINT('Origin',(0.,2.38806125833734E-15,-6.50000000000001));
#38161=CARTESIAN_POINT('Origin',(0.,1.19403062916869E-16,5.84999999999999));
#38162=CARTESIAN_POINT('',(2.57175827820944E-15,21.,5.84999999999999));
#38163=CARTESIAN_POINT('',(-2.57175827820944E-15,-21.,5.84999999999999));
#38164=CARTESIAN_POINT('Origin',(0.,1.19403062916869E-16,5.84999999999999));
#38165=CARTESIAN_POINT('',(-2.49215623626487E-15,-20.35,6.49999999999999));
#38166=CARTESIAN_POINT('',(-2.57175827820944E-15,-21.,5.84999999999999));
#38167=CARTESIAN_POINT('Origin',(0.,1.96135664184276E-30,6.49999999999999));
#38168=CARTESIAN_POINT('Origin',(0.,1.19403062916869E-16,5.84999999999999));
#38169=CARTESIAN_POINT('Origin',(0.,0.,6.5));
#38170=CARTESIAN_POINT('',(-2.57175827820944E-15,21.,6.5));
#38171=CARTESIAN_POINT('Origin',(0.,20.35,6.49999999999999));
#38172=CARTESIAN_POINT('Origin',(0.,20.35,-6.5));
#38173=CARTESIAN_POINT('Origin',(0.,16.0346153846154,-5.85));
#38174=CARTESIAN_POINT('Origin',(0.,16.2686153846154,-6.084));
#38175=CARTESIAN_POINT('Origin',(0.,16.2686153846154,6.084));
#38176=CARTESIAN_POINT('Origin',(0.,16.0346153846154,5.85));
#38177=CARTESIAN_POINT('Origin',(-11.1410986251694,8.88472967648693,-9.85584169237584E-16));
#38178=CARTESIAN_POINT('',(-11.838732871064,9.44107442276088,-3.96060240207311));
#38179=CARTESIAN_POINT('Origin',(-11.838732871064,9.44107442276088,-1.04729956121144E-15));
#38180=CARTESIAN_POINT('',(-10.4434643792749,8.32838493021299,-3.96060240207311));
#38181=CARTESIAN_POINT('Origin',(-11.1410986251694,8.88472967648693,-2.5198520116158));
#38182=CARTESIAN_POINT('Origin',(-10.4434643792749,8.32838493021299,-9.23868777263733E-16));
#38183=CARTESIAN_POINT('',(-13.176267261227,5.42664547033602,1.08333333333333));
#38184=CARTESIAN_POINT('',(-13.9269936544441,5.94376395877182,1.08333333333333));
#38185=CARTESIAN_POINT('Ctrl Pts',(-13.176267261227,5.42664547033603,1.08333333333333));
#38186=CARTESIAN_POINT('Ctrl Pts',(-13.3544742809805,5.48608062863209,1.08333333333333));
#38187=CARTESIAN_POINT('Ctrl Pts',(-13.5395781511317,5.58798093945111,1.08333333333333));
#38188=CARTESIAN_POINT('Ctrl Pts',(-13.7657237213497,5.76832601371359,1.08333333333333));
#38189=CARTESIAN_POINT('Ctrl Pts',(-13.851789663848,5.85187873682469,1.08333333333333));
#38190=CARTESIAN_POINT('Ctrl Pts',(-13.9269936544446,5.9437639587714,1.08333333333333));
#38191=CARTESIAN_POINT('',(-13.176267261227,5.42664547033602,-1.08333333333333));
#38192=CARTESIAN_POINT('Ctrl Pts',(-13.176267261227,5.426645470336,1.08333333333333));
#38193=CARTESIAN_POINT('Ctrl Pts',(-13.1893705593041,5.39482976422217,0.949270311030458));
#38194=CARTESIAN_POINT('Ctrl Pts',(-13.1999097963793,5.36892368585873,0.813521288367943));
#38195=CARTESIAN_POINT('Ctrl Pts',(-13.2079621630869,5.34904061477063,0.676607052100963));
#38196=CARTESIAN_POINT('Ctrl Pts',(-13.2148460430323,5.33204279546006,0.559560573777783));
#38197=CARTESIAN_POINT('Ctrl Pts',(-13.2199117356377,5.31944645364942,0.441662516279014));
#38198=CARTESIAN_POINT('Ctrl Pts',(-13.2231796369648,5.31131059989529,0.323238258334693));
#38199=CARTESIAN_POINT('Ctrl Pts',(-13.2269557156994,5.30190957419894,0.186398348762648));
#38200=CARTESIAN_POINT('Ctrl Pts',(-13.2283213471704,5.29849241313602,0.0492519096262365));
#38201=CARTESIAN_POINT('Ctrl Pts',(-13.2273014856384,5.30103720115478,-0.0876758270660023));
#38202=CARTESIAN_POINT('Ctrl Pts',(-13.2262786675027,5.30358936657696,-0.225000520654269));
#38203=CARTESIAN_POINT('Ctrl Pts',(-13.2228564747501,5.31213809759637,-0.362105241912721));
#38204=CARTESIAN_POINT('Ctrl Pts',(-13.21701132539,5.32664168351063,-0.498460177595569));
#38205=CARTESIAN_POINT('Ctrl Pts',(-13.2111409592134,5.34120783998416,-0.635403368116636));
#38206=CARTESIAN_POINT('Ctrl Pts',(-13.2028266475275,5.36178038996277,-0.771590289741212));
#38207=CARTESIAN_POINT('Ctrl Pts',(-13.1919958930595,5.38829698119001,-0.90648424252654));
#38208=CARTESIAN_POINT('Ctrl Pts',(-13.1872415508606,5.39993688577963,-0.965698216399817));
#38209=CARTESIAN_POINT('Ctrl Pts',(-13.1820016856382,5.4127218947045,-1.02466304565395));
#38210=CARTESIAN_POINT('Ctrl Pts',(-13.176267261227,5.426645470336,-1.08333333333333));
#38211=CARTESIAN_POINT('',(-13.9269936544455,5.94376395877242,-1.08333333333333));
#38212=CARTESIAN_POINT('Ctrl Pts',(-13.176267261227,5.42664547033603,-1.08333333333333));
#38213=CARTESIAN_POINT('Ctrl Pts',(-13.3544742809805,5.48608062863209,-1.08333333333333));
#38214=CARTESIAN_POINT('Ctrl Pts',(-13.5395781511317,5.58798093945111,-1.08333333333333));
#38215=CARTESIAN_POINT('Ctrl Pts',(-13.76572372135,5.76832601371385,-1.08333333333333));
#38216=CARTESIAN_POINT('Ctrl Pts',(-13.8517896638487,5.85187873682532,-1.08333333333333));
#38217=CARTESIAN_POINT('Ctrl Pts',(-13.9269936544455,5.94376395877245,-1.08333333333333));
#38218=CARTESIAN_POINT('Ctrl Pts',(-13.9269936544444,5.94376395877114,-1.08333333333355));
#38219=CARTESIAN_POINT('Ctrl Pts',(-13.9416885168396,5.90933203032471,-0.95688863210348));
#38220=CARTESIAN_POINT('Ctrl Pts',(-13.9536527109306,5.88095561854246,-0.828820583351296));
#38221=CARTESIAN_POINT('Ctrl Pts',(-13.9629765258054,5.85873440158612,-0.699646919261824));
#38222=CARTESIAN_POINT('Ctrl Pts',(-13.9722513158078,5.83663002439321,-0.571152453813156));
#38223=CARTESIAN_POINT('Ctrl Pts',(-13.9789135007646,5.82061622745832,-0.441563969171476));
#38224=CARTESIAN_POINT('Ctrl Pts',(-13.9830050237945,5.81077040959789,-0.311391073637591));
#38225=CARTESIAN_POINT('Ctrl Pts',(-13.9870637119681,5.80100360534983,-0.182262827807202));
#38226=CARTESIAN_POINT('Ctrl Pts',(-13.9885928700523,5.79730615639837,-0.0525595133518154));
#38227=CARTESIAN_POINT('Ctrl Pts',(-13.9875862925321,5.79973378332902,0.0772214321948836));
#38228=CARTESIAN_POINT('Ctrl Pts',(-13.9868997670034,5.80138952054624,0.16573715053464));
#38229=CARTESIAN_POINT('Ctrl Pts',(-13.9850326975558,5.80589410253377,0.25428898113034));
#38230=CARTESIAN_POINT('Ctrl Pts',(-13.9819702480149,5.81325986277477,0.342719102199523));
#38231=CARTESIAN_POINT('Ctrl Pts',(-13.9773533484511,5.82436436418404,0.476034927301742));
#38232=CARTESIAN_POINT('Ctrl Pts',(-13.9700489046451,5.84190742581559,0.608312350205735));
#38233=CARTESIAN_POINT('Ctrl Pts',(-13.9600480872369,5.86570879353503,0.739057191237609));
#38234=CARTESIAN_POINT('Ctrl Pts',(-13.9511688384278,5.8868408927778,0.855139299994326));
#38235=CARTESIAN_POINT('Ctrl Pts',(-13.9401632237806,5.9129059856334,0.970013302477931));
#38236=CARTESIAN_POINT('Ctrl Pts',(-13.9269936544444,5.94376395877114,1.08333333333355));
#38237=CARTESIAN_POINT('',(-8.89378902201695,12.2552029391753,1.08333333333333));
#38238=CARTESIAN_POINT('',(-8.22258343557141,11.6383685130291,1.08333333333333));
#38239=CARTESIAN_POINT('Ctrl Pts',(-8.89378902201693,12.2552029391753,1.08333333333333));
#38240=CARTESIAN_POINT('Ctrl Pts',(-8.78747309219938,12.2023308550396,1.08333333333333));
#38241=CARTESIAN_POINT('Ctrl Pts',(-8.68686373639314,12.1370149953911,1.08333333333333));
#38242=CARTESIAN_POINT('Ctrl Pts',(-8.46071816617524,11.9566699211287,1.08333333333333));
#38243=CARTESIAN_POINT('Ctrl Pts',(-8.32018322283281,11.7988819437994,1.08333333333333));
#38244=CARTESIAN_POINT('Ctrl Pts',(-8.22258343557192,11.6383685130288,1.08333333333333));
#38245=CARTESIAN_POINT('',(-8.89378902201695,12.2552029391753,-1.08333333333333));
#38246=CARTESIAN_POINT('Ctrl Pts',(-8.89378902201696,12.2552029391753,1.08333333333333));
#38247=CARTESIAN_POINT('Ctrl Pts',(-8.86325700199161,12.2773604951023,0.955915065626613));
#38248=CARTESIAN_POINT('Ctrl Pts',(-8.83806624000395,12.2954729083691,0.8267015714506));
#38249=CARTESIAN_POINT('Ctrl Pts',(-8.81837639229442,12.3095783864577,0.696211209492237));
#38250=CARTESIAN_POINT('Ctrl Pts',(-8.79899689851553,12.3234615321731,0.567777653525536));
#38251=CARTESIAN_POINT('Ctrl Pts',(-8.7849462329058,12.3334631509294,0.438107164856251));
#38252=CARTESIAN_POINT('Ctrl Pts',(-8.77634666705863,12.3395794672318,0.307693975181527));
#38253=CARTESIAN_POINT('Ctrl Pts',(-8.76960830208466,12.3443720314467,0.205506064179221));
#38254=CARTESIAN_POINT('Ctrl Pts',(-8.76621624622179,12.3467783236356,0.102862147741002));
#38255=CARTESIAN_POINT('Ctrl Pts',(-8.76621624622179,12.3467783236356,-2.44249065417534E-15));
#38256=CARTESIAN_POINT('Ctrl Pts',(-8.76621624622179,12.3467783236356,-0.130666807305558));
#38257=CARTESIAN_POINT('Ctrl Pts',(-8.77169236507929,12.3428956683044,-0.261069786498707));
#38258=CARTESIAN_POINT('Ctrl Pts',(-8.78256611126601,12.3351536167882,-0.390710450871087));
#38259=CARTESIAN_POINT('Ctrl Pts',(-8.79357042167237,12.3273186042172,-0.521907748246256));
#38260=CARTESIAN_POINT('Ctrl Pts',(-8.8101027782242,12.315530900308,-0.652324314224256));
#38261=CARTESIAN_POINT('Ctrl Pts',(-8.83205039902736,12.2997710546807,-0.781443489202971));
#38262=CARTESIAN_POINT('Ctrl Pts',(-8.84930597782606,12.2873804060307,-0.882959098491573));
#38263=CARTESIAN_POINT('Ctrl Pts',(-8.86990830867396,12.2725335396739,-0.983672743459536));
#38264=CARTESIAN_POINT('Ctrl Pts',(-8.89378902201696,12.2552029391753,-1.08333333333333));
#38265=CARTESIAN_POINT('',(-8.22258343557665,11.6383685130365,-1.08333333333333));
#38266=CARTESIAN_POINT('Ctrl Pts',(-8.89378902201693,12.2552029391753,-1.08333333333333));
#38267=CARTESIAN_POINT('Ctrl Pts',(-8.78747309219938,12.2023308550396,-1.08333333333333));
#38268=CARTESIAN_POINT('Ctrl Pts',(-8.68686373639314,12.1370149953911,-1.08333333333333));
#38269=CARTESIAN_POINT('Ctrl Pts',(-8.46071816617751,11.9566699211305,-1.08333333333333));
#38270=CARTESIAN_POINT('Ctrl Pts',(-8.32018322283717,11.7988819438045,-1.08333333333333));
#38271=CARTESIAN_POINT('Ctrl Pts',(-8.22258343557662,11.6383685130365,-1.08333333333333));
#38272=CARTESIAN_POINT('Ctrl Pts',(-8.22258343557191,11.6383685130287,-1.08333333333318));
#38273=CARTESIAN_POINT('Ctrl Pts',(-8.19455490688727,11.6581708517696,-0.949622058007629));
#38274=CARTESIAN_POINT('Ctrl Pts',(-8.17172113698899,11.6741565633286,-0.814376693553349));
#38275=CARTESIAN_POINT('Ctrl Pts',(-8.15417398891324,11.6864000683928,-0.678132403728345));
#38276=CARTESIAN_POINT('Ctrl Pts',(-8.13671023659264,11.698585384152,-0.542535637671064));
#38277=CARTESIAN_POINT('Ctrl Pts',(-8.12448291951145,11.7070640382822,-0.405949418799179));
#38278=CARTESIAN_POINT('Ctrl Pts',(-8.11755242812626,11.7118675955896,-0.268901316712111));
#38279=CARTESIAN_POINT('Ctrl Pts',(-8.11302715126356,11.7150040870061,-0.179415511018989));
#38280=CARTESIAN_POINT('Ctrl Pts',(-8.11075954642953,11.7165728598427,-0.0897327832367744));
#38281=CARTESIAN_POINT('Ctrl Pts',(-8.11075954642953,11.7165728598427,-9.99200722162641E-15));
#38282=CARTESIAN_POINT('Ctrl Pts',(-8.11075954642954,11.7165728598427,0.137573936980354));
#38283=CARTESIAN_POINT('Ctrl Pts',(-8.11609005089583,11.7128881555246,0.274951212619692));
#38284=CARTESIAN_POINT('Ctrl Pts',(-8.12669452775723,11.7055258768037,0.4116124062147));
#38285=CARTESIAN_POINT('Ctrl Pts',(-8.13738105388554,11.6981066344457,0.549330978772881));
#38286=CARTESIAN_POINT('Ctrl Pts',(-8.15342350530942,11.6869526399855,0.686322345437031));
#38287=CARTESIAN_POINT('Ctrl Pts',(-8.17473347641523,11.6720277839618,0.822054935347404));
#38288=CARTESIAN_POINT('Ctrl Pts',(-8.18849695174643,11.662388264195,0.909720570537357));
#38289=CARTESIAN_POINT('Ctrl Pts',(-8.20445714658991,11.6511748546878,0.996861109122827));
#38290=CARTESIAN_POINT('Ctrl Pts',(-8.22258343557191,11.6383685130287,1.08333333333318));
#38291=CARTESIAN_POINT('Origin',(-11.1410986251694,8.88472967648693,-9.85584169237584E-16));
#38292=CARTESIAN_POINT('',(-13.6377879061429,6.58029051604744,-1.08333333333333));
#38293=CARTESIAN_POINT('',(-13.2594869773434,6.22835470309403,-1.08333333333333));
#38294=CARTESIAN_POINT('Origin',(-11.1410986251694,8.88472967648693,-1.08333333333333));
#38295=CARTESIAN_POINT('',(-9.02271027299537,11.5411046498798,-1.08333333333333));
#38296=CARTESIAN_POINT('Origin',(-11.1410986251694,8.88472967648693,-9.85584169237584E-16));
#38297=CARTESIAN_POINT('',(-9.45000219633307,11.8316076987796,-1.08333333333333));
#38298=CARTESIAN_POINT('Origin',(-11.1410986251694,8.88472967648693,-1.08333333333333));
#38299=CARTESIAN_POINT('',(-9.45000219633307,11.8316076987796,1.08333333333333));
#38300=CARTESIAN_POINT('Ctrl Pts',(-9.45000219633306,11.8316076987796,-1.08333333333334));
#38301=CARTESIAN_POINT('Ctrl Pts',(-9.35474240837113,11.9076924734257,-0.727666221822799));
#38302=CARTESIAN_POINT('Ctrl Pts',(-9.30796390402501,11.9436715548398,-0.352782973842778));
#38303=CARTESIAN_POINT('Ctrl Pts',(-9.30796390402501,11.9436715548398,-5.10741104345864E-16));
#38304=CARTESIAN_POINT('Ctrl Pts',(-9.30796390402501,11.9436715548398,0.352782973842777));
#38305=CARTESIAN_POINT('Ctrl Pts',(-9.35474240837113,11.9076924734257,0.727666221822798));
#38306=CARTESIAN_POINT('Ctrl Pts',(-9.45000219633306,11.8316076987796,1.08333333333334));
#38307=CARTESIAN_POINT('',(-8.72113759169224,11.2696166353063,1.08333333333333));
#38308=CARTESIAN_POINT('Origin',(-11.1410986251694,8.88472967648693,1.08333333333333));
#38309=CARTESIAN_POINT('',(-8.72113759169224,11.2696166353063,-1.08333333333333));
#38310=CARTESIAN_POINT('Ctrl Pts',(-8.72113759169222,11.2696166353063,1.08333333333334));
#38311=CARTESIAN_POINT('Ctrl Pts',(-8.63036626326988,11.3398611937656,0.725928647976584));
#38312=CARTESIAN_POINT('Ctrl Pts',(-8.58623309669495,11.3727349924818,0.352039859176991));
#38313=CARTESIAN_POINT('Ctrl Pts',(-8.58623309669495,11.3727349924818,-4.46574186955748E-16));
#38314=CARTESIAN_POINT('Ctrl Pts',(-8.58623309669495,11.3727349924818,-0.352039859176992));
#38315=CARTESIAN_POINT('Ctrl Pts',(-8.63036626326988,11.3398611937656,-0.725928647976585));
#38316=CARTESIAN_POINT('Ctrl Pts',(-8.72113759169222,11.2696166353063,-1.08333333333334));
#38317=CARTESIAN_POINT('Origin',(-11.1410986251694,8.88472967648693,-1.08333333333333));
#38318=CARTESIAN_POINT('',(-12.9276994994136,5.99475484510091,-1.08333333333333));
#38319=CARTESIAN_POINT('Origin',(-11.1410986251694,8.88472967648693,-1.08333333333333));
#38320=CARTESIAN_POINT('',(-12.9276994994136,5.99475484510091,1.08333333333333));
#38321=CARTESIAN_POINT('Ctrl Pts',(-12.9276994994136,5.99475484510092,-1.08333333333333));
#38322=CARTESIAN_POINT('Ctrl Pts',(-12.9759843593574,5.89062845864246,-0.725928647976576));
#38323=CARTESIAN_POINT('Ctrl Pts',(-12.9982133898606,5.84028669430256,-0.352039859176989));
#38324=CARTESIAN_POINT('Ctrl Pts',(-12.9982133898606,5.84028669430256,0.352039859176986));
#38325=CARTESIAN_POINT('Ctrl Pts',(-12.9759843593574,5.89062845864246,0.725928647976574));
#38326=CARTESIAN_POINT('Ctrl Pts',(-12.9276994994136,5.99475484510092,1.08333333333332));
#38327=CARTESIAN_POINT('',(-13.6377879061429,6.58029051604744,1.08333333333333));
#38328=CARTESIAN_POINT('Origin',(-11.1410986251694,8.88472967648693,1.08333333333333));
#38329=CARTESIAN_POINT('Ctrl Pts',(-13.6377879061429,6.58029051604746,1.08333333333332));
#38330=CARTESIAN_POINT('Ctrl Pts',(-13.6907677796516,6.47048863474076,0.727666221822783));
#38331=CARTESIAN_POINT('Ctrl Pts',(-13.7154355939007,6.41687686636447,0.352782973842769));
#38332=CARTESIAN_POINT('Ctrl Pts',(-13.7154355939007,6.41687686636447,-0.352782973842771));
#38333=CARTESIAN_POINT('Ctrl Pts',(-13.6907677796516,6.47048863474076,-0.727666221822784));
#38334=CARTESIAN_POINT('Ctrl Pts',(-13.6377879061429,6.58029051604746,-1.08333333333332));
#38335=CARTESIAN_POINT('',(-10.4434643792749,8.32838493021299,3.45272288248773));
#38336=CARTESIAN_POINT('Origin',(-10.4434643792749,8.32838493021299,-9.23868777263733E-16));
#38337=CARTESIAN_POINT('',(-11.838732871064,9.44107442276088,3.45272288248773));
#38338=CARTESIAN_POINT('Origin',(-11.838732871064,9.44107442276088,-1.04729956121144E-15));
#38339=CARTESIAN_POINT('Origin',(-13.892722748591,-3.17092330887753,-3.20017169526126E-15));
#38340=CARTESIAN_POINT('',(-14.7626584240763,-3.36948044994625,-3.96060240207311));
#38341=CARTESIAN_POINT('Origin',(-14.7626584240763,-3.36948044994625,-3.40056031423578E-15));
#38342=CARTESIAN_POINT('',(-13.0227870731057,-2.97236616780882,-3.96060240207311));
#38343=CARTESIAN_POINT('Origin',(-13.892722748591,-3.17092330887753,-2.5198520116158));
#38344=CARTESIAN_POINT('Origin',(-13.0227870731057,-2.97236616780882,-2.99978307628674E-15));
#38345=CARTESIAN_POINT('',(-12.4579905368413,-6.91816245718267,1.08333333333333));
#38346=CARTESIAN_POINT('',(-13.3303603014234,-7.18268588222789,1.08333333333333));
#38347=CARTESIAN_POINT('Ctrl Pts',(-12.4579905368413,-6.91816245718265,
1.08333333333333));
#38348=CARTESIAN_POINT('Ctrl Pts',(-12.6155690741986,-7.02043310055334,
1.08333333333333));
#38349=CARTESIAN_POINT('Ctrl Pts',(-12.8106483205941,-7.10161932916232,
1.08333333333333));
#38350=CARTESIAN_POINT('Ctrl Pts',(-13.0926472341269,-7.16598374096129,
1.08333333333333));
#38351=CARTESIAN_POINT('Ctrl Pts',(-13.211632620936,-7.18117853359748,1.08333333333333));
#38352=CARTESIAN_POINT('Ctrl Pts',(-13.3303603014234,-7.18268588222786,
1.08333333333333));
#38353=CARTESIAN_POINT('',(-12.4579905368413,-6.91816245718267,-1.08333333333334));
#38354=CARTESIAN_POINT('Ctrl Pts',(-12.4579905368413,-6.91816245718269,
1.08333333333333));
#38355=CARTESIAN_POINT('Ctrl Pts',(-12.4412857888864,-6.94824379644449,
0.949270311030495));
#38356=CARTESIAN_POINT('Ctrl Pts',(-12.4276027080703,-6.97263587945683,
0.813521288368019));
#38357=CARTESIAN_POINT('Ctrl Pts',(-12.4170780656485,-6.99132836531023,
0.676607052101084));
#38358=CARTESIAN_POINT('Ctrl Pts',(-12.4080806643214,-7.0073083663671,0.559560573777871));
#38359=CARTESIAN_POINT('Ctrl Pts',(-12.4013908554087,-7.01912257498617,
0.441662516279072));
#38360=CARTESIAN_POINT('Ctrl Pts',(-12.3970674919579,-7.02675014497037,
0.323238258334728));
#38361=CARTESIAN_POINT('Ctrl Pts',(-12.392071820683,-7.03556384585404,0.186398348762656));
#38362=CARTESIAN_POINT('Ctrl Pts',(-12.3902516338786,-7.03876210460556,
0.0492519096262199));
#38363=CARTESIAN_POINT('Ctrl Pts',(-12.3916053560034,-7.03637809537454,
-0.0876758270660418));
#38364=CARTESIAN_POINT('Ctrl Pts',(-12.3929630026022,-7.03398717484178,
-0.22500052065431));
#38365=CARTESIAN_POINT('Ctrl Pts',(-12.3975129673671,-7.02598155019929,
-0.36210524191276));
#38366=CARTESIAN_POINT('Ctrl Pts',(-12.4052079364271,-7.0123687905019,-0.498460177595606));
#38367=CARTESIAN_POINT('Ctrl Pts',(-12.4129361026924,-6.99869730339788,
-0.635403368116707));
#38368=CARTESIAN_POINT('Ctrl Pts',(-12.4238364813948,-6.97937013765694,
-0.771590289741313));
#38369=CARTESIAN_POINT('Ctrl Pts',(-12.4378151222667,-6.9543694886247,-0.906484242526672));
#38370=CARTESIAN_POINT('Ctrl Pts',(-12.4439512822522,-6.94339503240897,
-0.965698216399908));
#38371=CARTESIAN_POINT('Ctrl Pts',(-12.450680002204,-6.93132701813286,-1.024663045654));
#38372=CARTESIAN_POINT('Ctrl Pts',(-12.4579905368413,-6.91816245718269,
-1.08333333333334));
#38373=CARTESIAN_POINT('',(-13.3303603014234,-7.18268588222787,-1.08333333333334));
#38374=CARTESIAN_POINT('Ctrl Pts',(-12.4579905368413,-6.91816245718265,
-1.08333333333333));
#38375=CARTESIAN_POINT('Ctrl Pts',(-12.6150882655077,-7.02012104908378,
-1.08333333333333));
#38376=CARTESIAN_POINT('Ctrl Pts',(-12.8106174809568,-7.10161229021636,
-1.08333333333333));
#38377=CARTESIAN_POINT('Ctrl Pts',(-13.0925863122299,-7.16596983593587,
-1.08333333333333));
#38378=CARTESIAN_POINT('Ctrl Pts',(-13.2116839714656,-7.18117918553602,
-1.08333333333333));
#38379=CARTESIAN_POINT('Ctrl Pts',(-13.3303603014234,-7.18268588222786,
-1.08333333333333));
#38380=CARTESIAN_POINT('Ctrl Pts',(-13.3303603014234,-7.18268588222788,
-1.08333333333333));
#38381=CARTESIAN_POINT('Ctrl Pts',(-13.312602432605,-7.21564274452362,-0.9568886321034));
#38382=CARTESIAN_POINT('Ctrl Pts',(-13.2978764135175,-7.24268913148589,
-0.828820583351364));
#38383=CARTESIAN_POINT('Ctrl Pts',(-13.2863164700111,-7.26383348564883,
-0.699646919262042));
#38384=CARTESIAN_POINT('Ctrl Pts',(-13.2748173090022,-7.28486666222222,
-0.571152453813466));
#38385=CARTESIAN_POINT('Ctrl Pts',(-13.2664510227833,-7.30005980724142,
-0.441563969171881));
#38386=CARTESIAN_POINT('Ctrl Pts',(-13.2613042752926,-7.30939745578436,
-0.311391073638092));
#38387=CARTESIAN_POINT('Ctrl Pts',(-13.2561988309335,-7.3186601688214,-0.182262827807686));
#38388=CARTESIAN_POINT('Ctrl Pts',(-13.2542614634094,-7.32216103446744,
-0.0525595133522827));
#38389=CARTESIAN_POINT('Ctrl Pts',(-13.2555318677528,-7.31986045983868,
0.0772214321944347));
#38390=CARTESIAN_POINT('Ctrl Pts',(-13.2563983335701,-7.31829137729732,
0.165737150534351));
#38391=CARTESIAN_POINT('Ctrl Pts',(-13.2587560588234,-7.31402308269238,
0.254288981130211));
#38392=CARTESIAN_POINT('Ctrl Pts',(-13.2626054360146,-7.30703628683457,
0.342719102199554));
#38393=CARTESIAN_POINT('Ctrl Pts',(-13.2684086950193,-7.29650310602083,
0.476034927301584));
#38394=CARTESIAN_POINT('Ctrl Pts',(-13.2775701666804,-7.27985434187078,
0.608312350205395));
#38395=CARTESIAN_POINT('Ctrl Pts',(-13.2899434176249,-7.25719547792734,
0.739057191237093));
#38396=CARTESIAN_POINT('Ctrl Pts',(-13.3009290370229,-7.23707775329796,
0.855139299993907));
#38397=CARTESIAN_POINT('Ctrl Pts',(-13.3144456587151,-7.21222189770289,
0.970013302477609));
#38398=CARTESIAN_POINT('Ctrl Pts',(-13.3303603014234,-7.18268588222788,
1.08333333333332));
#38399=CARTESIAN_POINT('',(-15.1266902369927,0.68754979644356,1.08333333333333));
#38400=CARTESIAN_POINT('',(-14.2259398250621,0.827729480997533,1.08333333333333));
#38401=CARTESIAN_POINT('Ctrl Pts',(-15.1266902369927,0.687549796443589,
1.08333333333333));
#38402=CARTESIAN_POINT('Ctrl Pts',(-15.0191128271494,0.737684039417719,
1.08333333333333));
#38403=CARTESIAN_POINT('Ctrl Pts',(-14.905210454464,0.775655426636244,1.08333333333333));
#38404=CARTESIAN_POINT('Ctrl Pts',(-14.6232416231909,0.840012972355744,
1.08333333333333));
#38405=CARTESIAN_POINT('Ctrl Pts',(-14.411718162898,0.851428848194329,1.08333333333333));
#38406=CARTESIAN_POINT('Ctrl Pts',(-14.2259398250622,0.827729480996923,
1.08333333333333));
#38407=CARTESIAN_POINT('',(-15.1266902369927,0.687549796443561,-1.08333333333334));
#38408=CARTESIAN_POINT('Ctrl Pts',(-15.1266902369927,0.687549796443564,
1.08333333333333));
#38409=CARTESIAN_POINT('Ctrl Pts',(-15.1249773086751,0.725235701077295,
0.955915065626697));
#38410=CARTESIAN_POINT('Ctrl Pts',(-15.1234319803901,0.756223536825465,
0.826701571450772));
#38411=CARTESIAN_POINT('Ctrl Pts',(-15.122183667988,0.780412301388329,0.696211209492499));
#38412=CARTESIAN_POINT('Ctrl Pts',(-15.1209550316477,0.804219799510246,
0.567777653525797));
#38413=CARTESIAN_POINT('Ctrl Pts',(-15.12001416535,0.821440959530219,0.438107164856512));
#38414=CARTESIAN_POINT('Ctrl Pts',(-15.1194343523859,0.83197783168462,0.307693975181787));
#38415=CARTESIAN_POINT('Ctrl Pts',(-15.1189800281283,0.840234212474348,
0.205506064179395));
#38416=CARTESIAN_POINT('Ctrl Pts',(-15.1187464308798,0.844386527178334,
0.102862147741089));
#38417=CARTESIAN_POINT('Ctrl Pts',(-15.1187464308798,0.844386527178334,
-1.99840144432528E-15));
#38418=CARTESIAN_POINT('Ctrl Pts',(-15.1187464308798,0.844386527178334,
-0.130666807305563));
#38419=CARTESIAN_POINT('Ctrl Pts',(-15.1191251529677,0.837684329050672,
-0.261069786498716));
#38420=CARTESIAN_POINT('Ctrl Pts',(-15.1198518432089,0.824355801783686,
-0.3907104508711));
#38421=CARTESIAN_POINT('Ctrl Pts',(-15.1205872590302,0.810867235029684,
-0.521907748246278));
#38422=CARTESIAN_POINT('Ctrl Pts',(-15.1216790167187,0.790592205023353,
-0.652324314224286));
#38423=CARTESIAN_POINT('Ctrl Pts',(-15.1230415909943,0.763606761086714,
-0.78144348920301));
#38424=CARTESIAN_POINT('Ctrl Pts',(-15.1241128691977,0.742390363261972,
-0.882959098491598));
#38425=CARTESIAN_POINT('Ctrl Pts',(-15.1253504648421,0.717025942629857,
-0.983672743459549));
#38426=CARTESIAN_POINT('Ctrl Pts',(-15.1266902369927,0.687549796443564,
-1.08333333333333));
#38427=CARTESIAN_POINT('',(-14.2259398250711,0.827729480998061,-1.08333333333334));
#38428=CARTESIAN_POINT('Ctrl Pts',(-15.1266902369927,0.687549796443589,
-1.08333333333333));
#38429=CARTESIAN_POINT('Ctrl Pts',(-15.0191128271494,0.73768403941772,-1.08333333333333));
#38430=CARTESIAN_POINT('Ctrl Pts',(-14.905210454464,0.775655426636245,-1.08333333333333));
#38431=CARTESIAN_POINT('Ctrl Pts',(-14.6232416231937,0.840012972355103,
-1.08333333333333));
#38432=CARTESIAN_POINT('Ctrl Pts',(-14.4117181629048,0.851428848194163,
-1.08333333333333));
#38433=CARTESIAN_POINT('Ctrl Pts',(-14.2259398250711,0.827729480998062,
-1.08333333333333));
#38434=CARTESIAN_POINT('Ctrl Pts',(-14.2259398250621,0.827729480996948,
-1.08333333333319));
#38435=CARTESIAN_POINT('Ctrl Pts',(-14.2239464151202,0.86198962338768,-0.949622058007746));
#38436=CARTESIAN_POINT('Ctrl Pts',(-14.2222079250172,0.889808711690097,
-0.814376693553578));
#38437=CARTESIAN_POINT('Ctrl Pts',(-14.2208398148552,0.911161325029729,
-0.678132403728685));
#38438=CARTESIAN_POINT('Ctrl Pts',(-14.2194782068654,0.932412456504284,
-0.542535637671376));
#38439=CARTESIAN_POINT('Ctrl Pts',(-14.2184834780892,0.947258512328182,
-0.405949418799462));
#38440=CARTESIAN_POINT('Ctrl Pts',(-14.2179179597194,0.955671957675903,
-0.268901316712362));
#38441=CARTESIAN_POINT('Ctrl Pts',(-14.2175487034788,0.961165532005871,
-0.179415511019154));
#38442=CARTESIAN_POINT('Ctrl Pts',(-14.2173613909827,0.963916530719958,
-0.0897327832368514));
#38443=CARTESIAN_POINT('Ctrl Pts',(-14.2173613909827,0.963916530719958,
1.77635683940025E-15));
#38444=CARTESIAN_POINT('Ctrl Pts',(-14.2173613909827,0.963916530719959,
0.137573936980362));
#38445=CARTESIAN_POINT('Ctrl Pts',(-14.2178040883167,0.957451598945575,
0.274951212619699));
#38446=CARTESIAN_POINT('Ctrl Pts',(-14.2186598102071,0.944570379379332,
0.411612406214706));
#38447=CARTESIAN_POINT('Ctrl Pts',(-14.2195221530139,0.931589494866292,
0.549330978772852));
#38448=CARTESIAN_POINT('Ctrl Pts',(-14.2208039138492,0.912092599491199,
0.686322345436968));
#38449=CARTESIAN_POINT('Ctrl Pts',(-14.222421741201,0.886126297665223,0.82205493534731));
#38450=CARTESIAN_POINT('Ctrl Pts',(-14.2234666476786,0.869355437073727,
0.909720570537294));
#38451=CARTESIAN_POINT('Ctrl Pts',(-14.2246506698206,0.849885807806941,
0.996861109122796));
#38452=CARTESIAN_POINT('Ctrl Pts',(-14.2259398250621,0.827729480996951,
1.08333333333318));
#38453=CARTESIAN_POINT('Origin',(-13.892722748591,-3.17092330887753,-3.20017169526126E-15));
#38454=CARTESIAN_POINT('',(-13.6476999686241,-6.55970790622096,-1.08333333333334));
#38455=CARTESIAN_POINT('',(-13.1366786991091,-6.483368720524,-1.08333333333334));
#38456=CARTESIAN_POINT('Origin',(-13.892722748591,-3.17092330887753,-1.08333333333334));
#38457=CARTESIAN_POINT('',(-14.6487667980729,0.141522102768936,-1.08333333333334));
#38458=CARTESIAN_POINT('Origin',(-13.892722748591,-3.17092330887753,-3.20017169526126E-15));
#38459=CARTESIAN_POINT('',(-15.1423033840733,-0.0114224867028857,-1.08333333333334));
#38460=CARTESIAN_POINT('Origin',(-13.892722748591,-3.17092330887753,-1.08333333333334));
#38461=CARTESIAN_POINT('',(-15.1423033840733,-0.0114224867028862,1.08333333333333));
#38462=CARTESIAN_POINT('Ctrl Pts',(-15.1423033840733,-0.0114224867028739,
-1.08333333333334));
#38463=CARTESIAN_POINT('Ctrl Pts',(-15.1423953499066,0.110492695607543,
-0.727666221822802));
#38464=CARTESIAN_POINT('Ctrl Pts',(-15.1413590080604,0.169498193350012,
-0.352782973842781));
#38465=CARTESIAN_POINT('Ctrl Pts',(-15.1413590080604,0.169498193350012,
-2.67362166230902E-15));
#38466=CARTESIAN_POINT('Ctrl Pts',(-15.1413590080604,0.169498193350012,
0.352782973842775));
#38467=CARTESIAN_POINT('Ctrl Pts',(-15.1423953499066,0.110492695607543,
0.727666221822795));
#38468=CARTESIAN_POINT('Ctrl Pts',(-15.1423033840733,-0.0114224867028737,
1.08333333333334));
#38469=CARTESIAN_POINT('',(-14.2484814298548,0.20803111085057,1.08333333333333));
#38470=CARTESIAN_POINT('Origin',(-13.892722748591,-3.17092330887754,1.08333333333333));
#38471=CARTESIAN_POINT('',(-14.2484814298548,0.208031110850571,-1.08333333333334));
#38472=CARTESIAN_POINT('Ctrl Pts',(-14.2484814298548,0.208031110850584,
1.08333333333333));
#38473=CARTESIAN_POINT('Ctrl Pts',(-14.2468058395578,0.322795758952019,
0.725928647976579));
#38474=CARTESIAN_POINT('Ctrl Pts',(-14.2449910310593,0.37779693624925,0.352039859176988));
#38475=CARTESIAN_POINT('Ctrl Pts',(-14.2449910310593,0.37779693624925,-2.46631154156404E-15));
#38476=CARTESIAN_POINT('Ctrl Pts',(-14.2449910310593,0.37779693624925,-0.352039859176994));
#38477=CARTESIAN_POINT('Ctrl Pts',(-14.2468058395578,0.322795758952019,
-0.725928647976587));
#38478=CARTESIAN_POINT('Ctrl Pts',(-14.2484814298548,0.208031110850583,
-1.08333333333334));
#38479=CARTESIAN_POINT('Origin',(-13.892722748591,-3.17092330887753,-1.08333333333334));
#38480=CARTESIAN_POINT('',(-12.7471768669563,-6.36961395396413,-1.08333333333334));
#38481=CARTESIAN_POINT('Origin',(-13.892722748591,-3.17092330887753,-1.08333333333334));
#38482=CARTESIAN_POINT('',(-12.7471768669563,-6.36961395396413,1.08333333333333));
#38483=CARTESIAN_POINT('Ctrl Pts',(-12.7471768669563,-6.36961395396412,
-1.08333333333334));
#38484=CARTESIAN_POINT('Ctrl Pts',(-12.6958726976266,-6.472286317656,-0.725928647976585));
#38485=CARTESIAN_POINT('Ctrl Pts',(-12.6703734952066,-6.52105325020167,
-0.352039859176994));
#38486=CARTESIAN_POINT('Ctrl Pts',(-12.6703734952066,-6.52105325020167,
0.352039859176985));
#38487=CARTESIAN_POINT('Ctrl Pts',(-12.6958726976266,-6.472286317656,0.725928647976577));
#38488=CARTESIAN_POINT('Ctrl Pts',(-12.7471768669563,-6.36961395396412,
1.08333333333333));
#38489=CARTESIAN_POINT('',(-13.6476999686241,-6.55970790622096,1.08333333333333));
#38490=CARTESIAN_POINT('Origin',(-13.892722748591,-3.17092330887754,1.08333333333333));
#38491=CARTESIAN_POINT('Ctrl Pts',(-13.6476999686241,-6.55970790622096,
1.08333333333332));
#38492=CARTESIAN_POINT('Ctrl Pts',(-13.5948858118208,-6.66958959248691,
0.727666221822788));
#38493=CARTESIAN_POINT('Ctrl Pts',(-13.5683505740919,-6.72230205711272,
0.35278297384277));
#38494=CARTESIAN_POINT('Ctrl Pts',(-13.5683505740919,-6.72230205711272,
-0.352782973842779));
#38495=CARTESIAN_POINT('Ctrl Pts',(-13.5948858118208,-6.66958959248691,
-0.727666221822796));
#38496=CARTESIAN_POINT('Ctrl Pts',(-13.6476999686241,-6.55970790622096,
-1.08333333333333));
#38497=CARTESIAN_POINT('',(-13.0227870731057,-2.97236616780882,3.45272288248773));
#38498=CARTESIAN_POINT('Origin',(-13.0227870731057,-2.97236616780882,-2.99978307628674E-15));
#38499=CARTESIAN_POINT('',(-14.7626584240763,-3.36948044994625,3.45272288248773));
#38500=CARTESIAN_POINT('Origin',(-14.7626584240763,-3.36948044994625,-3.40056031423578E-15));
#38501=CARTESIAN_POINT('Origin',(-6.18284328242512,-12.8388063676095,-4.97613300162231E-15));
#38502=CARTESIAN_POINT('',(-6.57000108040694,-13.6427478189686,-3.96060240207311));
#38503=CARTESIAN_POINT('Origin',(-6.57000108040694,-13.6427478189686,-5.28772891427451E-15));
#38504=CARTESIAN_POINT('',(-5.79568548444331,-12.0348649162504,-3.96060240207311));
#38505=CARTESIAN_POINT('Origin',(-6.18284328242512,-12.8388063676095,-2.51985201161581));
#38506=CARTESIAN_POINT('Origin',(-5.79568548444331,-12.0348649162504,-4.66453708897012E-15));
#38507=CARTESIAN_POINT('',(-2.35859284151935,-14.0534529496467,1.08333333333333));
#38508=CARTESIAN_POINT('',(-2.69569375163562,-14.9004267538186,1.08333333333333));
#38509=CARTESIAN_POINT('Ctrl Pts',(-2.35859284151934,-14.0534529496467,
1.08333333333333));
#38510=CARTESIAN_POINT('Ctrl Pts',(-2.37682723618162,-14.2398470420046,
1.08333333333333));
#38511=CARTESIAN_POINT('Ctrl Pts',(-2.43502529011671,-14.4435268961719,
1.08333333333332));
#38512=CARTESIAN_POINT('Ctrl Pts',(-2.56051322547963,-14.7041052789647,
1.08333333333333));
#38513=CARTESIAN_POINT('Ctrl Pts',(-2.62287825309305,-14.806702452812,1.08333333333333));
#38514=CARTESIAN_POINT('Ctrl Pts',(-2.69569375163558,-14.9004267538186,
1.08333333333333));
#38515=CARTESIAN_POINT('',(-2.35859284151935,-14.0534529496467,-1.08333333333334));
#38516=CARTESIAN_POINT('Ctrl Pts',(-2.35859284151935,-14.0534529496467,
1.08333333333333));
#38517=CARTESIAN_POINT('Ctrl Pts',(-2.32474809698527,-14.0591331175362,
0.949622058007895));
#38518=CARTESIAN_POINT('Ctrl Pts',(-2.29723964086638,-14.0636285445206,
0.814376693553736));
#38519=CARTESIAN_POINT('Ctrl Pts',(-2.27611794897253,-14.0670461391994,
0.678132403728853));
#38520=CARTESIAN_POINT('Ctrl Pts',(-2.25509664145098,-14.0704474911881,
0.542535637671543));
#38521=CARTESIAN_POINT('Ctrl Pts',(-2.24040145926613,-14.0727812605466,
0.405949418799629));
#38522=CARTESIAN_POINT('Ctrl Pts',(-2.23207311688321,-14.0741020886196,
0.268901316712528));
#38523=CARTESIAN_POINT('Ctrl Pts',(-2.22663511068775,-14.0749645256946,
0.179415511019263));
#38524=CARTESIAN_POINT('Ctrl Pts',(-2.2239114043034,-14.075394064317,0.0897327832369026));
#38525=CARTESIAN_POINT('Ctrl Pts',(-2.2239114043034,-14.075394064317,-8.43769498715119E-15));
#38526=CARTESIAN_POINT('Ctrl Pts',(-2.2239114043034,-14.075394064317,-0.137573936980349));
#38527=CARTESIAN_POINT('Ctrl Pts',(-2.23031275616482,-14.0743870796481,
-0.274951212619667));
#38528=CARTESIAN_POINT('Ctrl Pts',(-2.24306143269717,-14.0723550057958,
-0.411612406214657));
#38529=CARTESIAN_POINT('Ctrl Pts',(-2.25590874866049,-14.0703072093226,
-0.549330978772813));
#38530=CARTESIAN_POINT('Ctrl Pts',(-2.27520203478074,-14.0672183663696,
-0.68632234543694));
#38531=CARTESIAN_POINT('Ctrl Pts',(-2.30087730766032,-14.0630175856782,
-0.822054935347292));
#38532=CARTESIAN_POINT('Ctrl Pts',(-2.31746020132759,-14.0603044266067,
-0.909720570537337));
#38533=CARTESIAN_POINT('Ctrl Pts',(-2.33670515605249,-14.0571263627534,
-0.996861109122898));
#38534=CARTESIAN_POINT('Ctrl Pts',(-2.35859284151935,-14.0534529496467,
-1.08333333333334));
#38535=CARTESIAN_POINT('',(-2.69569375163563,-14.9004267538187,-1.08333333333334));
#38536=CARTESIAN_POINT('Ctrl Pts',(-2.35859284151934,-14.0534529496467,
-1.08333333333333));
#38537=CARTESIAN_POINT('Ctrl Pts',(-2.37688304383397,-14.2404175142851,
-1.08333333333333));
#38538=CARTESIAN_POINT('Ctrl Pts',(-2.43503901504648,-14.4435553962822,
-1.08333333333334));
#38539=CARTESIAN_POINT('Ctrl Pts',(-2.56054033827446,-14.7041615792632,
-1.08333333333334));
#38540=CARTESIAN_POINT('Ctrl Pts',(-2.62284674626764,-14.8066618988743,
-1.08333333333334));
#38541=CARTESIAN_POINT('Ctrl Pts',(-2.69569375163563,-14.9004267538187,
-1.08333333333334));
#38542=CARTESIAN_POINT('Ctrl Pts',(-2.69569375163559,-14.9004267538186,
-1.08333333333335));
#38543=CARTESIAN_POINT('Ctrl Pts',(-2.65857154890325,-14.9071426748862,
-0.955915065626573));
#38544=CARTESIAN_POINT('Ctrl Pts',(-2.628016775001,-14.9125315333598,-0.826701571450498));
#38545=CARTESIAN_POINT('Ctrl Pts',(-2.60415669762586,-14.9166970252376,
-0.696211209492072));
#38546=CARTESIAN_POINT('Ctrl Pts',(-2.58067270588166,-14.9207968600927,
-0.567777653525379));
#38547=CARTESIAN_POINT('Ctrl Pts',(-2.56367395385075,-14.923711651889,-0.438107164856101));
#38548=CARTESIAN_POINT('Ctrl Pts',(-2.55327224255806,-14.9254910506792,
-0.307693975181385));
#38549=CARTESIAN_POINT('Ctrl Pts',(-2.54512176981446,-14.9268853348437,
-0.205506064179128));
#38550=CARTESIAN_POINT('Ctrl Pts',(-2.54102158203148,-14.9275815713119,
-0.102862147740959));
#38551=CARTESIAN_POINT('Ctrl Pts',(-2.54102158203148,-14.9275815713119,
-4.44089209850063E-15));
#38552=CARTESIAN_POINT('Ctrl Pts',(-2.54102158203148,-14.9275815713119,
0.130666807305524));
#38553=CARTESIAN_POINT('Ctrl Pts',(-2.54764001565181,-14.9264594186595,
0.261069786498646));
#38554=CARTESIAN_POINT('Ctrl Pts',(-2.56079607270382,-14.9242020129234,
0.390710450870999));
#38555=CARTESIAN_POINT('Ctrl Pts',(-2.57411009834303,-14.9219175018628,
0.521907748246163));
#38556=CARTESIAN_POINT('Ctrl Pts',(-2.59411972995703,-14.9184702682937,
0.652324314224157));
#38557=CARTESIAN_POINT('Ctrl Pts',(-2.62073179377387,-14.9137938537994,
0.781443489202868));
#38558=CARTESIAN_POINT('Ctrl Pts',(-2.64165463403551,-14.9101171801624,
0.882959098491507));
#38559=CARTESIAN_POINT('Ctrl Pts',(-2.66665850662476,-14.9056796321318,
0.983672743459509));
#38560=CARTESIAN_POINT('Ctrl Pts',(-2.69569375163559,-14.9004267538186,
1.08333333333334));
#38561=CARTESIAN_POINT('',(-9.96888517526507,-11.3978423664701,1.08333333333333));
#38562=CARTESIAN_POINT('',(-9.516873369993,-10.6062067328295,1.08333333333333));
#38563=CARTESIAN_POINT('Ctrl Pts',(-9.96888517526507,-11.3978423664701,
1.08333333333333));
#38564=CARTESIAN_POINT('Ctrl Pts',(-9.94100828682427,-11.282476771434,1.08333333333333));
#38565=CARTESIAN_POINT('Ctrl Pts',(-9.89967854500783,-11.1697495378475,
1.08333333333333));
#38566=CARTESIAN_POINT('Ctrl Pts',(-9.77419060964491,-10.9091711550547,
1.08333333333333));
#38567=CARTESIAN_POINT('Ctrl Pts',(-9.65123318042897,-10.7366777723525,
1.08333333333333));
#38568=CARTESIAN_POINT('Ctrl Pts',(-9.51687336999256,-10.6062067328299,
1.08333333333333));
#38569=CARTESIAN_POINT('',(-9.96888517526507,-11.3978423664701,-1.08333333333334));
#38570=CARTESIAN_POINT('Ctrl Pts',(-9.96888517526508,-11.3978423664701,
1.08333333333333));
#38571=CARTESIAN_POINT('Ctrl Pts',(-9.99706424266063,-11.3731961327199,
0.956888632103256));
#38572=CARTESIAN_POINT('Ctrl Pts',(-10.020155672713,-11.3528209383891,0.828820583351071));
#38573=CARTESIAN_POINT('Ctrl Pts',(-10.038197564346,-11.3368457653652,0.699646919261599));
#38574=CARTESIAN_POINT('Ctrl Pts',(-10.0561445912219,-11.3209545902358,
0.571152453812953));
#38575=CARTESIAN_POINT('Ctrl Pts',(-10.0690951385517,-11.3094172714603,
0.441563969171296));
#38576=CARTESIAN_POINT('Ctrl Pts',(-10.0770534136919,-11.3023217413999,
0.311391073637437));
#38577=CARTESIAN_POINT('Ctrl Pts',(-10.0849478229272,-11.2952831536342,
0.182262827807044));
#38578=CARTESIAN_POINT('Ctrl Pts',(-10.0879298097314,-11.2926153440655,
0.0525595133516554));
#38579=CARTESIAN_POINT('Ctrl Pts',(-10.0859696068728,-11.2943658227348,
-0.0772214321950453));
#38580=CARTESIAN_POINT('Ctrl Pts',(-10.0846326712896,-11.2955597181575,
-0.165737150534751));
#38581=CARTESIAN_POINT('Ctrl Pts',(-10.0809960349672,-11.2988081152181,
-0.2542889811304));
#38582=CARTESIAN_POINT('Ctrl Pts',(-10.0750409796764,-11.304115688826,-0.342719102199531));
#38583=CARTESIAN_POINT('Ctrl Pts',(-10.0660632343107,-11.3121173012435,
-0.476034927301883));
#38584=CARTESIAN_POINT('Ctrl Pts',(-10.0518705086679,-11.3247537742305,
-0.608312350206005));
#38585=CARTESIAN_POINT('Ctrl Pts',(-10.0325330571073,-11.3418588735079,
-0.739057191238004));
#38586=CARTESIAN_POINT('Ctrl Pts',(-10.0153642561251,-11.3570456753652,
-0.855139299994515));
#38587=CARTESIAN_POINT('Ctrl Pts',(-9.99413932000721,-11.3757543553326,
-0.970013302477919));
#38588=CARTESIAN_POINT('Ctrl Pts',(-9.96888517526508,-11.3978423664701,
-1.08333333333334));
#38589=CARTESIAN_POINT('',(-9.51687336999906,-10.6062067328363,-1.08333333333334));
#38590=CARTESIAN_POINT('Ctrl Pts',(-9.96888517526507,-11.3978423664701,
-1.08333333333333));
#38591=CARTESIAN_POINT('Ctrl Pts',(-9.94100828682427,-11.282476771434,-1.08333333333333));
#38592=CARTESIAN_POINT('Ctrl Pts',(-9.89967854500783,-11.1697495378475,
-1.08333333333333));
#38593=CARTESIAN_POINT('Ctrl Pts',(-9.77419060964618,-10.9091711550573,
-1.08333333333333));
#38594=CARTESIAN_POINT('Ctrl Pts',(-9.6512331804331,-10.7366777723579,-1.08333333333333));
#38595=CARTESIAN_POINT('Ctrl Pts',(-9.51687336999908,-10.6062067328363,
-1.08333333333333));
#38596=CARTESIAN_POINT('Ctrl Pts',(-9.51687336999256,-10.6062067328299,
-1.08333333333319));
#38597=CARTESIAN_POINT('Ctrl Pts',(-9.54248335115827,-10.5832270800755,
-0.949270311030248));
#38598=CARTESIAN_POINT('Ctrl Pts',(-9.56321910180067,-10.5644593135702,
-0.813521288367661));
#38599=CARTESIAN_POINT('Ctrl Pts',(-9.57910097474595,-10.5500390764974,
-0.676607052100613));
#38600=CARTESIAN_POINT('Ctrl Pts',(-9.59267821366648,-10.5377113740467,
-0.559560573777554));
#38601=CARTESIAN_POINT('Ctrl Pts',(-9.6027075928823,-10.5285603838747,-0.44166251627891));
#38602=CARTESIAN_POINT('Ctrl Pts',(-9.6091818848891,-10.5226481221753,-0.323238258334718));
#38603=CARTESIAN_POINT('Ctrl Pts',(-9.61666296645239,-10.5158164698571,
-0.186398348762648));
#38604=CARTESIAN_POINT('Ctrl Pts',(-9.61937600851194,-10.5133302394117,
-0.0492519096262118));
#38605=CARTESIAN_POINT('Ctrl Pts',(-9.61735300288125,-10.5151805128572,
0.08767582706605));
#38606=CARTESIAN_POINT('Ctrl Pts',(-9.61532413250719,-10.5170361502911,
0.225000520654331));
#38607=CARTESIAN_POINT('Ctrl Pts',(-9.60853168799772,-10.5232534570122,
0.362105241912796));
#38608=CARTESIAN_POINT('Ctrl Pts',(-9.59697252030892,-10.5337846211338,
0.498460177595657));
#38609=CARTESIAN_POINT('Ctrl Pts',(-9.5853634847053,-10.5443612182148,0.635403368116659));
#38610=CARTESIAN_POINT('Ctrl Pts',(-9.56894645381043,-10.5592890006364,
0.771590289741169));
#38611=CARTESIAN_POINT('Ctrl Pts',(-9.54768316346852,-10.578480335569,0.906484242526434));
#38612=CARTESIAN_POINT('Ctrl Pts',(-9.53834928383367,-10.5869046954593,
0.965698216399696));
#38613=CARTESIAN_POINT('Ctrl Pts',(-9.52808112091929,-10.5961500981613,
1.02466304565381));
#38614=CARTESIAN_POINT('Ctrl Pts',(-9.51687336999256,-10.6062067328299,
1.08333333333318));
#38615=CARTESIAN_POINT('Origin',(-6.18284328242512,-12.8388063676095,-4.97613300162231E-15));
#38616=CARTESIAN_POINT('',(-3.38061559238688,-14.7601124814492,-1.08333333333334));
#38617=CARTESIAN_POINT('',(-3.12168342103518,-14.3129832609672,-1.08333333333334));
#38618=CARTESIAN_POINT('Origin',(-6.18284328242512,-12.8388063676095,-1.08333333333334));
#38619=CARTESIAN_POINT('',(-9.24400314381506,-11.3646294742518,-1.08333333333334));
#38620=CARTESIAN_POINT('Origin',(-6.18284328242512,-12.8388063676095,-4.97613300162231E-15));
#38621=CARTESIAN_POINT('',(-9.43214127690829,-11.8458513067218,-1.08333333333334));
#38622=CARTESIAN_POINT('Origin',(-6.18284328242512,-12.8388063676095,-1.08333333333334));
#38623=CARTESIAN_POINT('',(-9.43214127690829,-11.8458513067218,1.08333333333333));
#38624=CARTESIAN_POINT('Ctrl Pts',(-9.43214127690829,-11.8458513067218,
-1.08333333333333));
#38625=CARTESIAN_POINT('Ctrl Pts',(-9.52751574438859,-11.7699103356433,
-0.727666221822795));
#38626=CARTESIAN_POINT('Ctrl Pts',(-9.57300195158999,-11.7323107648653,
-0.352782973842778));
#38627=CARTESIAN_POINT('Ctrl Pts',(-9.57300195158999,-11.7323107648653,
-4.85994849902029E-15));
#38628=CARTESIAN_POINT('Ctrl Pts',(-9.57300195158999,-11.7323107648653,
0.352782973842767));
#38629=CARTESIAN_POINT('Ctrl Pts',(-9.52751574438859,-11.7699103356433,
0.727666221822782));
#38630=CARTESIAN_POINT('Ctrl Pts',(-9.43214127690829,-11.8458513067218,
1.08333333333332));
#38631=CARTESIAN_POINT('',(-9.04642813528379,-11.0102060831369,1.08333333333333));
#38632=CARTESIAN_POINT('Origin',(-6.18284328242512,-12.8388063676095,1.08333333333333));
#38633=CARTESIAN_POINT('',(-9.04642813528379,-11.0102060831369,-1.08333333333334));
#38634=CARTESIAN_POINT('Ctrl Pts',(-9.0464281352838,-11.0102060831369,1.08333333333332));
#38635=CARTESIAN_POINT('Ctrl Pts',(-9.13511003678158,-10.9373414661859,
0.725928647976571));
#38636=CARTESIAN_POINT('Ctrl Pts',(-9.17698017417422,-10.901629918632,0.352039859176983));
#38637=CARTESIAN_POINT('Ctrl Pts',(-9.17698017417422,-10.901629918632,-4.5383086406711E-15));
#38638=CARTESIAN_POINT('Ctrl Pts',(-9.17698017417422,-10.901629918632,-0.352039859176993));
#38639=CARTESIAN_POINT('Ctrl Pts',(-9.13511003678158,-10.9373414661859,
-0.725928647976581));
#38640=CARTESIAN_POINT('Ctrl Pts',(-9.0464281352838,-11.0102060831369,-1.08333333333333));
#38641=CARTESIAN_POINT('Origin',(-6.18284328242512,-12.8388063676095,-1.08333333333334));
#38642=CARTESIAN_POINT('',(-2.96777005865995,-13.9375335292483,-1.08333333333334));
#38643=CARTESIAN_POINT('Origin',(-6.18284328242512,-12.8388063676095,-1.08333333333334));
#38644=CARTESIAN_POINT('',(-2.96777005865995,-13.9375335292483,1.08333333333333));
#38645=CARTESIAN_POINT('Ctrl Pts',(-2.96777005865994,-13.9375335292483,
-1.08333333333334));
#38646=CARTESIAN_POINT('Ctrl Pts',(-2.85550994597631,-13.9614374861791,
-0.725928647976589));
#38647=CARTESIAN_POINT('Ctrl Pts',(-2.80148393014434,-13.9719070920595,
-0.352039859176996));
#38648=CARTESIAN_POINT('Ctrl Pts',(-2.80148393014434,-13.9719070920595,
0.352039859176986));
#38649=CARTESIAN_POINT('Ctrl Pts',(-2.85550994597631,-13.9614374861791,
0.725928647976578));
#38650=CARTESIAN_POINT('Ctrl Pts',(-2.96777005865994,-13.9375335292483,
1.08333333333333));
#38651=CARTESIAN_POINT('',(-3.38061559238688,-14.7601124814492,1.08333333333333));
#38652=CARTESIAN_POINT('Origin',(-6.18284328242512,-12.8388063676095,1.08333333333333));
#38653=CARTESIAN_POINT('Ctrl Pts',(-3.38061559238688,-14.7601124814492,
1.08333333333333));
#38654=CARTESIAN_POINT('Ctrl Pts',(-3.26177754255684,-14.7873308217382,
0.727666221822789));
#38655=CARTESIAN_POINT('Ctrl Pts',(-3.20402082808,-14.799450421612,0.35278297384277));
#38656=CARTESIAN_POINT('Ctrl Pts',(-3.20402082808,-14.799450421612,-0.352782973842781));
#38657=CARTESIAN_POINT('Ctrl Pts',(-3.26177754255684,-14.7873308217382,
-0.727666221822799));
#38658=CARTESIAN_POINT('Ctrl Pts',(-3.38061559238688,-14.7601124814492,
-1.08333333333334));
#38659=CARTESIAN_POINT('',(-5.79568548444331,-12.0348649162504,3.45272288248773));
#38660=CARTESIAN_POINT('Origin',(-5.79568548444331,-12.0348649162504,-4.66453708897012E-15));
#38661=CARTESIAN_POINT('',(-6.57000108040694,-13.6427478189686,3.45272288248772));
#38662=CARTESIAN_POINT('Origin',(-6.57000108040694,-13.6427478189686,-5.28772891427451E-15));
#38663=CARTESIAN_POINT('Origin',(6.1828432824253,-12.8388063676094,-4.9761330016223E-15));
#38664=CARTESIAN_POINT('',(6.57000108040713,-13.6427478189685,-3.96060240207311));
#38665=CARTESIAN_POINT('Origin',(6.57000108040713,-13.6427478189685,-5.28772891427449E-15));
#38666=CARTESIAN_POINT('',(5.79568548444348,-12.0348649162503,-3.96060240207311));
#38667=CARTESIAN_POINT('Origin',(6.1828432824253,-12.8388063676094,-2.51985201161581));
#38668=CARTESIAN_POINT('Origin',(5.79568548444348,-12.0348649162504,-4.66453708897011E-15));
#38669=CARTESIAN_POINT('',(9.51687336999268,-10.6062067328298,1.08333333333333));
#38670=CARTESIAN_POINT('',(9.96888517526453,-11.3978423664706,1.08333333333333));
#38671=CARTESIAN_POINT('Ctrl Pts',(9.5168733699927,-10.6062067328298,1.08333333333333));
#38672=CARTESIAN_POINT('Ctrl Pts',(9.65164439811578,-10.737077088181,1.08333333333333));
#38673=CARTESIAN_POINT('Ctrl Pts',(9.77420433457484,-10.9091996551649,1.08333333333333));
#38674=CARTESIAN_POINT('Ctrl Pts',(9.89970565780286,-11.169805838146,1.08333333333333));
#38675=CARTESIAN_POINT('Ctrl Pts',(9.94099622466366,-11.2824268534395,1.08333333333333));
#38676=CARTESIAN_POINT('Ctrl Pts',(9.96888517526534,-11.3978423664704,1.08333333333333));
#38677=CARTESIAN_POINT('',(9.51687336999268,-10.6062067328298,-1.08333333333334));
#38678=CARTESIAN_POINT('Ctrl Pts',(9.51687336999268,-10.6062067328298,1.08333333333333));
#38679=CARTESIAN_POINT('Ctrl Pts',(9.54241615713793,-10.5832873727889,0.949622058007762));
#38680=CARTESIAN_POINT('Ctrl Pts',(9.56308206533645,-10.5645832486408,0.814376693553466));
#38681=CARTESIAN_POINT('Ctrl Pts',(9.5789232079445,-10.5502004803844,0.678132403728444));
#38682=CARTESIAN_POINT('Ctrl Pts',(9.59468906287363,-10.5358860686389,0.542535637671145));
#38683=CARTESIAN_POINT('Ctrl Pts',(9.60567597345963,-10.5258519939611,0.405949418799242));
#38684=CARTESIAN_POINT('Ctrl Pts',(9.61190127497217,-10.5201641565229,0.268901316712153));
#38685=CARTESIAN_POINT('Ctrl Pts',(9.61596609683434,-10.5164502727984,0.179415511019018));
#38686=CARTESIAN_POINT('Ctrl Pts',(9.61800012680612,-10.5145886063487,0.0897327832367887));
#38687=CARTESIAN_POINT('Ctrl Pts',(9.61800012680612,-10.5145886063487,9.32587340685131E-15));
#38688=CARTESIAN_POINT('Ctrl Pts',(9.61800012680612,-10.5145886063487,-0.137573936980381));
#38689=CARTESIAN_POINT('Ctrl Pts',(9.61322165688595,-10.5189655400926,-0.274951212619743));
#38690=CARTESIAN_POINT('Ctrl Pts',(9.6036842477684,-10.5276658794419,-0.411612406214774));
#38691=CARTESIAN_POINT('Ctrl Pts',(9.59407304553156,-10.5364335353099,-0.54933097877281));
#38692=CARTESIAN_POINT('Ctrl Pts',(9.57962892372621,-10.5495917717182,-0.686322345436814));
#38693=CARTESIAN_POINT('Ctrl Pts',(9.5603363503304,-10.5670463644555,-0.822054935347047));
#38694=CARTESIAN_POINT('Ctrl Pts',(9.54787585206456,-10.5783197657831,-0.909720570537174));
#38695=CARTESIAN_POINT('Ctrl Pts',(9.5333921086825,-10.5913845868635,-0.996861109122817));
#38696=CARTESIAN_POINT('Ctrl Pts',(9.51687336999268,-10.6062067328298,-1.08333333333334));
#38697=CARTESIAN_POINT('',(9.9688851752657,-11.3978423664719,-1.08333333333334));
#38698=CARTESIAN_POINT('Ctrl Pts',(9.5168733699927,-10.6062067328298,-1.08333333333333));
#38699=CARTESIAN_POINT('Ctrl Pts',(9.65123318042911,-10.7366777723523,-1.08333333333333));
#38700=CARTESIAN_POINT('Ctrl Pts',(9.77419060964506,-10.9091711550545,-1.08333333333333));
#38701=CARTESIAN_POINT('Ctrl Pts',(9.89967854500826,-11.1697495378479,-1.08333333333333));
#38702=CARTESIAN_POINT('Ctrl Pts',(9.94100828682489,-11.2824767714351,-1.08333333333333));
#38703=CARTESIAN_POINT('Ctrl Pts',(9.96888517526571,-11.3978423664719,-1.08333333333333));
#38704=CARTESIAN_POINT('Ctrl Pts',(9.96888517526519,-11.39784236647,-1.08333333333359));
#38705=CARTESIAN_POINT('Ctrl Pts',(9.99728120861575,-11.3730063679711,-0.955915065626921));
#38706=CARTESIAN_POINT('Ctrl Pts',(10.0205449777511,-11.3524775820965,-0.826701571450959));
#38707=CARTESIAN_POINT('Ctrl Pts',(10.038678205356,-11.3364201641361,-0.696211209492648));
#38708=CARTESIAN_POINT('Ctrl Pts',(10.0565256146782,-11.3206158452779,-0.567777653525928));
#38709=CARTESIAN_POINT('Ctrl Pts',(10.0694030392049,-11.309143028737,-0.438107164856624));
#38710=CARTESIAN_POINT('Ctrl Pts',(10.0772795901119,-11.3021200803759,-0.307693975181881));
#38711=CARTESIAN_POINT('Ctrl Pts',(10.0834514220032,-11.2966171061454,-0.20550606417946));
#38712=CARTESIAN_POINT('Ctrl Pts',(10.0865521868617,-11.2938455465903,-0.102862147741125));
#38713=CARTESIAN_POINT('Ctrl Pts',(10.0865521868617,-11.2938455465903,-4.44089209850063E-15));
#38714=CARTESIAN_POINT('Ctrl Pts',(10.0865521868617,-11.2938455465903,0.130666807305562));
#38715=CARTESIAN_POINT('Ctrl Pts',(10.0815483267233,-11.2983203956244,0.261069786498721));
#38716=CARTESIAN_POINT('Ctrl Pts',(10.0715807484455,-11.3071987457576,0.390710450871112));
#38717=CARTESIAN_POINT('Ctrl Pts',(10.0614934865685,-11.3161837008123,0.521907748246463));
#38718=CARTESIAN_POINT('Ctrl Pts',(10.0463225295865,-11.3296785457857,0.652324314224642));
#38719=CARTESIAN_POINT('Ctrl Pts',(10.0260740111135,-11.3475689983448,0.781443489203535));
#38720=CARTESIAN_POINT('Ctrl Pts',(10.0101542943843,-11.3616347650465,0.88295909849203));
#38721=CARTESIAN_POINT('Ctrl Pts',(9.99109522006272,-11.3784168138781,0.983672743459888));
#38722=CARTESIAN_POINT('Ctrl Pts',(9.96888517526519,-11.39784236647,1.08333333333358));
#38723=CARTESIAN_POINT('',(2.69569375163578,-14.9004267538186,1.08333333333333));
#38724=CARTESIAN_POINT('',(2.35859284151893,-14.0534529496468,1.08333333333333));
#38725=CARTESIAN_POINT('Ctrl Pts',(2.6956937516358,-14.9004267538186,1.08333333333332));
#38726=CARTESIAN_POINT('Ctrl Pts',(2.62284674626782,-14.8066618988742,1.08333333333332));
#38727=CARTESIAN_POINT('Ctrl Pts',(2.56054033827465,-14.7041615792632,1.08333333333332));
#38728=CARTESIAN_POINT('Ctrl Pts',(2.4350390150467,-14.4435553962822,1.08333333333332));
#38729=CARTESIAN_POINT('Ctrl Pts',(2.37688304383419,-14.2404175142851,1.08333333333332));
#38730=CARTESIAN_POINT('Ctrl Pts',(2.35859284151955,-14.0534529496467,1.08333333333332));
#38731=CARTESIAN_POINT('',(2.69569375163578,-14.9004267538186,-1.08333333333334));
#38732=CARTESIAN_POINT('Ctrl Pts',(2.69569375163578,-14.9004267538186,1.08333333333333));
#38733=CARTESIAN_POINT('Ctrl Pts',(2.65885518901859,-14.9070913604575,0.956888632103347));
#38734=CARTESIAN_POINT('Ctrl Pts',(2.62852794948137,-14.9124412415715,0.828820583351256));
#38735=CARTESIAN_POINT('Ctrl Pts',(2.60478912083403,-14.9165866029902,0.699646919261879));
#38736=CARTESIAN_POINT('Ctrl Pts',(2.58117511159368,-14.9207101679857,0.571152453813268));
#38737=CARTESIAN_POINT('Ctrl Pts',(2.56408033836306,-14.9236419130061,0.441563969171648));
#38738=CARTESIAN_POINT('Ctrl Pts',(2.55357092618676,-14.9254399524253,0.311391073637824));
#38739=CARTESIAN_POINT('Ctrl Pts',(2.54314585302948,-14.9272235624095,0.182262827807427));
#38740=CARTESIAN_POINT('Ctrl Pts',(2.53920083715778,-14.927891621514,0.0525595133520343));
#38741=CARTESIAN_POINT('Ctrl Pts',(2.54179158298272,-14.9274504788058,-0.077221432194672));
#38742=CARTESIAN_POINT('Ctrl Pts',(2.54355857371286,-14.9271496020974,-0.165737150534507));
#38743=CARTESIAN_POINT('Ctrl Pts',(2.54836567846244,-14.9263317077699,-0.254288981130285));
#38744=CARTESIAN_POINT('Ctrl Pts',(2.55622822284789,-14.9249850760809,-0.342719102199546));
#38745=CARTESIAN_POINT('Ctrl Pts',(2.56808166802554,-14.9229549158531,-0.47603492730158));
#38746=CARTESIAN_POINT('Ctrl Pts',(2.58681028013297,-14.9197373081624,-0.608312350205393));
#38747=CARTESIAN_POINT('Ctrl Pts',(2.61224028910069,-14.9152835347009,-0.739057191237091));
#38748=CARTESIAN_POINT('Ctrl Pts',(2.63481838123332,-14.9113292416576,-0.855139299993913));
#38749=CARTESIAN_POINT('Ctrl Pts',(2.66267894744191,-14.9063995895532,-0.970013302477622));
#38750=CARTESIAN_POINT('Ctrl Pts',(2.69569375163578,-14.9004267538186,-1.08333333333334));
#38751=CARTESIAN_POINT('',(2.35859284152043,-14.0534529496557,-1.08333333333334));
#38752=CARTESIAN_POINT('Ctrl Pts',(2.6956937516358,-14.9004267538186,-1.08333333333334));
#38753=CARTESIAN_POINT('Ctrl Pts',(2.62284674626782,-14.8066618988742,-1.08333333333334));
#38754=CARTESIAN_POINT('Ctrl Pts',(2.56054033827465,-14.7041615792632,-1.08333333333334));
#38755=CARTESIAN_POINT('Ctrl Pts',(2.43503901504795,-14.4435553962848,-1.08333333333334));
#38756=CARTESIAN_POINT('Ctrl Pts',(2.37688304383586,-14.2404175142916,-1.08333333333334));
#38757=CARTESIAN_POINT('Ctrl Pts',(2.35859284152042,-14.0534529496557,-1.08333333333334));
#38758=CARTESIAN_POINT('Ctrl Pts',(2.35859284151951,-14.0534529496467,-1.08333333333319));
#38759=CARTESIAN_POINT('Ctrl Pts',(2.32465906345733,-14.0591480600448,-0.949270311030372));
#38760=CARTESIAN_POINT('Ctrl Pts',(2.29705730368849,-14.0636584116899,-0.813521288367913));
#38761=CARTESIAN_POINT('Ctrl Pts',(2.27588092254449,-14.0670844892038,-0.676607052100994));
#38762=CARTESIAN_POINT('Ctrl Pts',(2.25777746665768,-14.0700134052785,-0.55956057377781));
#38763=CARTESIAN_POINT('Ctrl Pts',(2.24436971878542,-14.0721491406499,-0.441662516279038));
#38764=CARTESIAN_POINT('Ctrl Pts',(2.23571067141573,-14.073524711092,-0.323238258334718));
#38765=CARTESIAN_POINT('Ctrl Pts',(2.2257050924945,-14.0751141906309,-0.186398348762649));
#38766=CARTESIAN_POINT('Ctrl Pts',(2.22206972520347,-14.0756851929985,-0.0492519096262131));
#38767=CARTESIAN_POINT('Ctrl Pts',(2.22477765061414,-14.0752571701311,0.087675827066048));
#38768=CARTESIAN_POINT('Ctrl Pts',(2.22749342636756,-14.0748279064149,0.225000520654297));
#38769=CARTESIAN_POINT('Ctrl Pts',(2.23658933237962,-14.0733937867901,0.362105241912729));
#38770=CARTESIAN_POINT('Ctrl Pts',(2.25202995120888,-14.0709225390114,0.498460177595558));
#38771=CARTESIAN_POINT('Ctrl Pts',(2.26753718309241,-14.0684406299137,0.635403368116538));
#38772=CARTESIAN_POINT('Ctrl Pts',(2.28944404469282,-14.0649125984157,0.771590289741026));
#38773=CARTESIAN_POINT('Ctrl Pts',(2.31770587921582,-14.0602538902201,0.906484242526269));
#38774=CARTESIAN_POINT('Ctrl Pts',(2.33011188776182,-14.0582088717468,0.965698216399587));
#38775=CARTESIAN_POINT('Ctrl Pts',(2.34374232952329,-14.0559453130119,1.02466304565376));
#38776=CARTESIAN_POINT('Ctrl Pts',(2.35859284151951,-14.0534529496467,1.08333333333318));
#38777=CARTESIAN_POINT('Origin',(6.1828432824253,-12.8388063676094,-4.9761330016223E-15));
#38778=CARTESIAN_POINT('',(9.43214127690845,-11.8458513067217,-1.08333333333334));
#38779=CARTESIAN_POINT('',(9.24400314381522,-11.3646294742516,-1.08333333333334));
#38780=CARTESIAN_POINT('Origin',(6.1828432824253,-12.8388063676094,-1.08333333333334));
#38781=CARTESIAN_POINT('',(3.12168342103538,-14.3129832609672,-1.08333333333334));
#38782=CARTESIAN_POINT('Origin',(6.1828432824253,-12.8388063676094,-4.9761330016223E-15));
#38783=CARTESIAN_POINT('',(3.38061559238708,-14.7601124814491,-1.08333333333334));
#38784=CARTESIAN_POINT('Origin',(6.1828432824253,-12.8388063676094,-1.08333333333334));
#38785=CARTESIAN_POINT('',(3.38061559238708,-14.7601124814491,1.08333333333333));
#38786=CARTESIAN_POINT('Ctrl Pts',(3.3806155923871,-14.7601124814491,-1.08333333333334));
#38787=CARTESIAN_POINT('Ctrl Pts',(3.26177754255705,-14.7873308217381,-0.7276662218228));
#38788=CARTESIAN_POINT('Ctrl Pts',(3.20402082808022,-14.7994504216119,-0.35278297384278));
#38789=CARTESIAN_POINT('Ctrl Pts',(3.20402082808022,-14.7994504216119,-5.42337291349619E-15));
#38790=CARTESIAN_POINT('Ctrl Pts',(3.20402082808022,-14.7994504216119,0.352782973842771));
#38791=CARTESIAN_POINT('Ctrl Pts',(3.26177754255705,-14.7873308217381,0.727666221822789));
#38792=CARTESIAN_POINT('Ctrl Pts',(3.3806155923871,-14.7601124814491,1.08333333333333));
#38793=CARTESIAN_POINT('',(2.96777005866014,-13.9375335292483,1.08333333333333));
#38794=CARTESIAN_POINT('Origin',(6.1828432824253,-12.8388063676094,1.08333333333333));
#38795=CARTESIAN_POINT('',(2.96777005866014,-13.9375335292483,-1.08333333333334));
#38796=CARTESIAN_POINT('Ctrl Pts',(2.96777005866014,-13.9375335292483,1.08333333333333));
#38797=CARTESIAN_POINT('Ctrl Pts',(2.85550994597651,-13.9614374861791,0.725928647976575));
#38798=CARTESIAN_POINT('Ctrl Pts',(2.80148393014454,-13.9719070920595,0.352039859176984));
#38799=CARTESIAN_POINT('Ctrl Pts',(2.80148393014454,-13.9719070920595,-5.10230940761107E-15));
#38800=CARTESIAN_POINT('Ctrl Pts',(2.80148393014454,-13.9719070920595,-0.352039859176994));
#38801=CARTESIAN_POINT('Ctrl Pts',(2.85550994597651,-13.9614374861791,-0.725928647976584));
#38802=CARTESIAN_POINT('Ctrl Pts',(2.96777005866014,-13.9375335292483,-1.08333333333334));
#38803=CARTESIAN_POINT('Origin',(6.1828432824253,-12.8388063676094,-1.08333333333334));
#38804=CARTESIAN_POINT('',(9.04642813528394,-11.0102060831368,-1.08333333333334));
#38805=CARTESIAN_POINT('Origin',(6.1828432824253,-12.8388063676094,-1.08333333333334));
#38806=CARTESIAN_POINT('',(9.04642813528394,-11.0102060831368,1.08333333333333));
#38807=CARTESIAN_POINT('Ctrl Pts',(9.04642813528395,-11.0102060831368,-1.08333333333334));
#38808=CARTESIAN_POINT('Ctrl Pts',(9.13511003678174,-10.9373414661857,-0.725928647976586));
#38809=CARTESIAN_POINT('Ctrl Pts',(9.17698017417438,-10.9016299186319,-0.352039859176995));
#38810=CARTESIAN_POINT('Ctrl Pts',(9.17698017417438,-10.9016299186319,0.352039859176985));
#38811=CARTESIAN_POINT('Ctrl Pts',(9.13511003678174,-10.9373414661857,0.725928647976577));
#38812=CARTESIAN_POINT('Ctrl Pts',(9.04642813528396,-11.0102060831368,1.08333333333333));
#38813=CARTESIAN_POINT('',(9.43214127690845,-11.8458513067217,1.08333333333333));
#38814=CARTESIAN_POINT('Origin',(6.1828432824253,-12.8388063676094,1.08333333333333));
#38815=CARTESIAN_POINT('Ctrl Pts',(9.43214127690846,-11.8458513067217,1.08333333333333));
#38816=CARTESIAN_POINT('Ctrl Pts',(9.52751574438876,-11.7699103356432,0.727666221822791));
#38817=CARTESIAN_POINT('Ctrl Pts',(9.57300195159016,-11.7323107648652,0.352782973842771));
#38818=CARTESIAN_POINT('Ctrl Pts',(9.57300195159016,-11.7323107648652,-0.352782973842781));
#38819=CARTESIAN_POINT('Ctrl Pts',(9.52751574438875,-11.7699103356432,-0.7276662218228));
#38820=CARTESIAN_POINT('Ctrl Pts',(9.43214127690846,-11.8458513067217,-1.08333333333334));
#38821=CARTESIAN_POINT('',(5.79568548444348,-12.0348649162504,3.45272288248773));
#38822=CARTESIAN_POINT('Origin',(5.79568548444348,-12.0348649162504,-4.66453708897011E-15));
#38823=CARTESIAN_POINT('',(6.57000108040713,-13.6427478189685,3.45272288248772));
#38824=CARTESIAN_POINT('Origin',(6.57000108040713,-13.6427478189685,-5.28772891427449E-15));
#38825=CARTESIAN_POINT('Origin',(13.892722748591,-3.17092330887735,-3.20017169526122E-15));
#38826=CARTESIAN_POINT('',(14.7626584240763,-3.36948044994605,-3.96060240207311));
#38827=CARTESIAN_POINT('Origin',(14.7626584240763,-3.36948044994605,-3.40056031423575E-15));
#38828=CARTESIAN_POINT('',(13.0227870731057,-2.97236616780864,-3.96060240207311));
#38829=CARTESIAN_POINT('Origin',(13.892722748591,-3.17092330887735,-2.5198520116158));
#38830=CARTESIAN_POINT('Origin',(13.0227870731057,-2.97236616780865,-2.9997830762867E-15));
#38831=CARTESIAN_POINT('',(14.2259398250621,0.827729480997053,1.08333333333333));
#38832=CARTESIAN_POINT('',(15.1266902369927,0.68754979644376,1.08333333333333));
#38833=CARTESIAN_POINT('Ctrl Pts',(14.2259398250621,0.827729480997104,1.08333333333333));
#38834=CARTESIAN_POINT('Ctrl Pts',(14.4122867506183,0.85150138178118,1.08333333333333));
#38835=CARTESIAN_POINT('Ctrl Pts',(14.6232724628281,0.840005933409976,1.08333333333333));
#38836=CARTESIAN_POINT('Ctrl Pts',(14.9052713763609,0.775641521611009,1.08333333333333));
#38837=CARTESIAN_POINT('Ctrl Pts',(15.0190662790554,0.737705732201359,1.08333333333333));
#38838=CARTESIAN_POINT('Ctrl Pts',(15.1266902369927,0.687549796443767,1.08333333333333));
#38839=CARTESIAN_POINT('',(14.2259398250621,0.827729480997055,-1.08333333333334));
#38840=CARTESIAN_POINT('Ctrl Pts',(14.2259398250621,0.8277294809971,1.08333333333334));
#38841=CARTESIAN_POINT('Ctrl Pts',(14.2239464151202,0.861989623387911,0.949622058007612));
#38842=CARTESIAN_POINT('Ctrl Pts',(14.2222079250172,0.889808711690379,0.814376693553152));
#38843=CARTESIAN_POINT('Ctrl Pts',(14.2208398148552,0.911161325030034,0.678132403727965));
#38844=CARTESIAN_POINT('Ctrl Pts',(14.2194782068654,0.932412456504566,0.542535637670654));
#38845=CARTESIAN_POINT('Ctrl Pts',(14.2184834780892,0.947258512328438,0.40594941879874));
#38846=CARTESIAN_POINT('Ctrl Pts',(14.2179179597194,0.955671957676133,0.268901316711642));
#38847=CARTESIAN_POINT('Ctrl Pts',(14.2175487034788,0.961165532006069,0.179415511018676));
#38848=CARTESIAN_POINT('Ctrl Pts',(14.2173613909827,0.963916530720146,0.0897327832366183));
#38849=CARTESIAN_POINT('Ctrl Pts',(14.2173613909827,0.963916530720146,1.06581410364015E-14));
#38850=CARTESIAN_POINT('Ctrl Pts',(14.2173613909827,0.963916530720146,-0.13757393698032));
#38851=CARTESIAN_POINT('Ctrl Pts',(14.2178040883167,0.957451598945758,-0.274951212619625));
#38852=CARTESIAN_POINT('Ctrl Pts',(14.2186598102071,0.944570379379524,-0.411612406214599));
#38853=CARTESIAN_POINT('Ctrl Pts',(14.2195221530139,0.931589494866494,-0.549330978772693));
#38854=CARTESIAN_POINT('Ctrl Pts',(14.2208039138492,0.912092599491427,-0.686322345436757));
#38855=CARTESIAN_POINT('Ctrl Pts',(14.222421741201,0.886126297665472,-0.822054935347047));
#38856=CARTESIAN_POINT('Ctrl Pts',(14.2234666476786,0.869355437073955,-0.909720570537178));
#38857=CARTESIAN_POINT('Ctrl Pts',(14.2246506698206,0.849885807807131,-0.996861109122824));
#38858=CARTESIAN_POINT('Ctrl Pts',(14.2259398250621,0.827729480997101,-1.08333333333335));
#38859=CARTESIAN_POINT('',(15.1266902369927,0.687549796443762,-1.08333333333334));
#38860=CARTESIAN_POINT('Ctrl Pts',(14.2259398250621,0.827729480997104,-1.08333333333333));
#38861=CARTESIAN_POINT('Ctrl Pts',(14.4122867506183,0.85150138178118,-1.08333333333333));
#38862=CARTESIAN_POINT('Ctrl Pts',(14.6232724628281,0.840005933409977,-1.08333333333333));
#38863=CARTESIAN_POINT('Ctrl Pts',(14.9052713763609,0.775641521611009,-1.08333333333333));
#38864=CARTESIAN_POINT('Ctrl Pts',(15.0190662790554,0.73770573220136,-1.08333333333333));
#38865=CARTESIAN_POINT('Ctrl Pts',(15.1266902369927,0.687549796443768,-1.08333333333333));
#38866=CARTESIAN_POINT('Ctrl Pts',(15.1266902369927,0.687549796443768,-1.08333333333334));
#38867=CARTESIAN_POINT('Ctrl Pts',(15.1249773086751,0.725235701077452,-0.955915065626868));
#38868=CARTESIAN_POINT('Ctrl Pts',(15.1234319803901,0.756223536825589,-0.826701571451108));
#38869=CARTESIAN_POINT('Ctrl Pts',(15.122183667988,0.780412301388443,-0.696211209493001));
#38870=CARTESIAN_POINT('Ctrl Pts',(15.1209550316477,0.804219799510377,-0.567777653526322));
#38871=CARTESIAN_POINT('Ctrl Pts',(15.12001416535,0.821440959530357,-0.43810716485706));
#38872=CARTESIAN_POINT('Ctrl Pts',(15.1194343523859,0.831977831684773,-0.307693975182356));
#38873=CARTESIAN_POINT('Ctrl Pts',(15.1189800281283,0.840234212474528,-0.205506064179778));
#38874=CARTESIAN_POINT('Ctrl Pts',(15.1187464308798,0.844386527178536,-0.102862147741283));
#38875=CARTESIAN_POINT('Ctrl Pts',(15.1187464308798,0.844386527178536,-1.99840144432528E-15));
#38876=CARTESIAN_POINT('Ctrl Pts',(15.1187464308798,0.844386527178536,0.130666807305585));
#38877=CARTESIAN_POINT('Ctrl Pts',(15.1191251529677,0.837684329050871,0.261069786498764));
#38878=CARTESIAN_POINT('Ctrl Pts',(15.1198518432089,0.824355801783881,0.390710450871172));
#38879=CARTESIAN_POINT('Ctrl Pts',(15.1205872590302,0.810867235029882,0.521907748246314));
#38880=CARTESIAN_POINT('Ctrl Pts',(15.1216790167187,0.790592205023559,0.652324314224285));
#38881=CARTESIAN_POINT('Ctrl Pts',(15.1230415909943,0.763606761086929,0.781443489202972));
#38882=CARTESIAN_POINT('Ctrl Pts',(15.1241128691977,0.742390363262186,0.882959098491574));
#38883=CARTESIAN_POINT('Ctrl Pts',(15.1253504648421,0.717025942630064,0.983672743459537));
#38884=CARTESIAN_POINT('Ctrl Pts',(15.1266902369927,0.687549796443768,1.08333333333333));
#38885=CARTESIAN_POINT('',(13.3303603014235,-7.18268588222768,1.08333333333333));
#38886=CARTESIAN_POINT('',(12.4579905368411,-6.91816245718305,1.08333333333333));
#38887=CARTESIAN_POINT('Ctrl Pts',(13.3303603014235,-7.18268588222769,1.08333333333333));
#38888=CARTESIAN_POINT('Ctrl Pts',(13.2116326209361,-7.18117853359731,1.08333333333333));
#38889=CARTESIAN_POINT('Ctrl Pts',(13.0926472341269,-7.16598374096113,1.08333333333333));
#38890=CARTESIAN_POINT('Ctrl Pts',(12.8106483205942,-7.10161932916216,1.08333333333333));
#38891=CARTESIAN_POINT('Ctrl Pts',(12.6155690741987,-7.02043310055321,1.08333333333333));
#38892=CARTESIAN_POINT('Ctrl Pts',(12.4579905368414,-6.91816245718254,1.08333333333333));
#38893=CARTESIAN_POINT('',(13.3303603014235,-7.18268588222768,-1.08333333333334));
#38894=CARTESIAN_POINT('Ctrl Pts',(13.3303603014235,-7.18268588222769,1.08333333333333));
#38895=CARTESIAN_POINT('Ctrl Pts',(13.3126024326051,-7.21564274452345,0.956888632103319));
#38896=CARTESIAN_POINT('Ctrl Pts',(13.2978764135175,-7.24268913148574,0.828820583351199));
#38897=CARTESIAN_POINT('Ctrl Pts',(13.2863164700112,-7.26383348564869,0.699646919261793));
#38898=CARTESIAN_POINT('Ctrl Pts',(13.2748173090023,-7.28486666222208,0.57115245381317));
#38899=CARTESIAN_POINT('Ctrl Pts',(13.2664510227834,-7.30005980724128,0.441563969171537));
#38900=CARTESIAN_POINT('Ctrl Pts',(13.2613042752927,-7.30939745578421,0.311391073637702));
#38901=CARTESIAN_POINT('Ctrl Pts',(13.2561988309336,-7.31866016882124,0.182262827807302));
#38902=CARTESIAN_POINT('Ctrl Pts',(13.2542614634095,-7.32216103446727,0.0525595133519065));
#38903=CARTESIAN_POINT('Ctrl Pts',(13.2555318677529,-7.3198604598385,-0.0772214321948015));
#38904=CARTESIAN_POINT('Ctrl Pts',(13.2563983335702,-7.31829137729713,-0.16573715053459));
#38905=CARTESIAN_POINT('Ctrl Pts',(13.2587560588235,-7.31402308269219,-0.254288981130321));
#38906=CARTESIAN_POINT('Ctrl Pts',(13.2626054360147,-7.30703628683439,-0.342719102199534));
#38907=CARTESIAN_POINT('Ctrl Pts',(13.2684086950193,-7.29650310602066,-0.476034927301568));
#38908=CARTESIAN_POINT('Ctrl Pts',(13.2775701666805,-7.2798543418706,-0.608312350205377));
#38909=CARTESIAN_POINT('Ctrl Pts',(13.289943417625,-7.25719547792716,-0.739057191237071));
#38910=CARTESIAN_POINT('Ctrl Pts',(13.300929037023,-7.23707775329776,-0.8551392999939));
#38911=CARTESIAN_POINT('Ctrl Pts',(13.3144456587152,-7.21222189770271,-0.970013302477615));
#38912=CARTESIAN_POINT('Ctrl Pts',(13.3303603014235,-7.18268588222769,-1.08333333333334));
#38913=CARTESIAN_POINT('',(12.4579905368491,-6.91816245718746,-1.08333333333334));
#38914=CARTESIAN_POINT('Ctrl Pts',(13.3303603014235,-7.18268588222769,-1.08333333333333));
#38915=CARTESIAN_POINT('Ctrl Pts',(13.2116326209361,-7.18117853359731,-1.08333333333333));
#38916=CARTESIAN_POINT('Ctrl Pts',(13.0926472341269,-7.16598374096113,-1.08333333333333));
#38917=CARTESIAN_POINT('Ctrl Pts',(12.810648320597,-7.10161932916281,-1.08333333333333));
#38918=CARTESIAN_POINT('Ctrl Pts',(12.6155690742049,-7.020433100556,-1.08333333333333));
#38919=CARTESIAN_POINT('Ctrl Pts',(12.4579905368491,-6.91816245718749,-1.08333333333333));
#38920=CARTESIAN_POINT('Ctrl Pts',(12.4579905368414,-6.91816245718254,-1.08333333333318));
#38921=CARTESIAN_POINT('Ctrl Pts',(12.4412857888865,-6.94824379644432,-0.949270311030419));
#38922=CARTESIAN_POINT('Ctrl Pts',(12.4276027080704,-6.97263587945666,-0.813521288368017));
#38923=CARTESIAN_POINT('Ctrl Pts',(12.4170780656486,-6.99132836531005,-0.676607052101155));
#38924=CARTESIAN_POINT('Ctrl Pts',(12.4080806643215,-7.00730836636693,-0.559560573777918));
#38925=CARTESIAN_POINT('Ctrl Pts',(12.4013908554088,-7.019122574986,-0.441662516279092));
#38926=CARTESIAN_POINT('Ctrl Pts',(12.397067491958,-7.0267501449702,-0.323238258334718));
#38927=CARTESIAN_POINT('Ctrl Pts',(12.3920718206831,-7.03556384585387,-0.186398348762654));
#38928=CARTESIAN_POINT('Ctrl Pts',(12.3902516338787,-7.03876210460539,-0.0492519096262223));
#38929=CARTESIAN_POINT('Ctrl Pts',(12.3916053560035,-7.03637809537437,0.0876758270660355));
#38930=CARTESIAN_POINT('Ctrl Pts',(12.3929630026023,-7.03398717484161,0.225000520654302));
#38931=CARTESIAN_POINT('Ctrl Pts',(12.3975129673672,-7.02598155019911,0.362105241912753));
#38932=CARTESIAN_POINT('Ctrl Pts',(12.4052079364272,-7.01236879050172,0.498460177595601));
#38933=CARTESIAN_POINT('Ctrl Pts',(12.4129361026925,-6.99869730339771,0.635403368116608));
#38934=CARTESIAN_POINT('Ctrl Pts',(12.4238364813948,-6.9793701376568,0.771590289741124));
#38935=CARTESIAN_POINT('Ctrl Pts',(12.4378151222668,-6.95436948862457,0.906484242526394));
#38936=CARTESIAN_POINT('Ctrl Pts',(12.4439512822523,-6.94339503240884,0.96569821639967));
#38937=CARTESIAN_POINT('Ctrl Pts',(12.4506800022041,-6.93132701813272,1.0246630456538));
#38938=CARTESIAN_POINT('Ctrl Pts',(12.4579905368414,-6.91816245718254,1.08333333333318));
#38939=CARTESIAN_POINT('Origin',(13.892722748591,-3.17092330887735,-3.20017169526122E-15));
#38940=CARTESIAN_POINT('',(15.1423033840733,-0.0114224867026808,-1.08333333333334));
#38941=CARTESIAN_POINT('',(14.6487667980729,0.141522102769127,-1.08333333333334));
#38942=CARTESIAN_POINT('Origin',(13.892722748591,-3.17092330887735,-1.08333333333334));
#38943=CARTESIAN_POINT('',(13.1366786991091,-6.48336872052383,-1.08333333333334));
#38944=CARTESIAN_POINT('Origin',(13.892722748591,-3.17092330887735,-3.20017169526122E-15));
#38945=CARTESIAN_POINT('',(13.6476999686242,-6.55970790622078,-1.08333333333334));
#38946=CARTESIAN_POINT('Origin',(13.892722748591,-3.17092330887735,-1.08333333333334));
#38947=CARTESIAN_POINT('',(13.6476999686242,-6.55970790622078,1.08333333333333));
#38948=CARTESIAN_POINT('Ctrl Pts',(13.6476999686242,-6.55970790622078,-1.08333333333334));
#38949=CARTESIAN_POINT('Ctrl Pts',(13.5948858118209,-6.66958959248674,-0.727666221822799));
#38950=CARTESIAN_POINT('Ctrl Pts',(13.5683505740919,-6.72230205711255,-0.35278297384278));
#38951=CARTESIAN_POINT('Ctrl Pts',(13.5683505740919,-6.72230205711255,-3.93962482987281E-15));
#38952=CARTESIAN_POINT('Ctrl Pts',(13.5683505740919,-6.72230205711255,0.352782973842772));
#38953=CARTESIAN_POINT('Ctrl Pts',(13.5948858118209,-6.66958959248674,0.727666221822791));
#38954=CARTESIAN_POINT('Ctrl Pts',(13.6476999686242,-6.55970790622078,1.08333333333333));
#38955=CARTESIAN_POINT('',(12.7471768669564,-6.36961395396396,1.08333333333333));
#38956=CARTESIAN_POINT('Origin',(13.892722748591,-3.17092330887735,1.08333333333333));
#38957=CARTESIAN_POINT('',(12.7471768669564,-6.36961395396396,-1.08333333333334));
#38958=CARTESIAN_POINT('Ctrl Pts',(12.7471768669564,-6.36961395396397,1.08333333333334));
#38959=CARTESIAN_POINT('Ctrl Pts',(12.6958726976266,-6.47228631765585,0.725928647976583));
#38960=CARTESIAN_POINT('Ctrl Pts',(12.6703734952067,-6.52105325020152,0.352039859176988));
#38961=CARTESIAN_POINT('Ctrl Pts',(12.6703734952067,-6.52105325020152,-3.73360976135914E-15));
#38962=CARTESIAN_POINT('Ctrl Pts',(12.6703734952067,-6.52105325020152,-0.352039859176996));
#38963=CARTESIAN_POINT('Ctrl Pts',(12.6958726976266,-6.47228631765585,-0.72592864797659));
#38964=CARTESIAN_POINT('Ctrl Pts',(12.7471768669564,-6.36961395396397,-1.08333333333335));
#38965=CARTESIAN_POINT('Origin',(13.892722748591,-3.17092330887735,-1.08333333333334));
#38966=CARTESIAN_POINT('',(14.2484814298548,0.208031110850763,-1.08333333333334));
#38967=CARTESIAN_POINT('Origin',(13.892722748591,-3.17092330887735,-1.08333333333334));
#38968=CARTESIAN_POINT('',(14.2484814298548,0.208031110850763,1.08333333333333));
#38969=CARTESIAN_POINT('Ctrl Pts',(14.2484814298548,0.208031110850765,-1.08333333333334));
#38970=CARTESIAN_POINT('Ctrl Pts',(14.2468058395578,0.322795758952199,-0.725928647976584));
#38971=CARTESIAN_POINT('Ctrl Pts',(14.2449910310593,0.377796936249431,-0.352039859176992));
#38972=CARTESIAN_POINT('Ctrl Pts',(14.2449910310593,0.37779693624943,0.352039859176986));
#38973=CARTESIAN_POINT('Ctrl Pts',(14.2468058395578,0.322795758952199,0.725928647976576));
#38974=CARTESIAN_POINT('Ctrl Pts',(14.2484814298548,0.208031110850766,1.08333333333333));
#38975=CARTESIAN_POINT('',(15.1423033840733,-0.0114224867026808,1.08333333333333));
#38976=CARTESIAN_POINT('Origin',(13.892722748591,-3.17092330887735,1.08333333333333));
#38977=CARTESIAN_POINT('Ctrl Pts',(15.1423033840733,-0.0114224867026912,
1.08333333333333));
#38978=CARTESIAN_POINT('Ctrl Pts',(15.1423953499066,0.110492695607724,0.727666221822789));
#38979=CARTESIAN_POINT('Ctrl Pts',(15.1413590080604,0.169498193350193,0.352782973842772));
#38980=CARTESIAN_POINT('Ctrl Pts',(15.1413590080604,0.169498193350193,-0.352782973842778));
#38981=CARTESIAN_POINT('Ctrl Pts',(15.1423953499066,0.110492695607724,-0.727666221822797));
#38982=CARTESIAN_POINT('Ctrl Pts',(15.1423033840733,-0.0114224867026924,
-1.08333333333334));
#38983=CARTESIAN_POINT('',(13.0227870731057,-2.97236616780865,3.45272288248773));
#38984=CARTESIAN_POINT('Origin',(13.0227870731057,-2.97236616780865,-2.9997830762867E-15));
#38985=CARTESIAN_POINT('',(14.7626584240763,-3.36948044994605,3.45272288248773));
#38986=CARTESIAN_POINT('Origin',(14.7626584240763,-3.36948044994605,-3.40056031423575E-15));
#38987=CARTESIAN_POINT('Origin',(11.1410986251693,8.88472967648709,-9.85584169237555E-16));
#38988=CARTESIAN_POINT('',(11.8387328710639,9.44107442276104,-3.96060240207311));
#38989=CARTESIAN_POINT('Origin',(11.8387328710639,9.44107442276104,-1.0472995612114E-15));
#38990=CARTESIAN_POINT('',(10.4434643792748,8.32838493021314,-3.96060240207311));
#38991=CARTESIAN_POINT('Origin',(11.1410986251693,8.88472967648709,-2.5198520116158));
#38992=CARTESIAN_POINT('Origin',(10.4434643792748,8.32838493021314,-9.23868777263706E-16));
#38993=CARTESIAN_POINT('',(8.89378902201275,12.2552029391784,1.08333333331655));
#38994=CARTESIAN_POINT('',(8.89378902201677,12.2552029391754,-1.08333333333333));
#38995=CARTESIAN_POINT('Ctrl Pts',(8.89378902201274,12.2552029391784,1.08333333331655));
#38996=CARTESIAN_POINT('Ctrl Pts',(8.86335293025879,12.2772908784853,0.956315399884826));
#38997=CARTESIAN_POINT('Ctrl Pts',(8.83824313040494,12.2953456493747,0.827586922367285));
#38998=CARTESIAN_POINT('Ctrl Pts',(8.81859777764014,12.3094197866805,0.69766772380084));
#38999=CARTESIAN_POINT('Ctrl Pts',(8.7991879276401,12.3233252073292,0.569305958731489));
#39000=CARTESIAN_POINT('Ctrl Pts',(8.78511225071473,12.3333449381983,0.439781849534452));
#39001=CARTESIAN_POINT('Ctrl Pts',(8.77647376760361,12.3394890678296,0.309596747993595));
#39002=CARTESIAN_POINT('Ctrl Pts',(8.76964787761092,12.344343988818,0.206728088024587));
#39003=CARTESIAN_POINT('Ctrl Pts',(8.76621624622163,12.3467783236357,0.103446722778746));
#39004=CARTESIAN_POINT('Ctrl Pts',(8.76621624622163,12.3467783236357,7.54951656745106E-15));
#39005=CARTESIAN_POINT('Ctrl Pts',(8.76621624622163,12.3467783236357,-0.130951008152141));
#39006=CARTESIAN_POINT('Ctrl Pts',(8.77171477448527,12.3428797767713,-0.261548325668487));
#39007=CARTESIAN_POINT('Ctrl Pts',(8.78261416841303,12.3351194002049,-0.391301356121213));
#39008=CARTESIAN_POINT('Ctrl Pts',(8.79368558213778,12.3272365454154,-0.523102215114213));
#39009=CARTESIAN_POINT('Ctrl Pts',(8.81032969837903,12.3153689336875,-0.654031926803563));
#39010=CARTESIAN_POINT('Ctrl Pts',(8.83241243050519,12.2995110840219,-0.783576297698762));
#39011=CARTESIAN_POINT('Ctrl Pts',(8.84960195907419,12.2871670969504,-0.88441557119687));
#39012=CARTESIAN_POINT('Ctrl Pts',(8.87008627043973,12.2724043900869,-0.984415425401903));
#39013=CARTESIAN_POINT('Ctrl Pts',(8.89378902201675,12.2552029391755,-1.08333333333333));
#39014=CARTESIAN_POINT('',(8.22258343557175,11.6383685130288,1.08333333333333));
#39015=CARTESIAN_POINT('Ctrl Pts',(8.89378902201473,12.2552029391744,1.08333333333333));
#39016=CARTESIAN_POINT('Ctrl Pts',(8.7875190745609,12.202353722575,1.08333333333333));
#39017=CARTESIAN_POINT('Ctrl Pts',(8.68681488082435,12.1369760343753,1.08333333333333));
#39018=CARTESIAN_POINT('Ctrl Pts',(8.46069343470619,11.9566501984405,1.08333333333333));
#39019=CARTESIAN_POINT('Ctrl Pts',(8.31988542322913,11.7983921800676,1.08333333333333));
#39020=CARTESIAN_POINT('Ctrl Pts',(8.22258343557172,11.6383685130288,1.08333333333333));
#39021=CARTESIAN_POINT('',(8.22258343557123,11.6383685130292,-1.08333333333333));
#39022=CARTESIAN_POINT('Ctrl Pts',(8.2225834355717,11.6383685130289,-1.08333333333318));
#39023=CARTESIAN_POINT('Ctrl Pts',(8.19448780675769,11.6582182584498,-0.949301954017324));
#39024=CARTESIAN_POINT('Ctrl Pts',(8.17159767874311,11.6742430454627,-0.81366496302888));
#39025=CARTESIAN_POINT('Ctrl Pts',(8.15402161030241,11.6865063889394,-0.67695567866062));
#39026=CARTESIAN_POINT('Ctrl Pts',(8.13658119548769,11.6986750828637,-0.541301528447691));
#39027=CARTESIAN_POINT('Ctrl Pts',(8.12437307855494,11.7071402381473,-0.40459157308691));
#39028=CARTESIAN_POINT('Ctrl Pts',(8.1174733585697,11.7119223986889,-0.26734687734235));
#39029=CARTESIAN_POINT('Ctrl Pts',(8.11300215046573,11.7150213700985,-0.178408544025479));
#39030=CARTESIAN_POINT('Ctrl Pts',(8.11075954642938,11.7165728598428,-0.0892456520429063));
#39031=CARTESIAN_POINT('Ctrl Pts',(8.11075954642938,11.7165728598428,1.33226762955019E-15));
#39032=CARTESIAN_POINT('Ctrl Pts',(8.11075954642938,11.7165728598428,0.137335411050026));
#39033=CARTESIAN_POINT('Ctrl Pts',(8.11607262981309,11.7129002012938,0.274553571737022));
#39034=CARTESIAN_POINT('Ctrl Pts',(8.12665801674411,11.7055512249056,0.411127959090392));
#39035=CARTESIAN_POINT('Ctrl Pts',(8.13729388250879,11.698167203246,0.548353632582512));
#39036=CARTESIAN_POINT('Ctrl Pts',(8.15325248641432,11.6870716767896,0.684929378140945));
#39037=CARTESIAN_POINT('Ctrl Pts',(8.17446212457132,11.6722178258439,0.820321104282498));
#39038=CARTESIAN_POINT('Ctrl Pts',(8.18828255682692,11.6625388940673,0.908543834215877));
#39039=CARTESIAN_POINT('Ctrl Pts',(8.20433194575505,11.6512633098961,0.9962638332735));
#39040=CARTESIAN_POINT('Ctrl Pts',(8.22258343557176,11.6383685130288,1.08333333333334));
#39041=CARTESIAN_POINT('Ctrl Pts',(8.89378902201675,12.2552029391755,-1.08333333333333));
#39042=CARTESIAN_POINT('Ctrl Pts',(8.78751907456219,12.2023537225759,-1.08333333333333));
#39043=CARTESIAN_POINT('Ctrl Pts',(8.68681488082489,12.1369760343758,-1.08333333333333));
#39044=CARTESIAN_POINT('Ctrl Pts',(8.46069343470621,11.9566501984405,-1.08333333333333));
#39045=CARTESIAN_POINT('Ctrl Pts',(8.31988542322917,11.7983921800676,-1.08333333333333));
#39046=CARTESIAN_POINT('Ctrl Pts',(8.22258343557176,11.6383685130289,-1.08333333333333));
#39047=CARTESIAN_POINT('',(13.9269936544443,5.94376395877129,1.08333333333333));
#39048=CARTESIAN_POINT('',(13.1762672612271,5.42664547033562,1.08333333333333));
#39049=CARTESIAN_POINT('Ctrl Pts',(13.9269936544443,5.94376395877129,1.08333333333333));
#39050=CARTESIAN_POINT('Ctrl Pts',(13.8517896638478,5.85187873682469,1.08333333333333));
#39051=CARTESIAN_POINT('Ctrl Pts',(13.7657237213495,5.76832601371371,1.08333333333333));
#39052=CARTESIAN_POINT('Ctrl Pts',(13.5395781511316,5.5879809394513,1.08333333333333));
#39053=CARTESIAN_POINT('Ctrl Pts',(13.3544742809805,5.48608062863226,1.08333333333333));
#39054=CARTESIAN_POINT('Ctrl Pts',(13.1762672612269,5.42664547033621,1.08333333333333));
#39055=CARTESIAN_POINT('',(13.9269936544443,5.94376395877129,-1.08333333333333));
#39056=CARTESIAN_POINT('Ctrl Pts',(13.9269936544443,5.9437639587713,1.08333333333333));
#39057=CARTESIAN_POINT('Ctrl Pts',(13.9416885168395,5.90933203032488,0.95688863210334));
#39058=CARTESIAN_POINT('Ctrl Pts',(13.9536527109305,5.88095561854266,0.828820583351241));
#39059=CARTESIAN_POINT('Ctrl Pts',(13.9629765258053,5.85873440158633,0.699646919261855));
#39060=CARTESIAN_POINT('Ctrl Pts',(13.9722513158077,5.83663002439342,0.571152453813261));
#39061=CARTESIAN_POINT('Ctrl Pts',(13.9789135007645,5.82061622745854,0.441563969171658));
#39062=CARTESIAN_POINT('Ctrl Pts',(13.9830050237944,5.81077040959811,0.31139107363785));
#39063=CARTESIAN_POINT('Ctrl Pts',(13.987063711968,5.80100360535004,0.182262827807452));
#39064=CARTESIAN_POINT('Ctrl Pts',(13.9885928700522,5.79730615639857,0.0525595133520559));
#39065=CARTESIAN_POINT('Ctrl Pts',(13.9875862925321,5.79973378332923,-0.077221432194654));
#39066=CARTESIAN_POINT('Ctrl Pts',(13.9868997670033,5.80138952054645,-0.165737150534494));
#39067=CARTESIAN_POINT('Ctrl Pts',(13.9850326975557,5.80589410253397,-0.254288981130278));
#39068=CARTESIAN_POINT('Ctrl Pts',(13.9819702480148,5.81325986277498,-0.342719102199545));
#39069=CARTESIAN_POINT('Ctrl Pts',(13.977353348451,5.82436436418423,-0.476034927301432));
#39070=CARTESIAN_POINT('Ctrl Pts',(13.9700489046451,5.84190742581571,-0.608312350205104));
#39071=CARTESIAN_POINT('Ctrl Pts',(13.9600480872369,5.86570879353505,-0.739057191236667));
#39072=CARTESIAN_POINT('Ctrl Pts',(13.9511688384277,5.88684089277784,-0.855139299993628));
#39073=CARTESIAN_POINT('Ctrl Pts',(13.9401632237805,5.91290598563348,-0.970013302477476));
#39074=CARTESIAN_POINT('Ctrl Pts',(13.9269936544443,5.9437639587713,-1.08333333333333));
#39075=CARTESIAN_POINT('',(13.1762672612355,5.42664547033908,-1.08333333333333));
#39076=CARTESIAN_POINT('Ctrl Pts',(13.9269936544443,5.94376395877129,-1.08333333333333));
#39077=CARTESIAN_POINT('Ctrl Pts',(13.8517896638478,5.85187873682469,-1.08333333333333));
#39078=CARTESIAN_POINT('Ctrl Pts',(13.7657237213495,5.76832601371371,-1.08333333333333));
#39079=CARTESIAN_POINT('Ctrl Pts',(13.5395781511339,5.5879809394531,-1.08333333333333));
#39080=CARTESIAN_POINT('Ctrl Pts',(13.3544742809865,5.48608062863536,-1.08333333333333));
#39081=CARTESIAN_POINT('Ctrl Pts',(13.1762672612355,5.42664547033908,-1.08333333333333));
#39082=CARTESIAN_POINT('Ctrl Pts',(13.1762672612269,5.42664547033617,-1.08333333333318));
#39083=CARTESIAN_POINT('Ctrl Pts',(13.1893705593041,5.39482976422236,-0.949270311030452));
#39084=CARTESIAN_POINT('Ctrl Pts',(13.1999097963792,5.36892368585892,-0.813521288368082));
#39085=CARTESIAN_POINT('Ctrl Pts',(13.2079621630868,5.34904061477083,-0.676607052101254));
#39086=CARTESIAN_POINT('Ctrl Pts',(13.2148460430323,5.33204279546023,-0.559560573777983));
#39087=CARTESIAN_POINT('Ctrl Pts',(13.2199117356377,5.31944645364959,-0.441662516279123));
#39088=CARTESIAN_POINT('Ctrl Pts',(13.2231796369647,5.31131059989547,-0.323238258334714));
#39089=CARTESIAN_POINT('Ctrl Pts',(13.2269557156993,5.30190957419912,-0.186398348762647));
#39090=CARTESIAN_POINT('Ctrl Pts',(13.2283213471703,5.2984924131362,-0.0492519096262126));
#39091=CARTESIAN_POINT('Ctrl Pts',(13.2273014856384,5.30103720115497,0.087675827066048));
#39092=CARTESIAN_POINT('Ctrl Pts',(13.2262786675026,5.30358936657715,0.225000520654307));
#39093=CARTESIAN_POINT('Ctrl Pts',(13.22285647475,5.31213809759657,0.362105241912749));
#39094=CARTESIAN_POINT('Ctrl Pts',(13.2170113253899,5.32664168351083,0.498460177595588));
#39095=CARTESIAN_POINT('Ctrl Pts',(13.2111409592133,5.34120783998435,0.635403368116607));
#39096=CARTESIAN_POINT('Ctrl Pts',(13.2028266475275,5.36178038996296,0.771590289741134));
#39097=CARTESIAN_POINT('Ctrl Pts',(13.1919958930594,5.38829698119018,0.906484242526414));
#39098=CARTESIAN_POINT('Ctrl Pts',(13.1872415508606,5.3999368857798,0.965698216399684));
#39099=CARTESIAN_POINT('Ctrl Pts',(13.1820016856381,5.41272189470467,1.02466304565381));
#39100=CARTESIAN_POINT('Ctrl Pts',(13.1762672612269,5.42664547033617,1.08333333333318));
#39101=CARTESIAN_POINT('Origin',(11.1410986251693,8.88472967648709,-9.85584169237555E-16));
#39102=CARTESIAN_POINT('',(8.72113759169208,11.2696166353064,-1.08333333333333));
#39103=CARTESIAN_POINT('',(9.02271027299523,11.54110464988,-1.08333333333333));
#39104=CARTESIAN_POINT('Origin',(11.1410986251693,8.88472967648709,-1.08333333333333));
#39105=CARTESIAN_POINT('',(8.72113759169208,11.2696166353064,1.08333333333333));
#39106=CARTESIAN_POINT('Ctrl Pts',(8.72113759169207,11.2696166353064,1.08333333333334));
#39107=CARTESIAN_POINT('Ctrl Pts',(8.63036626326973,11.3398611937657,0.725928647976583));
#39108=CARTESIAN_POINT('Ctrl Pts',(8.5862330966948,11.3727349924819,0.35203985917699));
#39109=CARTESIAN_POINT('Ctrl Pts',(8.5862330966948,11.3727349924819,-0.352039859176991));
#39110=CARTESIAN_POINT('Ctrl Pts',(8.63036626326973,11.3398611937657,-0.725928647976582));
#39111=CARTESIAN_POINT('Ctrl Pts',(8.72113759169207,11.2696166353064,-1.08333333333334));
#39112=CARTESIAN_POINT('',(9.4500021963329,11.8316076987797,1.08333333333333));
#39113=CARTESIAN_POINT('Origin',(11.1410986251693,8.88472967648709,1.08333333333333));
#39114=CARTESIAN_POINT('',(9.4500021963329,11.8316076987797,-1.08333333333333));
#39115=CARTESIAN_POINT('Ctrl Pts',(9.4500021963329,11.8316076987798,-1.08333333333334));
#39116=CARTESIAN_POINT('Ctrl Pts',(9.35474240837097,11.9076924734258,-0.7276662218228));
#39117=CARTESIAN_POINT('Ctrl Pts',(9.30796390402485,11.9436715548399,-0.352782973842779));
#39118=CARTESIAN_POINT('Ctrl Pts',(9.30796390402485,11.9436715548399,0.352782973842777));
#39119=CARTESIAN_POINT('Ctrl Pts',(9.35474240837097,11.9076924734258,0.727666221822799));
#39120=CARTESIAN_POINT('Ctrl Pts',(9.4500021963329,11.8316076987798,1.08333333333334));
#39121=CARTESIAN_POINT('Origin',(11.1410986251693,8.88472967648709,-1.08333333333333));
#39122=CARTESIAN_POINT('',(13.2594869773434,6.22835470309422,-1.08333333333333));
#39123=CARTESIAN_POINT('Origin',(11.1410986251693,8.88472967648709,-9.85584169237555E-16));
#39124=CARTESIAN_POINT('',(13.6377879061428,6.58029051604763,-1.08333333333333));
#39125=CARTESIAN_POINT('Origin',(11.1410986251693,8.88472967648709,-1.08333333333333));
#39126=CARTESIAN_POINT('',(13.6377879061428,6.58029051604763,1.08333333333333));
#39127=CARTESIAN_POINT('Ctrl Pts',(13.6377879061428,6.58029051604764,-1.08333333333332));
#39128=CARTESIAN_POINT('Ctrl Pts',(13.6907677796515,6.47048863474093,-0.727666221822788));
#39129=CARTESIAN_POINT('Ctrl Pts',(13.7154355939006,6.41687686636464,-0.352782973842773));
#39130=CARTESIAN_POINT('Ctrl Pts',(13.7154355939006,6.41687686636464,-9.86054494281319E-16));
#39131=CARTESIAN_POINT('Ctrl Pts',(13.7154355939006,6.41687686636464,0.352782973842772));
#39132=CARTESIAN_POINT('Ctrl Pts',(13.6907677796515,6.47048863474094,0.727666221822788));
#39133=CARTESIAN_POINT('Ctrl Pts',(13.6377879061428,6.58029051604764,1.08333333333332));
#39134=CARTESIAN_POINT('',(12.9276994994135,5.9947548451011,1.08333333333333));
#39135=CARTESIAN_POINT('Origin',(11.1410986251693,8.88472967648709,1.08333333333333));
#39136=CARTESIAN_POINT('',(12.9276994994135,5.9947548451011,-1.08333333333333));
#39137=CARTESIAN_POINT('Ctrl Pts',(12.9276994994135,5.9947548451011,1.08333333333333));
#39138=CARTESIAN_POINT('Ctrl Pts',(12.9759843593573,5.89062845864264,0.72592864797658));
#39139=CARTESIAN_POINT('Ctrl Pts',(12.9982133898606,5.84028669430273,0.352039859176989));
#39140=CARTESIAN_POINT('Ctrl Pts',(12.9982133898606,5.84028669430273,-9.85141416048961E-16));
#39141=CARTESIAN_POINT('Ctrl Pts',(12.9982133898606,5.84028669430273,-0.35203985917699));
#39142=CARTESIAN_POINT('Ctrl Pts',(12.9759843593573,5.89062845864264,-0.72592864797658));
#39143=CARTESIAN_POINT('Ctrl Pts',(12.9276994994135,5.9947548451011,-1.08333333333333));
#39144=CARTESIAN_POINT('Origin',(11.1410986251693,8.88472967648709,-1.08333333333333));
#39145=CARTESIAN_POINT('',(10.4434643792748,8.32838493021314,3.45272288248773));
#39146=CARTESIAN_POINT('Origin',(10.4434643792748,8.32838493021314,-9.23868777263706E-16));
#39147=CARTESIAN_POINT('',(11.8387328710639,9.44107442276105,3.45272288248773));
#39148=CARTESIAN_POINT('Origin',(11.8387328710639,9.44107442276104,-1.0472995612114E-15));
#39149=CARTESIAN_POINT('Origin',(0.,14.25,0.));
#39150=CARTESIAN_POINT('',(-3.35834339016074,14.7651959662676,-1.08333333333333));
#39151=CARTESIAN_POINT('',(-3.39763111739558,14.25,-1.08333333333333));
#39152=CARTESIAN_POINT('Origin',(1.55588456152529E-16,14.25,-1.08333333333333));
#39153=CARTESIAN_POINT('',(3.39763111739558,14.25,-1.08333333333333));
#39154=CARTESIAN_POINT('Origin',(0.,14.25,0.));
#39155=CARTESIAN_POINT('',(3.35834339016074,14.7651959662676,-1.08333333333333));
#39156=CARTESIAN_POINT('Origin',(0.,14.25,-1.08333333333333));
#39157=CARTESIAN_POINT('',(3.35834339016074,14.7651959662676,1.08333333333333));
#39158=CARTESIAN_POINT('Ctrl Pts',(3.35834339016074,14.7651959662676,-1.08333333333333));
#39159=CARTESIAN_POINT('Ctrl Pts',(3.47722236863702,14.7381569460943,-0.727666221822793));
#39160=CARTESIAN_POINT('Ctrl Pts',(3.53451786760282,14.7240166290356,-0.352782973842775));
#39161=CARTESIAN_POINT('Ctrl Pts',(3.53451786760282,14.7240166290356,0.));
#39162=CARTESIAN_POINT('Ctrl Pts',(3.53451786760282,14.7240166290356,0.352782973842776));
#39163=CARTESIAN_POINT('Ctrl Pts',(3.47722236863702,14.7381569460943,0.727666221822795));
#39164=CARTESIAN_POINT('Ctrl Pts',(3.35834339016074,14.7651959662676,1.08333333333333));
#39165=CARTESIAN_POINT('',(3.37340073180097,13.8449509750914,1.08333333333333));
#39166=CARTESIAN_POINT('Origin',(0.,14.25,1.08333333333333));
#39167=CARTESIAN_POINT('',(3.37340073180097,13.8449509750914,-1.08333333333333));
#39168=CARTESIAN_POINT('Ctrl Pts',(3.37340073180098,13.8449509750914,1.08333333333333));
#39169=CARTESIAN_POINT('Ctrl Pts',(3.48491513664897,13.8177798586608,0.725928647976577));
#39170=CARTESIAN_POINT('Ctrl Pts',(3.53813348671686,13.8037716378594,0.352039859176988));
#39171=CARTESIAN_POINT('Ctrl Pts',(3.53813348671686,13.8037716378594,0.));
#39172=CARTESIAN_POINT('Ctrl Pts',(3.53813348671686,13.8037716378594,-0.352039859176988));
#39173=CARTESIAN_POINT('Ctrl Pts',(3.48491513664897,13.8177798586608,-0.725928647976578));
#39174=CARTESIAN_POINT('Ctrl Pts',(3.37340073180098,13.8449509750914,-1.08333333333333));
#39175=CARTESIAN_POINT('Origin',(0.,14.25,-1.08333333333333));
#39176=CARTESIAN_POINT('',(-3.37340073180097,13.8449509750914,-1.08333333333333));
#39177=CARTESIAN_POINT('Origin',(1.55588456152529E-16,14.25,-1.08333333333333));
#39178=CARTESIAN_POINT('',(-3.37340073180097,13.8449509750914,1.08333333333333));
#39179=CARTESIAN_POINT('Ctrl Pts',(-3.37340073180098,13.8449509750914,-1.08333333333333));
#39180=CARTESIAN_POINT('Ctrl Pts',(-3.48491513664897,13.8177798586608,-0.725928647976578));
#39181=CARTESIAN_POINT('Ctrl Pts',(-3.53813348671686,13.8037716378594,-0.352039859176988));
#39182=CARTESIAN_POINT('Ctrl Pts',(-3.53813348671686,13.8037716378594,0.352039859176988));
#39183=CARTESIAN_POINT('Ctrl Pts',(-3.48491513664897,13.8177798586608,0.725928647976578));
#39184=CARTESIAN_POINT('Ctrl Pts',(-3.37340073180098,13.8449509750914,1.08333333333333));
#39185=CARTESIAN_POINT('',(-3.35834339016074,14.7651959662676,1.08333333333333));
#39186=CARTESIAN_POINT('Origin',(-1.5558845615253E-16,14.25,1.08333333333333));
#39187=CARTESIAN_POINT('Ctrl Pts',(-3.35834339016074,14.7651959662676,1.08333333333333));
#39188=CARTESIAN_POINT('Ctrl Pts',(-3.47722236863702,14.7381569460943,0.727666221822794));
#39189=CARTESIAN_POINT('Ctrl Pts',(-3.53451786760282,14.7240166290356,0.352782973842775));
#39190=CARTESIAN_POINT('Ctrl Pts',(-3.53451786760282,14.7240166290356,-0.352782973842776));
#39191=CARTESIAN_POINT('Ctrl Pts',(-3.47722236863702,14.7381569460943,-0.727666221822794));
#39192=CARTESIAN_POINT('Ctrl Pts',(-3.35834339016074,14.7651959662676,-1.08333333333333));
#39193=CARTESIAN_POINT('',(0.,13.3576923076923,3.45272288248773));
#39194=CARTESIAN_POINT('Origin',(0.,13.3576923076923,0.));
#39195=CARTESIAN_POINT('',(0.,15.1423076923077,3.45272288248773));
#39196=CARTESIAN_POINT('Origin',(0.,15.1423076923077,0.));
#39197=CARTESIAN_POINT('Origin',(0.,14.25,0.));
#39198=CARTESIAN_POINT('',(-4.85033905439415E-16,15.1423076923077,-3.96060240207311));
#39199=CARTESIAN_POINT('Origin',(0.,15.1423076923077,0.));
#39200=CARTESIAN_POINT('',(-4.85033905439415E-16,13.3576923076923,-3.96060240207311));
#39201=CARTESIAN_POINT('Origin',(-3.08592870035031E-16,14.25,-2.5198520116158));
#39202=CARTESIAN_POINT('Origin',(0.,13.3576923076923,0.));
#39203=CARTESIAN_POINT('',(-3.97254599103887,13.6850786752975,1.08333333333333));
#39204=CARTESIAN_POINT('',(-4.03631672677061,14.5944383081266,1.08333333333333));
#39205=CARTESIAN_POINT('Ctrl Pts',(-3.97254599103889,13.6850786752975,1.08333333333333));
#39206=CARTESIAN_POINT('Ctrl Pts',(-4.03699073486477,13.8609255570095,1.08333333333333));
#39207=CARTESIAN_POINT('Ctrl Pts',(-4.07292947680577,14.0696859538838,1.08333333333333));
#39208=CARTESIAN_POINT('Ctrl Pts',(-4.07292947680577,14.358906139038,1.08333333333333));
#39209=CARTESIAN_POINT('Ctrl Pts',(-4.06125577389194,14.4784021699804,1.08333333333333));
#39210=CARTESIAN_POINT('Ctrl Pts',(-4.03631672677123,14.5944383081267,1.08333333333333));
#39211=CARTESIAN_POINT('',(-3.97254599103887,13.6850786752975,-1.08333333333333));
#39212=CARTESIAN_POINT('Ctrl Pts',(-3.97254599103885,13.6850786752975,1.08333333333333));
#39213=CARTESIAN_POINT('Ctrl Pts',(-4.0055902844374,13.6754864779574,0.949270311030653));
#39214=CARTESIAN_POINT('Ctrl Pts',(-4.03241557892495,13.6675742096383,0.813521288368336));
#39215=CARTESIAN_POINT('Ctrl Pts',(-4.05298135839275,13.6614729113855,0.67660705210156));
#39216=CARTESIAN_POINT('Ctrl Pts',(-4.07056281760631,13.6562569784544,0.559560573778188));
#39217=CARTESIAN_POINT('Ctrl Pts',(-4.08356944187665,13.6523638057542,0.441662516279225));
#39218=CARTESIAN_POINT('Ctrl Pts',(-4.09196781162929,13.6498461320482,0.32323825833471));
#39219=CARTESIAN_POINT('Ctrl Pts',(-4.10167217606822,13.6469369456345,0.186398348762652));
#39220=CARTESIAN_POINT('Ctrl Pts',(-4.10519527746315,13.6458740742379,0.0492519096262281));
#39221=CARTESIAN_POINT('Ctrl Pts',(-4.1025698088094,13.6466633637621,-0.0876758270660229));
#39222=CARTESIAN_POINT('Ctrl Pts',(-4.09993672885708,13.6474549414561,-0.225000520654293));
#39223=CARTESIAN_POINT('Ctrl Pts',(-4.0911193595297,13.6501094100325,-0.362105241912746));
#39224=CARTESIAN_POINT('Ctrl Pts',(-4.07613560843688,13.6545823261509,-0.498460177595596));
#39225=CARTESIAN_POINT('Ctrl Pts',(-4.06108721528303,13.659074539074,-0.635403368116582));
#39226=CARTESIAN_POINT('Ctrl Pts',(-4.03981905948952,13.6654009235528,-0.771590289741077));
#39227=CARTESIAN_POINT('Ctrl Pts',(-4.01233468870309,13.673465922941,-0.906484242526326));
#39228=CARTESIAN_POINT('Ctrl Pts',(-4.00026996096645,13.6770061903378,-0.965698216399675));
#39229=CARTESIAN_POINT('Ctrl Pts',(-3.98700723595603,13.6808808214243,-1.02466304565388));
#39230=CARTESIAN_POINT('Ctrl Pts',(-3.97254599103885,13.6850786752975,-1.08333333333333));
#39231=CARTESIAN_POINT('',(-4.03631672677098,14.5944383081279,-1.08333333333333));
#39232=CARTESIAN_POINT('Ctrl Pts',(-3.97254599103889,13.6850786752975,-1.08333333333333));
#39233=CARTESIAN_POINT('Ctrl Pts',(-4.03718797255354,13.8614637488071,-1.08333333333333));
#39234=CARTESIAN_POINT('Ctrl Pts',(-4.07292947680577,14.0697175866198,-1.08333333333333));
#39235=CARTESIAN_POINT('Ctrl Pts',(-4.07292947680577,14.3589686276554,-1.08333333333333));
#39236=CARTESIAN_POINT('Ctrl Pts',(-4.06126656486658,14.4783519618466,-1.08333333333333));
#39237=CARTESIAN_POINT('Ctrl Pts',(-4.03631672677098,14.5944383081279,-1.08333333333333));
#39238=CARTESIAN_POINT('Ctrl Pts',(-4.03631672677125,14.5944383081264,-1.08333333333353));
#39239=CARTESIAN_POINT('Ctrl Pts',(-4.07239878927587,14.5844592579328,-0.956888632103535));
#39240=CARTESIAN_POINT('Ctrl Pts',(-4.10204391436992,14.576120838176,-0.828820583351431));
#39241=CARTESIAN_POINT('Ctrl Pts',(-4.12523046485396,14.5695557880246,-0.699646919262042));
#39242=CARTESIAN_POINT('Ctrl Pts',(-4.14829509982461,14.5630252570856,-0.571152453813459));
#39243=CARTESIAN_POINT('Ctrl Pts',(-4.16496899480084,14.5582495239489,-0.441563969171867));
#39244=CARTESIAN_POINT('Ctrl Pts',(-4.17521778805797,14.555309638438,-0.311391073638072));
#39245=CARTESIAN_POINT('Ctrl Pts',(-4.18538433378736,14.5523933457842,-0.182262827807668));
#39246=CARTESIAN_POINT('Ctrl Pts',(-4.18922853025337,14.5512835680019,-0.0525595133522669));
#39247=CARTESIAN_POINT('Ctrl Pts',(-4.18670294427272,14.5520101946411,0.0772214321944475));
#39248=CARTESIAN_POINT('Ctrl Pts',(-4.18498039512374,14.5525057826387,0.165737150534356));
#39249=CARTESIAN_POINT('Ctrl Pts',(-4.1802944723506,14.5538546098955,0.254288981130209));
#39250=CARTESIAN_POINT('Ctrl Pts',(-4.17262628304436,14.5560527668241,0.342719102199544));
#39251=CARTESIAN_POINT('Ctrl Pts',(-4.16106584445129,14.5593666727772,0.476034927301542));
#39252=CARTESIAN_POINT('Ctrl Pts',(-4.14279588034764,14.5645937486684,0.608312350205319));
#39253=CARTESIAN_POINT('Ctrl Pts',(-4.11795181407459,14.5716147048116,0.739057191236983));
#39254=CARTESIAN_POINT('Ctrl Pts',(-4.09589395251526,14.5778482769217,0.855139299993905));
#39255=CARTESIAN_POINT('Ctrl Pts',(-4.06865355383155,14.5854950604866,0.970013302477714));
#39256=CARTESIAN_POINT('Ctrl Pts',(-4.03631672677125,14.5944383081264,1.08333333333353));
#39257=CARTESIAN_POINT('',(4.0363167267713,14.5944383081264,1.08333333333333));
#39258=CARTESIAN_POINT('',(3.97254599103947,13.6850786752973,1.08333333333333));
#39259=CARTESIAN_POINT('Ctrl Pts',(4.0363167267713,14.5944383081264,1.08333333333333));
#39260=CARTESIAN_POINT('Ctrl Pts',(4.06125577389196,14.4784021699801,1.08333333333333));
#39261=CARTESIAN_POINT('Ctrl Pts',(4.07292947680577,14.3589061390379,1.08333333333333));
#39262=CARTESIAN_POINT('Ctrl Pts',(4.07292947680577,14.0696859538838,1.08333333333333));
#39263=CARTESIAN_POINT('Ctrl Pts',(4.03699073486477,13.8609255570095,1.08333333333333));
#39264=CARTESIAN_POINT('Ctrl Pts',(3.97254599103889,13.6850786752975,1.08333333333333));
#39265=CARTESIAN_POINT('',(4.0363167267713,14.5944383081264,-1.08333333333333));
#39266=CARTESIAN_POINT('Ctrl Pts',(4.0363167267713,14.5944383081264,1.08333333333333));
#39267=CARTESIAN_POINT('Ctrl Pts',(4.07267660468553,14.5843824238018,0.955915065626592));
#39268=CARTESIAN_POINT('Ctrl Pts',(4.10254364280131,14.5759803979714,0.826701571450557));
#39269=CARTESIAN_POINT('Ctrl Pts',(4.12584816889326,14.5693808768856,0.696211209492171));
#39270=CARTESIAN_POINT('Ctrl Pts',(4.14878536602558,14.5628853783063,0.567777653525462));
#39271=CARTESIAN_POINT('Ctrl Pts',(4.16536539316191,14.5581360328796,0.438107164856169));
#39272=CARTESIAN_POINT('Ctrl Pts',(4.17550906341001,14.5552260824043,0.307693975181436));
#39273=CARTESIAN_POINT('Ctrl Pts',(4.18345734283739,14.55294593144,0.205506064179161));
#39274=CARTESIAN_POINT('Ctrl Pts',(4.18745357006455,14.5517942140162,0.102862147740973));
#39275=CARTESIAN_POINT('Ctrl Pts',(4.18745357006455,14.5517942140162,-4.44089209850063E-16));
#39276=CARTESIAN_POINT('Ctrl Pts',(4.18745357006455,14.5517942140162,-0.13066680730557));
#39277=CARTESIAN_POINT('Ctrl Pts',(4.18100368362964,14.5536548201376,-0.261069786498731));
#39278=CARTESIAN_POINT('Ctrl Pts',(4.16817103415993,14.5573291670729,-0.390710450871123));
#39279=CARTESIAN_POINT('Ctrl Pts',(4.15518429935153,14.561047632956,-0.521907748246283));
#39280=CARTESIAN_POINT('Ctrl Pts',(4.13566054561854,14.5666236366129,-0.652324314224272));
#39281=CARTESIAN_POINT('Ctrl Pts',(4.10965488440249,14.5739568744946,-0.781443489202978));
#39282=CARTESIAN_POINT('Ctrl Pts',(4.08920880779353,14.5797223861759,-0.882959098491578));
#39283=CARTESIAN_POINT('Ctrl Pts',(4.06475571708163,14.586573067282,-0.983672743459539));
#39284=CARTESIAN_POINT('Ctrl Pts',(4.0363167267713,14.5944383081264,-1.08333333333333));
#39285=CARTESIAN_POINT('',(3.972545991042,13.685078675306,-1.08333333333333));
#39286=CARTESIAN_POINT('Ctrl Pts',(4.0363167267713,14.5944383081264,-1.08333333333333));
#39287=CARTESIAN_POINT('Ctrl Pts',(4.06125577389196,14.4784021699801,-1.08333333333333));
#39288=CARTESIAN_POINT('Ctrl Pts',(4.07292947680577,14.3589061390379,-1.08333333333333));
#39289=CARTESIAN_POINT('Ctrl Pts',(4.07292947680577,14.0696859538867,-1.08333333333333));
#39290=CARTESIAN_POINT('Ctrl Pts',(4.03699073486612,13.8609255570161,-1.08333333333333));
#39291=CARTESIAN_POINT('Ctrl Pts',(3.97254599104201,13.685078675306,-1.08333333333333));
#39292=CARTESIAN_POINT('Ctrl Pts',(3.97254599103891,13.6850786752974,-1.08333333333318));
#39293=CARTESIAN_POINT('Ctrl Pts',(4.00550358468898,13.6755116454224,-0.949622058007565));
#39294=CARTESIAN_POINT('Ctrl Pts',(4.03223833992508,13.667626413385,-0.814376693553222));
#39295=CARTESIAN_POINT('Ctrl Pts',(4.05275116551691,13.6615412011384,-0.678132403728152));
#39296=CARTESIAN_POINT('Ctrl Pts',(4.07316650047532,13.6554849098804,-0.542535637670838));
#39297=CARTESIAN_POINT('Ctrl Pts',(4.0874189867075,13.6512115628239,-0.40594941879892));
#39298=CARTESIAN_POINT('Ctrl Pts',(4.09549564973878,13.6487880554638,-0.268901316711817));
#39299=CARTESIAN_POINT('Ctrl Pts',(4.10076932144717,13.6472056219574,-0.179415511018788));
#39300=CARTESIAN_POINT('Ctrl Pts',(4.10340966592831,13.6464108509735,-0.0897327832366672));
#39301=CARTESIAN_POINT('Ctrl Pts',(4.10340966592831,13.6464108509735,4.66293670342566E-15));
#39302=CARTESIAN_POINT('Ctrl Pts',(4.10340966592831,13.6464108509735,0.137573936980382));
#39303=CARTESIAN_POINT('Ctrl Pts',(4.09720533291532,13.6482810316174,0.274951212619736));
#39304=CARTESIAN_POINT('Ctrl Pts',(4.08483748845152,13.6519816397819,0.41161240621476));
#39305=CARTESIAN_POINT('Ctrl Pts',(4.07237395114171,13.6557108803995,0.549330978772818));
#39306=CARTESIAN_POINT('Ctrl Pts',(4.05365110225785,13.6612989721827,0.686322345436846));
#39307=CARTESIAN_POINT('Ctrl Pts',(4.02869583028489,13.6686542829587,0.822054935347102));
#39308=CARTESIAN_POINT('Ctrl Pts',(4.01257796374822,13.6734048590114,0.909720570537157));
#39309=CARTESIAN_POINT('Ctrl Pts',(3.99385994844905,13.6788915953345,0.996861109122728));
#39310=CARTESIAN_POINT('Ctrl Pts',(3.97254599103891,13.6850786752974,1.08333333333318));
#39311=CARTESIAN_POINT('Origin',(0.,0.,1.08333333333333));
#39312=CARTESIAN_POINT('Origin',(0.,0.,-1.08333333333333));
#39313=CARTESIAN_POINT('Origin',(0.,0.,1.08333333333333));
#39314=CARTESIAN_POINT('Origin',(0.,0.,1.08333333333333));
#39315=CARTESIAN_POINT('Origin',(0.,0.,1.08333333333333));
#39316=CARTESIAN_POINT('Origin',(0.,0.,-1.08333333333333));
#39317=CARTESIAN_POINT('Origin',(0.,0.,1.08333333333333));
#39318=CARTESIAN_POINT('Origin',(0.,0.,-1.08333333333333));
#39319=CARTESIAN_POINT('Origin',(0.,15.1423076923077,3.45272288248773));
#39320=CARTESIAN_POINT('Origin',(0.,13.3576923076923,3.45272288248773));
#39321=CARTESIAN_POINT('Origin',(0.,0.,1.08333333333333));
#39322=CARTESIAN_POINT('Origin',(0.,0.,1.08333333333333));
#39323=CARTESIAN_POINT('Origin',(0.,0.,1.08333333333333));
#39324=CARTESIAN_POINT('Origin',(0.,0.,-1.08333333333333));
#39325=CARTESIAN_POINT('Origin',(0.,0.,-1.08333333333333));
#39326=CARTESIAN_POINT('Origin',(0.,0.,-1.08333333333333));
#39327=CARTESIAN_POINT('Origin',(0.,0.,1.08333333333333));
#39328=CARTESIAN_POINT('Origin',(0.,0.,1.08333333333333));
#39329=CARTESIAN_POINT('Origin',(10.4434643792748,8.32838493021314,3.45272288248773));
#39330=CARTESIAN_POINT('Origin',(11.8387328710639,9.44107442276104,3.45272288248773));
#39331=CARTESIAN_POINT('Origin',(-1.55588456152528E-16,7.49274514625042E-17,
-1.08333333333333));
#39332=CARTESIAN_POINT('Origin',(-1.55588456152528E-16,7.49274514625042E-17,
-1.08333333333333));
#39333=CARTESIAN_POINT('Origin',(-1.55588456152528E-16,7.49274514625042E-17,
-1.08333333333333));
#39334=CARTESIAN_POINT('Origin',(1.55588456152528E-16,-7.49274514625042E-17,
1.08333333333333));
#39335=CARTESIAN_POINT('Origin',(1.55588456152528E-16,-7.49274514625042E-17,
1.08333333333333));
#39336=CARTESIAN_POINT('Origin',(1.55588456152528E-16,-7.49274514625042E-17,
1.08333333333333));
#39337=CARTESIAN_POINT('Origin',(1.55588456152528E-16,-7.49274514625042E-17,
1.08333333333333));
#39338=CARTESIAN_POINT('Origin',(1.55588456152528E-16,-7.49274514625042E-17,
1.08333333333333));
#39339=CARTESIAN_POINT('Origin',(1.94015631396094E-16,-2.43287906657286E-16,
1.08333333333333));
#39340=CARTESIAN_POINT('Origin',(1.94015631396094E-16,-2.43287906657286E-16,
1.08333333333333));
#39341=CARTESIAN_POINT('Origin',(-1.94015631396094E-16,2.43287906657286E-16,
-1.08333333333333));
#39342=CARTESIAN_POINT('Origin',(1.94015631396094E-16,-2.43287906657286E-16,
1.08333333333333));
#39343=CARTESIAN_POINT('Origin',(-1.94015631396094E-16,2.43287906657286E-16,
-1.08333333333333));
#39344=CARTESIAN_POINT('Origin',(1.94015631396094E-16,-2.43287906657286E-16,
1.08333333333333));
#39345=CARTESIAN_POINT('Origin',(-1.94015631396094E-16,2.43287906657286E-16,
-1.08333333333333));
#39346=CARTESIAN_POINT('Origin',(1.94015631396094E-16,-2.43287906657286E-16,
1.08333333333333));
#39347=CARTESIAN_POINT('Origin',(13.0227870731057,-2.97236616780865,3.45272288248773));
#39348=CARTESIAN_POINT('Origin',(14.7626584240763,-3.36948044994605,3.45272288248773));
#39349=CARTESIAN_POINT('Origin',(-1.94015631396094E-16,2.43287906657286E-16,
-1.08333333333333));
#39350=CARTESIAN_POINT('Origin',(-1.94015631396094E-16,2.43287906657286E-16,
-1.08333333333333));
#39351=CARTESIAN_POINT('Origin',(-1.94015631396094E-16,2.43287906657286E-16,
-1.08333333333333));
#39352=CARTESIAN_POINT('Origin',(1.94015631396094E-16,-2.43287906657286E-16,
1.08333333333333));
#39353=CARTESIAN_POINT('Origin',(1.94015631396094E-16,-2.43287906657286E-16,
1.08333333333333));
#39354=CARTESIAN_POINT('Origin',(1.94015631396094E-16,-2.43287906657286E-16,
1.08333333333333));
#39355=CARTESIAN_POINT('Origin',(1.94015631396094E-16,-2.43287906657286E-16,
1.08333333333333));
#39356=CARTESIAN_POINT('Origin',(1.94015631396094E-16,-2.43287906657286E-16,
1.08333333333333));
#39357=CARTESIAN_POINT('Origin',(8.63450790007668E-17,-3.78302508895262E-16,
1.08333333333333));
#39358=CARTESIAN_POINT('Origin',(8.63450790007668E-17,-3.78302508895262E-16,
1.08333333333333));
#39359=CARTESIAN_POINT('Origin',(-8.63450790007668E-17,3.78302508895262E-16,
-1.08333333333333));
#39360=CARTESIAN_POINT('Origin',(8.63450790007668E-17,-3.78302508895262E-16,
1.08333333333333));
#39361=CARTESIAN_POINT('Origin',(-8.63450790007668E-17,3.78302508895262E-16,
-1.08333333333333));
#39362=CARTESIAN_POINT('Origin',(8.63450790007668E-17,-3.78302508895262E-16,
1.08333333333333));
#39363=CARTESIAN_POINT('Origin',(-8.63450790007668E-17,3.78302508895262E-16,
-1.08333333333333));
#39364=CARTESIAN_POINT('Origin',(8.63450790007668E-17,-3.78302508895262E-16,
1.08333333333333));
#39365=CARTESIAN_POINT('Origin',(5.79568548444348,-12.0348649162504,3.45272288248773));
#39366=CARTESIAN_POINT('Origin',(6.57000108040713,-13.6427478189685,3.45272288248772));
#39367=CARTESIAN_POINT('Origin',(-8.63450790007668E-17,3.78302508895262E-16,
-1.08333333333333));
#39368=CARTESIAN_POINT('Origin',(-8.63450790007668E-17,3.78302508895262E-16,
-1.08333333333333));
#39369=CARTESIAN_POINT('Origin',(-8.63450790007668E-17,3.78302508895262E-16,
-1.08333333333333));
#39370=CARTESIAN_POINT('Origin',(8.63450790007668E-17,-3.78302508895262E-16,
1.08333333333333));
#39371=CARTESIAN_POINT('Origin',(8.63450790007668E-17,-3.78302508895262E-16,
1.08333333333333));
#39372=CARTESIAN_POINT('Origin',(8.63450790007668E-17,-3.78302508895262E-16,
1.08333333333333));
#39373=CARTESIAN_POINT('Origin',(8.63450790007668E-17,-3.78302508895262E-16,
1.08333333333333));
#39374=CARTESIAN_POINT('Origin',(8.63450790007668E-17,-3.78302508895262E-16,
1.08333333333333));
#39375=CARTESIAN_POINT('Origin',(-8.63450790007644E-17,-3.78302508895264E-16,
1.08333333333333));
#39376=CARTESIAN_POINT('Origin',(-8.63450790007644E-17,-3.78302508895264E-16,
1.08333333333333));
#39377=CARTESIAN_POINT('Origin',(8.63450790007644E-17,3.78302508895264E-16,
-1.08333333333333));
#39378=CARTESIAN_POINT('Origin',(-8.63450790007644E-17,-3.78302508895264E-16,
1.08333333333333));
#39379=CARTESIAN_POINT('Origin',(8.63450790007644E-17,3.78302508895264E-16,
-1.08333333333333));
#39380=CARTESIAN_POINT('Origin',(-8.63450790007644E-17,-3.78302508895264E-16,
1.08333333333333));
#39381=CARTESIAN_POINT('Origin',(8.63450790007644E-17,3.78302508895264E-16,
-1.08333333333333));
#39382=CARTESIAN_POINT('Origin',(-8.63450790007644E-17,-3.78302508895264E-16,
1.08333333333333));
#39383=CARTESIAN_POINT('Origin',(-5.79568548444331,-12.0348649162504,3.45272288248773));
#39384=CARTESIAN_POINT('Origin',(-6.57000108040694,-13.6427478189686,3.45272288248772));
#39385=CARTESIAN_POINT('Origin',(8.63450790007644E-17,3.78302508895264E-16,
-1.08333333333333));
#39386=CARTESIAN_POINT('Origin',(8.63450790007644E-17,3.78302508895264E-16,
-1.08333333333333));
#39387=CARTESIAN_POINT('Origin',(8.63450790007644E-17,3.78302508895264E-16,
-1.08333333333333));
#39388=CARTESIAN_POINT('Origin',(-8.63450790007644E-17,-3.78302508895264E-16,
1.08333333333333));
#39389=CARTESIAN_POINT('Origin',(-8.63450790007644E-17,-3.78302508895264E-16,
1.08333333333333));
#39390=CARTESIAN_POINT('Origin',(-8.63450790007644E-17,-3.78302508895264E-16,
1.08333333333333));
#39391=CARTESIAN_POINT('Origin',(-8.63450790007644E-17,-3.78302508895264E-16,
1.08333333333333));
#39392=CARTESIAN_POINT('Origin',(-8.63450790007644E-17,-3.78302508895264E-16,
1.08333333333333));
#39393=CARTESIAN_POINT('Origin',(-1.94015631396093E-16,-2.43287906657289E-16,
1.08333333333333));
#39394=CARTESIAN_POINT('Origin',(-1.94015631396093E-16,-2.43287906657289E-16,
1.08333333333333));
#39395=CARTESIAN_POINT('Origin',(1.94015631396093E-16,2.43287906657289E-16,
-1.08333333333333));
#39396=CARTESIAN_POINT('Origin',(-1.94015631396093E-16,-2.43287906657289E-16,
1.08333333333333));
#39397=CARTESIAN_POINT('Origin',(1.94015631396093E-16,2.43287906657289E-16,
-1.08333333333333));
#39398=CARTESIAN_POINT('Origin',(-1.94015631396093E-16,-2.43287906657289E-16,
1.08333333333333));
#39399=CARTESIAN_POINT('Origin',(1.94015631396093E-16,2.43287906657289E-16,
-1.08333333333333));
#39400=CARTESIAN_POINT('Origin',(-1.94015631396093E-16,-2.43287906657289E-16,
1.08333333333333));
#39401=CARTESIAN_POINT('Origin',(-13.0227870731057,-2.97236616780882,3.45272288248773));
#39402=CARTESIAN_POINT('Origin',(-14.7626584240763,-3.36948044994625,3.45272288248773));
#39403=CARTESIAN_POINT('Origin',(1.94015631396093E-16,2.43287906657289E-16,
-1.08333333333333));
#39404=CARTESIAN_POINT('Origin',(1.94015631396093E-16,2.43287906657289E-16,
-1.08333333333333));
#39405=CARTESIAN_POINT('Origin',(1.94015631396093E-16,2.43287906657289E-16,
-1.08333333333333));
#39406=CARTESIAN_POINT('Origin',(-1.94015631396093E-16,-2.43287906657289E-16,
1.08333333333333));
#39407=CARTESIAN_POINT('Origin',(-1.94015631396093E-16,-2.43287906657289E-16,
1.08333333333333));
#39408=CARTESIAN_POINT('Origin',(-1.94015631396093E-16,-2.43287906657289E-16,
1.08333333333333));
#39409=CARTESIAN_POINT('Origin',(-1.94015631396093E-16,-2.43287906657289E-16,
1.08333333333333));
#39410=CARTESIAN_POINT('Origin',(-1.94015631396093E-16,-2.43287906657289E-16,
1.08333333333333));
#39411=CARTESIAN_POINT('Origin',(-1.55588456152529E-16,-7.49274514625064E-17,
1.08333333333333));
#39412=CARTESIAN_POINT('Origin',(-1.55588456152529E-16,-7.49274514625064E-17,
1.08333333333333));
#39413=CARTESIAN_POINT('Origin',(1.55588456152529E-16,7.49274514625064E-17,
-1.08333333333333));
#39414=CARTESIAN_POINT('Origin',(-1.55588456152529E-16,-7.49274514625064E-17,
1.08333333333333));
#39415=CARTESIAN_POINT('Origin',(1.55588456152529E-16,7.49274514625064E-17,
-1.08333333333333));
#39416=CARTESIAN_POINT('Origin',(-1.55588456152529E-16,-7.49274514625064E-17,
1.08333333333333));
#39417=CARTESIAN_POINT('Origin',(1.55588456152529E-16,7.49274514625064E-17,
-1.08333333333333));
#39418=CARTESIAN_POINT('Origin',(-1.55588456152529E-16,-7.49274514625064E-17,
1.08333333333333));
#39419=CARTESIAN_POINT('Origin',(-10.4434643792749,8.32838493021299,3.45272288248773));
#39420=CARTESIAN_POINT('Origin',(-11.838732871064,9.44107442276088,3.45272288248773));
#39421=CARTESIAN_POINT('Origin',(1.55588456152529E-16,7.49274514625064E-17,
-1.08333333333333));
#39422=CARTESIAN_POINT('Origin',(1.55588456152529E-16,7.49274514625064E-17,
-1.08333333333333));
#39423=CARTESIAN_POINT('Origin',(1.55588456152529E-16,7.49274514625064E-17,
-1.08333333333333));
#39424=CARTESIAN_POINT('Origin',(-1.55588456152529E-16,-7.49274514625064E-17,
1.08333333333333));
#39425=CARTESIAN_POINT('Origin',(-1.55588456152529E-16,-7.49274514625064E-17,
1.08333333333333));
#39426=CARTESIAN_POINT('Origin',(-1.55588456152529E-16,-7.49274514625064E-17,
1.08333333333333));
#39427=CARTESIAN_POINT('Origin',(-1.55588456152529E-16,-7.49274514625064E-17,
1.08333333333333));
#39428=CARTESIAN_POINT('Origin',(-1.55588456152529E-16,-7.49274514625064E-17,
1.08333333333333));
#39429=CARTESIAN_POINT('Origin',(0.,0.,1.08333333333333));
#39430=CARTESIAN_POINT('Origin',(0.,0.,1.08333333333333));
#39431=CARTESIAN_POINT('Origin',(0.,0.,1.08333333333333));
#39432=CARTESIAN_POINT('Origin',(0.,0.,-1.08333333333333));
#39433=CARTESIAN_POINT('Origin',(0.,0.,-1.08333333333333));
#39434=CARTESIAN_POINT('Origin',(0.,0.,-1.08333333333333));
#39435=CARTESIAN_POINT('Origin',(0.,0.,1.08333333333333));
#39436=CARTESIAN_POINT('Origin',(0.,0.,1.08333333333333));
#39437=CARTESIAN_POINT('',(0.,0.,0.));
#39438=CARTESIAN_POINT('Origin',(0.,1.73472347597681E-15,-6.67403582113016E-15));
#39439=CARTESIAN_POINT('',(1.52656933693714E-15,12.4653846153846,3.0875));
#39440=CARTESIAN_POINT('Origin',(0.,6.26866080313552E-16,3.0875));
#39441=CARTESIAN_POINT('',(-1.52656933693714E-15,12.4653846153846,-3.0875));
#39442=CARTESIAN_POINT('Origin',(-1.74512168878498E-15,14.25,-4.05635328795269E-15));
#39443=CARTESIAN_POINT('Origin',(0.,1.76119517802379E-15,-3.0875));
#39444=CARTESIAN_POINT('Origin',(0.,1.56496838953657E-16,5.64807088834312));
#39445=CARTESIAN_POINT('',(9.67029207191279E-16,7.64278544417155,5.99278544417156));
#39446=CARTESIAN_POINT('',(-9.35971273077467E-16,-7.64278544417155,5.99278544417156));
#39447=CARTESIAN_POINT('Origin',(0.,9.31738023414375E-17,5.99278544417156));
#39448=CARTESIAN_POINT('Origin',(0.,9.31738023414375E-17,5.99278544417156));
#39449=CARTESIAN_POINT('',(-9.18485099360515E-16,-7.5,5.64807088834312));
#39450=CARTESIAN_POINT('Origin',(-9.78186630818948E-16,-7.9875,5.64807088834312));
#39451=CARTESIAN_POINT('',(9.18485099360515E-16,7.5,5.64807088834312));
#39452=CARTESIAN_POINT('Origin',(0.,1.56496838953657E-16,5.64807088834312));
#39453=CARTESIAN_POINT('Origin',(0.,1.56496838953657E-16,5.64807088834312));
#39454=CARTESIAN_POINT('Origin',(0.,2.23156441938368E-15,-5.64807088834312));
#39455=CARTESIAN_POINT('',(9.18485099360515E-16,7.5,-5.64807088834312));
#39456=CARTESIAN_POINT('',(-9.18485099360515E-16,-7.5,-5.64807088834312));
#39457=CARTESIAN_POINT('Origin',(0.,2.23156441938368E-15,-5.64807088834312));
#39458=CARTESIAN_POINT('Origin',(0.,2.23156441938368E-15,-5.64807088834312));
#39459=CARTESIAN_POINT('',(-9.35971273077467E-16,-7.64278544417155,-5.99278544417156));
#39460=CARTESIAN_POINT('Origin',(-9.78186630818948E-16,-7.9875,-5.64807088834312));
#39461=CARTESIAN_POINT('Origin',(0.,2.2948874559959E-15,-5.99278544417156));
#39462=CARTESIAN_POINT('Origin',(0.,-9.99635681210842E-31,6.5));
#39463=CARTESIAN_POINT('',(-9.98087141305092E-16,8.14999999999999,6.50000000000001));
#39464=CARTESIAN_POINT('',(-9.98087141305092E-16,8.14999999999999,6.5));
#39465=CARTESIAN_POINT('Origin',(0.,-9.99635681210842E-31,6.5));
#39466=CARTESIAN_POINT('Origin',(0.,0.,6.5));
#39467=CARTESIAN_POINT('',(-9.18485099360515E-16,7.5,6.5));
#39468=CARTESIAN_POINT('Origin',(0.,2.26865819542047E-15,-5.85));
#39469=CARTESIAN_POINT('',(-9.98087141305091E-16,-8.14999999999998,-6.50000000000001));
#39470=CARTESIAN_POINT('',(-9.18485099360515E-16,-7.5,-5.85));
#39471=CARTESIAN_POINT('Origin',(0.,2.38806125833734E-15,-6.50000000000001));
#39472=CARTESIAN_POINT('Origin',(0.,0.,6.5));
#39473=CARTESIAN_POINT('',(-1.52656933693714E-15,12.4653846153846,-6.50000000000001));
#39474=CARTESIAN_POINT('',(-1.52656933693714E-15,12.4653846153846,6.5));
#39475=CARTESIAN_POINT('Origin',(0.,2.38806125833734E-15,-6.50000000000001));
#39476=CARTESIAN_POINT('Origin',(0.,0.,6.5));
#39477=CARTESIAN_POINT('',(-1.52656933693714E-15,12.4653846153846,6.50000000000001));
#39478=CARTESIAN_POINT('Origin',(0.,-1.17267830746035E-30,6.50000000000001));
#39479=CARTESIAN_POINT('',(-1.52656933693714E-15,12.4653846153846,6.5));
#39480=CARTESIAN_POINT('Origin',(0.,8.14999999999999,6.50000000000001));
#39481=CARTESIAN_POINT('Origin',(0.,8.14999999999999,-6.50000000000001));
#39482=CARTESIAN_POINT('Origin',(0.,14.25,-4.07195060716495E-15));
#39483=CARTESIAN_POINT('',(-3.56616156686793,14.25,-4.07195060716495E-15));
#39484=CARTESIAN_POINT('',(3.56616156686793,14.25,-4.07195060716495E-15));
#39485=CARTESIAN_POINT('Origin',(0.,14.25,-4.07195060716495E-15));
#39486=CARTESIAN_POINT('Origin',(11.1410986251694,8.88472967648693,-5.05753477640253E-15));
#39487=CARTESIAN_POINT('',(8.91763325644669,11.6728670610318,-4.54536224786764E-15));
#39488=CARTESIAN_POINT('',(13.3645639938921,6.09659229194206,-5.56970730493742E-15));
#39489=CARTESIAN_POINT('Origin',(11.1410986251694,8.88472967648693,-5.05753477640253E-15));
#39490=CARTESIAN_POINT('Origin',(13.892722748591,-3.17092330887753,-7.27212230242621E-15));
#39491=CARTESIAN_POINT('',(14.6862683510896,0.305827142012077,-6.6334536057588E-15));
#39492=CARTESIAN_POINT('',(13.0991771460924,-6.64767375976714,-7.91079099909362E-15));
#39493=CARTESIAN_POINT('Origin',(13.892722748591,-3.17092330887753,-7.27212230242621E-15));
#39494=CARTESIAN_POINT('Origin',(6.18284328242512,-12.8388063676095,-9.04808360878726E-15));
#39495=CARTESIAN_POINT('',(9.39584383208325,-11.2915068526795,-8.76384929904507E-15));
#39496=CARTESIAN_POINT('',(2.96984273276699,-14.3861058825395,-9.33231791852945E-15));
#39497=CARTESIAN_POINT('Origin',(6.18284328242512,-12.8388063676095,-9.04808360878726E-15));
#39498=CARTESIAN_POINT('Origin',(-6.1828432824253,-12.8388063676094,-9.04808360878725E-15));
#39499=CARTESIAN_POINT('',(-2.9698427327672,-14.3861058825394,-9.33231791852944E-15));
#39500=CARTESIAN_POINT('',(-9.39584383208341,-11.2915068526794,-8.76384929904506E-15));
#39501=CARTESIAN_POINT('Origin',(-6.1828432824253,-12.8388063676094,-9.04808360878725E-15));
#39502=CARTESIAN_POINT('Origin',(-13.892722748591,-3.17092330887735,-7.27212230242617E-15));
#39503=CARTESIAN_POINT('',(-13.0991771460925,-6.64767375976697,-7.91079099909359E-15));
#39504=CARTESIAN_POINT('',(-14.6862683510895,0.30582714201227,-6.63345360575876E-15));
#39505=CARTESIAN_POINT('Origin',(-13.892722748591,-3.17092330887735,-7.27212230242617E-15));
#39506=CARTESIAN_POINT('Origin',(-11.1410986251693,8.88472967648709,-5.0575347764025E-15));
#39507=CARTESIAN_POINT('',(-13.3645639938921,6.09659229194225,-5.56970730493739E-15));
#39508=CARTESIAN_POINT('',(-8.91763325644655,11.6728670610319,-4.54536224786761E-15));
#39509=CARTESIAN_POINT('Origin',(-11.1410986251693,8.88472967648709,-5.0575347764025E-15));
#39510=CARTESIAN_POINT('Origin',(0.,1.07462756625201E-17,6.44149999999999));
#39511=CARTESIAN_POINT('',(-1.99949495950787E-15,-16.3271153846154,6.49999999999999));
#39512=CARTESIAN_POINT('Origin',(0.,2.01169401222323E-30,6.49999999999999));
#39513=CARTESIAN_POINT('',(-1.99233077573286E-15,-16.2686153846154,6.44149999999999));
#39514=CARTESIAN_POINT('Origin',(-1.99949495950788E-15,-16.3271153846154,
6.44149999999999));
#39515=CARTESIAN_POINT('',(1.99233077573286E-15,16.2686153846154,6.44149999999999));
#39516=CARTESIAN_POINT('Origin',(0.,1.07462756625199E-17,6.44149999999999));
#39517=CARTESIAN_POINT('Origin',(0.,1.07462756625199E-17,6.44149999999999));
#39518=CARTESIAN_POINT('Origin',(0.,1.30149338579385E-16,5.7915));
#39519=CARTESIAN_POINT('',(-1.96367404063281E-15,16.0346153846154,5.7915));
#39520=CARTESIAN_POINT('Origin',(0.,1.30149338579385E-16,5.7915));
#39521=CARTESIAN_POINT('',(-1.97083822440782E-15,16.0931153846154,5.85));
#39522=CARTESIAN_POINT('Origin',(-1.97083822440783E-15,16.0931153846154,
5.7915));
#39523=CARTESIAN_POINT('Origin',(0.,1.19403062916867E-16,5.85));
#39524=CARTESIAN_POINT('Origin',(0.,2.37731498267482E-15,-6.44150000000001));
#39525=CARTESIAN_POINT('',(-1.99949495950787E-15,16.3271153846154,-6.5));
#39526=CARTESIAN_POINT('Origin',(0.,2.38806125833734E-15,-6.50000000000001));
#39527=CARTESIAN_POINT('',(-1.99233077573286E-15,16.2686153846154,-6.4415));
#39528=CARTESIAN_POINT('Origin',(-1.99949495950788E-15,16.3271153846154,
-6.44150000000001));
#39529=CARTESIAN_POINT('Origin',(0.,2.37731498267482E-15,-6.44150000000001));
#39530=CARTESIAN_POINT('Origin',(0.,2.25791191975795E-15,-5.7915));
#39531=CARTESIAN_POINT('',(1.96367404063281E-15,16.0346153846154,-5.7915));
#39532=CARTESIAN_POINT('',(-1.96367404063282E-15,-16.0346153846154,-5.7915));
#39533=CARTESIAN_POINT('Origin',(0.,2.25791191975795E-15,-5.7915));
#39534=CARTESIAN_POINT('Origin',(0.,2.25791191975795E-15,-5.7915));
#39535=CARTESIAN_POINT('',(-1.97083822440782E-15,-16.0931153846154,-5.85000000000001));
#39536=CARTESIAN_POINT('Origin',(-1.97083822440783E-15,-16.0931153846154,
-5.7915));
#39537=CARTESIAN_POINT('Origin',(0.,2.26865819542047E-15,-5.85));
#39538=CARTESIAN_POINT('Origin',(0.,0.,6.5));
#39539=CARTESIAN_POINT('',(-2.16636878649169E-15,17.6897435897436,5.85));
#39540=CARTESIAN_POINT('Origin',(0.,1.19403062916867E-16,5.85));
#39541=CARTESIAN_POINT('',(-2.16636878649169E-15,17.6897435897436,6.084));
#39542=CARTESIAN_POINT('',(-2.16636878649169E-15,17.6897435897436,6.5));
#39543=CARTESIAN_POINT('Origin',(0.,7.6417960266795E-17,6.084));
#39544=CARTESIAN_POINT('Origin',(0.,0.,6.5));
#39545=CARTESIAN_POINT('',(-1.99233077573286E-15,16.2686153846154,6.084));
#39546=CARTESIAN_POINT('Origin',(0.,7.6417960266795E-17,6.084));
#39547=CARTESIAN_POINT('',(-1.99233077573286E-15,16.2686153846154,6.5));
#39548=CARTESIAN_POINT('Origin',(0.,0.,6.5));
#39549=CARTESIAN_POINT('',(-1.96367404063281E-15,16.0346153846154,-3.0875));
#39550=CARTESIAN_POINT('',(-1.96367404063282E-15,16.0346153846154,6.5));
#39551=CARTESIAN_POINT('Origin',(0.,1.76119517802379E-15,-3.08750000000001));
#39552=CARTESIAN_POINT('Origin',(0.,1.73472347597681E-15,-6.67403582113016E-15));
#39553=CARTESIAN_POINT('',(-1.96367404063281E-15,16.0346153846154,3.0875));
#39554=CARTESIAN_POINT('Origin',(-1.74512168878498E-15,14.25,-4.05635328795269E-15));
#39555=CARTESIAN_POINT('Origin',(0.,6.26866080313552E-16,3.08749999999999));
#39556=CARTESIAN_POINT('Origin',(0.,0.,6.5));
#39557=CARTESIAN_POINT('',(-1.96367404063282E-15,16.0346153846154,6.5));
#39558=CARTESIAN_POINT('Origin',(0.,0.,6.5));
#39559=CARTESIAN_POINT('',(-1.99233077573286E-15,16.2686153846154,-6.084));
#39560=CARTESIAN_POINT('',(-1.99233077573286E-15,16.2686153846154,6.5));
#39561=CARTESIAN_POINT('Origin',(0.,2.31164329807054E-15,-6.084));
#39562=CARTESIAN_POINT('Origin',(0.,0.,6.5));
#39563=CARTESIAN_POINT('',(-2.16636878649169E-15,17.6897435897436,-6.084));
#39564=CARTESIAN_POINT('Origin',(0.,2.31164329807054E-15,-6.084));
#39565=CARTESIAN_POINT('',(-2.16636878649169E-15,17.6897435897436,-5.85));
#39566=CARTESIAN_POINT('',(-2.16636878649169E-15,17.6897435897436,6.5));
#39567=CARTESIAN_POINT('Origin',(0.,2.26865819542047E-15,-5.85));
#39568=CARTESIAN_POINT('Origin',(0.,2.38806125833734E-15,-6.50000000000001));
#39569=CARTESIAN_POINT('',(-2.57175827820944E-15,21.,-5.85));
#39570=CARTESIAN_POINT('Origin',(0.,2.26865819542047E-15,-5.85000000000001));
#39571=CARTESIAN_POINT('',(-2.49215623626487E-15,20.35,-6.5));
#39572=CARTESIAN_POINT('',(-2.49215623626486E-15,20.35,-6.50000000000001));
#39573=CARTESIAN_POINT('Origin',(0.,2.38806125833734E-15,-6.50000000000001));
#39574=CARTESIAN_POINT('Origin',(0.,1.19403062916869E-16,5.84999999999999));
#39575=CARTESIAN_POINT('',(2.57175827820944E-15,21.,5.84999999999999));
#39576=CARTESIAN_POINT('',(-2.57175827820944E-15,-21.,5.84999999999999));
#39577=CARTESIAN_POINT('Origin',(0.,1.19403062916869E-16,5.84999999999999));
#39578=CARTESIAN_POINT('',(-2.49215623626487E-15,-20.35,6.49999999999999));
#39579=CARTESIAN_POINT('',(-2.57175827820944E-15,-21.,5.84999999999999));
#39580=CARTESIAN_POINT('Origin',(0.,1.96135664184276E-30,6.49999999999999));
#39581=CARTESIAN_POINT('Origin',(0.,1.19403062916869E-16,5.84999999999999));
#39582=CARTESIAN_POINT('Origin',(0.,0.,6.5));
#39583=CARTESIAN_POINT('',(-2.57175827820944E-15,21.,6.5));
#39584=CARTESIAN_POINT('Origin',(0.,20.35,6.49999999999999));
#39585=CARTESIAN_POINT('Origin',(0.,20.35,-6.5));
#39586=CARTESIAN_POINT('Origin',(0.,16.0346153846154,-5.85));
#39587=CARTESIAN_POINT('Origin',(0.,16.2686153846154,-6.084));
#39588=CARTESIAN_POINT('Origin',(0.,16.2686153846154,6.084));
#39589=CARTESIAN_POINT('Origin',(0.,16.0346153846154,5.85));
#39590=CARTESIAN_POINT('Origin',(-11.1410986251694,8.88472967648693,-9.85584169237584E-16));
#39591=CARTESIAN_POINT('',(-11.838732871064,9.44107442276088,-3.96060240207311));
#39592=CARTESIAN_POINT('Origin',(-11.838732871064,9.44107442276088,-1.04729956121144E-15));
#39593=CARTESIAN_POINT('',(-10.4434643792749,8.32838493021299,-3.96060240207311));
#39594=CARTESIAN_POINT('Origin',(-11.1410986251694,8.88472967648693,-2.5198520116158));
#39595=CARTESIAN_POINT('Origin',(-10.4434643792749,8.32838493021299,-9.23868777263733E-16));
#39596=CARTESIAN_POINT('',(-13.176267261227,5.42664547033602,1.08333333333333));
#39597=CARTESIAN_POINT('',(-13.9269936544441,5.94376395877182,1.08333333333333));
#39598=CARTESIAN_POINT('Ctrl Pts',(-13.176267261227,5.42664547033603,1.08333333333333));
#39599=CARTESIAN_POINT('Ctrl Pts',(-13.3544742809805,5.48608062863209,1.08333333333333));
#39600=CARTESIAN_POINT('Ctrl Pts',(-13.5395781511317,5.58798093945111,1.08333333333333));
#39601=CARTESIAN_POINT('Ctrl Pts',(-13.7657237213497,5.76832601371359,1.08333333333333));
#39602=CARTESIAN_POINT('Ctrl Pts',(-13.851789663848,5.85187873682469,1.08333333333333));
#39603=CARTESIAN_POINT('Ctrl Pts',(-13.9269936544446,5.9437639587714,1.08333333333333));
#39604=CARTESIAN_POINT('',(-13.176267261227,5.42664547033602,-1.08333333333333));
#39605=CARTESIAN_POINT('Ctrl Pts',(-13.176267261227,5.426645470336,1.08333333333333));
#39606=CARTESIAN_POINT('Ctrl Pts',(-13.1893705593041,5.39482976422217,0.949270311030458));
#39607=CARTESIAN_POINT('Ctrl Pts',(-13.1999097963793,5.36892368585873,0.813521288367943));
#39608=CARTESIAN_POINT('Ctrl Pts',(-13.2079621630869,5.34904061477063,0.676607052100963));
#39609=CARTESIAN_POINT('Ctrl Pts',(-13.2148460430323,5.33204279546006,0.559560573777783));
#39610=CARTESIAN_POINT('Ctrl Pts',(-13.2199117356377,5.31944645364942,0.441662516279014));
#39611=CARTESIAN_POINT('Ctrl Pts',(-13.2231796369648,5.31131059989529,0.323238258334693));
#39612=CARTESIAN_POINT('Ctrl Pts',(-13.2269557156994,5.30190957419894,0.186398348762648));
#39613=CARTESIAN_POINT('Ctrl Pts',(-13.2283213471704,5.29849241313602,0.0492519096262365));
#39614=CARTESIAN_POINT('Ctrl Pts',(-13.2273014856384,5.30103720115478,-0.0876758270660023));
#39615=CARTESIAN_POINT('Ctrl Pts',(-13.2262786675027,5.30358936657696,-0.225000520654269));
#39616=CARTESIAN_POINT('Ctrl Pts',(-13.2228564747501,5.31213809759637,-0.362105241912721));
#39617=CARTESIAN_POINT('Ctrl Pts',(-13.21701132539,5.32664168351063,-0.498460177595569));
#39618=CARTESIAN_POINT('Ctrl Pts',(-13.2111409592134,5.34120783998416,-0.635403368116636));
#39619=CARTESIAN_POINT('Ctrl Pts',(-13.2028266475275,5.36178038996277,-0.771590289741212));
#39620=CARTESIAN_POINT('Ctrl Pts',(-13.1919958930595,5.38829698119001,-0.90648424252654));
#39621=CARTESIAN_POINT('Ctrl Pts',(-13.1872415508606,5.39993688577963,-0.965698216399817));
#39622=CARTESIAN_POINT('Ctrl Pts',(-13.1820016856382,5.4127218947045,-1.02466304565395));
#39623=CARTESIAN_POINT('Ctrl Pts',(-13.176267261227,5.426645470336,-1.08333333333333));
#39624=CARTESIAN_POINT('',(-13.9269936544455,5.94376395877242,-1.08333333333333));
#39625=CARTESIAN_POINT('Ctrl Pts',(-13.176267261227,5.42664547033603,-1.08333333333333));
#39626=CARTESIAN_POINT('Ctrl Pts',(-13.3544742809805,5.48608062863209,-1.08333333333333));
#39627=CARTESIAN_POINT('Ctrl Pts',(-13.5395781511317,5.58798093945111,-1.08333333333333));
#39628=CARTESIAN_POINT('Ctrl Pts',(-13.76572372135,5.76832601371385,-1.08333333333333));
#39629=CARTESIAN_POINT('Ctrl Pts',(-13.8517896638487,5.85187873682532,-1.08333333333333));
#39630=CARTESIAN_POINT('Ctrl Pts',(-13.9269936544455,5.94376395877245,-1.08333333333333));
#39631=CARTESIAN_POINT('Ctrl Pts',(-13.9269936544444,5.94376395877114,-1.08333333333355));
#39632=CARTESIAN_POINT('Ctrl Pts',(-13.9416885168396,5.90933203032471,-0.95688863210348));
#39633=CARTESIAN_POINT('Ctrl Pts',(-13.9536527109306,5.88095561854246,-0.828820583351296));
#39634=CARTESIAN_POINT('Ctrl Pts',(-13.9629765258054,5.85873440158612,-0.699646919261824));
#39635=CARTESIAN_POINT('Ctrl Pts',(-13.9722513158078,5.83663002439321,-0.571152453813156));
#39636=CARTESIAN_POINT('Ctrl Pts',(-13.9789135007646,5.82061622745832,-0.441563969171476));
#39637=CARTESIAN_POINT('Ctrl Pts',(-13.9830050237945,5.81077040959789,-0.311391073637591));
#39638=CARTESIAN_POINT('Ctrl Pts',(-13.9870637119681,5.80100360534983,-0.182262827807202));
#39639=CARTESIAN_POINT('Ctrl Pts',(-13.9885928700523,5.79730615639837,-0.0525595133518154));
#39640=CARTESIAN_POINT('Ctrl Pts',(-13.9875862925321,5.79973378332902,0.0772214321948836));
#39641=CARTESIAN_POINT('Ctrl Pts',(-13.9868997670034,5.80138952054624,0.16573715053464));
#39642=CARTESIAN_POINT('Ctrl Pts',(-13.9850326975558,5.80589410253377,0.25428898113034));
#39643=CARTESIAN_POINT('Ctrl Pts',(-13.9819702480149,5.81325986277477,0.342719102199523));
#39644=CARTESIAN_POINT('Ctrl Pts',(-13.9773533484511,5.82436436418404,0.476034927301742));
#39645=CARTESIAN_POINT('Ctrl Pts',(-13.9700489046451,5.84190742581559,0.608312350205735));
#39646=CARTESIAN_POINT('Ctrl Pts',(-13.9600480872369,5.86570879353503,0.739057191237609));
#39647=CARTESIAN_POINT('Ctrl Pts',(-13.9511688384278,5.8868408927778,0.855139299994326));
#39648=CARTESIAN_POINT('Ctrl Pts',(-13.9401632237806,5.9129059856334,0.970013302477931));
#39649=CARTESIAN_POINT('Ctrl Pts',(-13.9269936544444,5.94376395877114,1.08333333333355));
#39650=CARTESIAN_POINT('',(-8.89378902201695,12.2552029391753,1.08333333333333));
#39651=CARTESIAN_POINT('',(-8.22258343557141,11.6383685130291,1.08333333333333));
#39652=CARTESIAN_POINT('Ctrl Pts',(-8.89378902201693,12.2552029391753,1.08333333333333));
#39653=CARTESIAN_POINT('Ctrl Pts',(-8.78747309219938,12.2023308550396,1.08333333333333));
#39654=CARTESIAN_POINT('Ctrl Pts',(-8.68686373639314,12.1370149953911,1.08333333333333));
#39655=CARTESIAN_POINT('Ctrl Pts',(-8.46071816617524,11.9566699211287,1.08333333333333));
#39656=CARTESIAN_POINT('Ctrl Pts',(-8.32018322283281,11.7988819437994,1.08333333333333));
#39657=CARTESIAN_POINT('Ctrl Pts',(-8.22258343557192,11.6383685130288,1.08333333333333));
#39658=CARTESIAN_POINT('',(-8.89378902201695,12.2552029391753,-1.08333333333333));
#39659=CARTESIAN_POINT('Ctrl Pts',(-8.89378902201696,12.2552029391753,1.08333333333333));
#39660=CARTESIAN_POINT('Ctrl Pts',(-8.86325700199161,12.2773604951023,0.955915065626613));
#39661=CARTESIAN_POINT('Ctrl Pts',(-8.83806624000395,12.2954729083691,0.8267015714506));
#39662=CARTESIAN_POINT('Ctrl Pts',(-8.81837639229442,12.3095783864577,0.696211209492237));
#39663=CARTESIAN_POINT('Ctrl Pts',(-8.79899689851553,12.3234615321731,0.567777653525536));
#39664=CARTESIAN_POINT('Ctrl Pts',(-8.7849462329058,12.3334631509294,0.438107164856251));
#39665=CARTESIAN_POINT('Ctrl Pts',(-8.77634666705863,12.3395794672318,0.307693975181527));
#39666=CARTESIAN_POINT('Ctrl Pts',(-8.76960830208466,12.3443720314467,0.205506064179221));
#39667=CARTESIAN_POINT('Ctrl Pts',(-8.76621624622179,12.3467783236356,0.102862147741002));
#39668=CARTESIAN_POINT('Ctrl Pts',(-8.76621624622179,12.3467783236356,-2.44249065417534E-15));
#39669=CARTESIAN_POINT('Ctrl Pts',(-8.76621624622179,12.3467783236356,-0.130666807305558));
#39670=CARTESIAN_POINT('Ctrl Pts',(-8.77169236507929,12.3428956683044,-0.261069786498707));
#39671=CARTESIAN_POINT('Ctrl Pts',(-8.78256611126601,12.3351536167882,-0.390710450871087));
#39672=CARTESIAN_POINT('Ctrl Pts',(-8.79357042167237,12.3273186042172,-0.521907748246256));
#39673=CARTESIAN_POINT('Ctrl Pts',(-8.8101027782242,12.315530900308,-0.652324314224256));
#39674=CARTESIAN_POINT('Ctrl Pts',(-8.83205039902736,12.2997710546807,-0.781443489202971));
#39675=CARTESIAN_POINT('Ctrl Pts',(-8.84930597782606,12.2873804060307,-0.882959098491573));
#39676=CARTESIAN_POINT('Ctrl Pts',(-8.86990830867396,12.2725335396739,-0.983672743459536));
#39677=CARTESIAN_POINT('Ctrl Pts',(-8.89378902201696,12.2552029391753,-1.08333333333333));
#39678=CARTESIAN_POINT('',(-8.22258343557665,11.6383685130365,-1.08333333333333));
#39679=CARTESIAN_POINT('Ctrl Pts',(-8.89378902201693,12.2552029391753,-1.08333333333333));
#39680=CARTESIAN_POINT('Ctrl Pts',(-8.78747309219938,12.2023308550396,-1.08333333333333));
#39681=CARTESIAN_POINT('Ctrl Pts',(-8.68686373639314,12.1370149953911,-1.08333333333333));
#39682=CARTESIAN_POINT('Ctrl Pts',(-8.46071816617751,11.9566699211305,-1.08333333333333));
#39683=CARTESIAN_POINT('Ctrl Pts',(-8.32018322283717,11.7988819438045,-1.08333333333333));
#39684=CARTESIAN_POINT('Ctrl Pts',(-8.22258343557662,11.6383685130365,-1.08333333333333));
#39685=CARTESIAN_POINT('Ctrl Pts',(-8.22258343557191,11.6383685130287,-1.08333333333318));
#39686=CARTESIAN_POINT('Ctrl Pts',(-8.19455490688727,11.6581708517696,-0.949622058007629));
#39687=CARTESIAN_POINT('Ctrl Pts',(-8.17172113698899,11.6741565633286,-0.814376693553349));
#39688=CARTESIAN_POINT('Ctrl Pts',(-8.15417398891324,11.6864000683928,-0.678132403728345));
#39689=CARTESIAN_POINT('Ctrl Pts',(-8.13671023659264,11.698585384152,-0.542535637671064));
#39690=CARTESIAN_POINT('Ctrl Pts',(-8.12448291951145,11.7070640382822,-0.405949418799179));
#39691=CARTESIAN_POINT('Ctrl Pts',(-8.11755242812626,11.7118675955896,-0.268901316712111));
#39692=CARTESIAN_POINT('Ctrl Pts',(-8.11302715126356,11.7150040870061,-0.179415511018989));
#39693=CARTESIAN_POINT('Ctrl Pts',(-8.11075954642953,11.7165728598427,-0.0897327832367744));
#39694=CARTESIAN_POINT('Ctrl Pts',(-8.11075954642953,11.7165728598427,-9.99200722162641E-15));
#39695=CARTESIAN_POINT('Ctrl Pts',(-8.11075954642954,11.7165728598427,0.137573936980354));
#39696=CARTESIAN_POINT('Ctrl Pts',(-8.11609005089583,11.7128881555246,0.274951212619692));
#39697=CARTESIAN_POINT('Ctrl Pts',(-8.12669452775723,11.7055258768037,0.4116124062147));
#39698=CARTESIAN_POINT('Ctrl Pts',(-8.13738105388554,11.6981066344457,0.549330978772881));
#39699=CARTESIAN_POINT('Ctrl Pts',(-8.15342350530942,11.6869526399855,0.686322345437031));
#39700=CARTESIAN_POINT('Ctrl Pts',(-8.17473347641523,11.6720277839618,0.822054935347404));
#39701=CARTESIAN_POINT('Ctrl Pts',(-8.18849695174643,11.662388264195,0.909720570537357));
#39702=CARTESIAN_POINT('Ctrl Pts',(-8.20445714658991,11.6511748546878,0.996861109122827));
#39703=CARTESIAN_POINT('Ctrl Pts',(-8.22258343557191,11.6383685130287,1.08333333333318));
#39704=CARTESIAN_POINT('Origin',(-11.1410986251694,8.88472967648693,-9.85584169237584E-16));
#39705=CARTESIAN_POINT('',(-13.6377879061429,6.58029051604744,-1.08333333333333));
#39706=CARTESIAN_POINT('',(-13.2594869773434,6.22835470309403,-1.08333333333333));
#39707=CARTESIAN_POINT('Origin',(-11.1410986251694,8.88472967648693,-1.08333333333333));
#39708=CARTESIAN_POINT('',(-9.02271027299537,11.5411046498798,-1.08333333333333));
#39709=CARTESIAN_POINT('Origin',(-11.1410986251694,8.88472967648693,-9.85584169237584E-16));
#39710=CARTESIAN_POINT('',(-9.45000219633307,11.8316076987796,-1.08333333333333));
#39711=CARTESIAN_POINT('Origin',(-11.1410986251694,8.88472967648693,-1.08333333333333));
#39712=CARTESIAN_POINT('',(-9.45000219633307,11.8316076987796,1.08333333333333));
#39713=CARTESIAN_POINT('Ctrl Pts',(-9.45000219633306,11.8316076987796,-1.08333333333334));
#39714=CARTESIAN_POINT('Ctrl Pts',(-9.35474240837113,11.9076924734257,-0.727666221822799));
#39715=CARTESIAN_POINT('Ctrl Pts',(-9.30796390402501,11.9436715548398,-0.352782973842778));
#39716=CARTESIAN_POINT('Ctrl Pts',(-9.30796390402501,11.9436715548398,-5.10741104345864E-16));
#39717=CARTESIAN_POINT('Ctrl Pts',(-9.30796390402501,11.9436715548398,0.352782973842777));
#39718=CARTESIAN_POINT('Ctrl Pts',(-9.35474240837113,11.9076924734257,0.727666221822798));
#39719=CARTESIAN_POINT('Ctrl Pts',(-9.45000219633306,11.8316076987796,1.08333333333334));
#39720=CARTESIAN_POINT('',(-8.72113759169224,11.2696166353063,1.08333333333333));
#39721=CARTESIAN_POINT('Origin',(-11.1410986251694,8.88472967648693,1.08333333333333));
#39722=CARTESIAN_POINT('',(-8.72113759169224,11.2696166353063,-1.08333333333333));
#39723=CARTESIAN_POINT('Ctrl Pts',(-8.72113759169222,11.2696166353063,1.08333333333334));
#39724=CARTESIAN_POINT('Ctrl Pts',(-8.63036626326988,11.3398611937656,0.725928647976584));
#39725=CARTESIAN_POINT('Ctrl Pts',(-8.58623309669495,11.3727349924818,0.352039859176991));
#39726=CARTESIAN_POINT('Ctrl Pts',(-8.58623309669495,11.3727349924818,-4.46574186955748E-16));
#39727=CARTESIAN_POINT('Ctrl Pts',(-8.58623309669495,11.3727349924818,-0.352039859176992));
#39728=CARTESIAN_POINT('Ctrl Pts',(-8.63036626326988,11.3398611937656,-0.725928647976585));
#39729=CARTESIAN_POINT('Ctrl Pts',(-8.72113759169222,11.2696166353063,-1.08333333333334));
#39730=CARTESIAN_POINT('Origin',(-11.1410986251694,8.88472967648693,-1.08333333333333));
#39731=CARTESIAN_POINT('',(-12.9276994994136,5.99475484510091,-1.08333333333333));
#39732=CARTESIAN_POINT('Origin',(-11.1410986251694,8.88472967648693,-1.08333333333333));
#39733=CARTESIAN_POINT('',(-12.9276994994136,5.99475484510091,1.08333333333333));
#39734=CARTESIAN_POINT('Ctrl Pts',(-12.9276994994136,5.99475484510092,-1.08333333333333));
#39735=CARTESIAN_POINT('Ctrl Pts',(-12.9759843593574,5.89062845864246,-0.725928647976576));
#39736=CARTESIAN_POINT('Ctrl Pts',(-12.9982133898606,5.84028669430256,-0.352039859176989));
#39737=CARTESIAN_POINT('Ctrl Pts',(-12.9982133898606,5.84028669430256,0.352039859176986));
#39738=CARTESIAN_POINT('Ctrl Pts',(-12.9759843593574,5.89062845864246,0.725928647976574));
#39739=CARTESIAN_POINT('Ctrl Pts',(-12.9276994994136,5.99475484510092,1.08333333333332));
#39740=CARTESIAN_POINT('',(-13.6377879061429,6.58029051604744,1.08333333333333));
#39741=CARTESIAN_POINT('Origin',(-11.1410986251694,8.88472967648693,1.08333333333333));
#39742=CARTESIAN_POINT('Ctrl Pts',(-13.6377879061429,6.58029051604746,1.08333333333332));
#39743=CARTESIAN_POINT('Ctrl Pts',(-13.6907677796516,6.47048863474076,0.727666221822783));
#39744=CARTESIAN_POINT('Ctrl Pts',(-13.7154355939007,6.41687686636447,0.352782973842769));
#39745=CARTESIAN_POINT('Ctrl Pts',(-13.7154355939007,6.41687686636447,-0.352782973842771));
#39746=CARTESIAN_POINT('Ctrl Pts',(-13.6907677796516,6.47048863474076,-0.727666221822784));
#39747=CARTESIAN_POINT('Ctrl Pts',(-13.6377879061429,6.58029051604746,-1.08333333333332));
#39748=CARTESIAN_POINT('',(-10.4434643792749,8.32838493021299,3.45272288248773));
#39749=CARTESIAN_POINT('Origin',(-10.4434643792749,8.32838493021299,-9.23868777263733E-16));
#39750=CARTESIAN_POINT('',(-11.838732871064,9.44107442276088,3.45272288248773));
#39751=CARTESIAN_POINT('Origin',(-11.838732871064,9.44107442276088,-1.04729956121144E-15));
#39752=CARTESIAN_POINT('Origin',(-13.892722748591,-3.17092330887753,-3.20017169526126E-15));
#39753=CARTESIAN_POINT('',(-14.7626584240763,-3.36948044994625,-3.96060240207311));
#39754=CARTESIAN_POINT('Origin',(-14.7626584240763,-3.36948044994625,-3.40056031423578E-15));
#39755=CARTESIAN_POINT('',(-13.0227870731057,-2.97236616780882,-3.96060240207311));
#39756=CARTESIAN_POINT('Origin',(-13.892722748591,-3.17092330887753,-2.5198520116158));
#39757=CARTESIAN_POINT('Origin',(-13.0227870731057,-2.97236616780882,-2.99978307628674E-15));
#39758=CARTESIAN_POINT('',(-12.4579905368413,-6.91816245718267,1.08333333333333));
#39759=CARTESIAN_POINT('',(-13.3303603014234,-7.18268588222789,1.08333333333333));
#39760=CARTESIAN_POINT('Ctrl Pts',(-12.4579905368413,-6.91816245718265,
1.08333333333333));
#39761=CARTESIAN_POINT('Ctrl Pts',(-12.6155690741986,-7.02043310055334,
1.08333333333333));
#39762=CARTESIAN_POINT('Ctrl Pts',(-12.8106483205941,-7.10161932916232,
1.08333333333333));
#39763=CARTESIAN_POINT('Ctrl Pts',(-13.0926472341269,-7.16598374096129,
1.08333333333333));
#39764=CARTESIAN_POINT('Ctrl Pts',(-13.211632620936,-7.18117853359748,1.08333333333333));
#39765=CARTESIAN_POINT('Ctrl Pts',(-13.3303603014234,-7.18268588222786,
1.08333333333333));
#39766=CARTESIAN_POINT('',(-12.4579905368413,-6.91816245718267,-1.08333333333334));
#39767=CARTESIAN_POINT('Ctrl Pts',(-12.4579905368413,-6.91816245718269,
1.08333333333333));
#39768=CARTESIAN_POINT('Ctrl Pts',(-12.4412857888864,-6.94824379644449,
0.949270311030495));
#39769=CARTESIAN_POINT('Ctrl Pts',(-12.4276027080703,-6.97263587945683,
0.813521288368019));
#39770=CARTESIAN_POINT('Ctrl Pts',(-12.4170780656485,-6.99132836531023,
0.676607052101084));
#39771=CARTESIAN_POINT('Ctrl Pts',(-12.4080806643214,-7.0073083663671,0.559560573777871));
#39772=CARTESIAN_POINT('Ctrl Pts',(-12.4013908554087,-7.01912257498617,
0.441662516279072));
#39773=CARTESIAN_POINT('Ctrl Pts',(-12.3970674919579,-7.02675014497037,
0.323238258334728));
#39774=CARTESIAN_POINT('Ctrl Pts',(-12.392071820683,-7.03556384585404,0.186398348762656));
#39775=CARTESIAN_POINT('Ctrl Pts',(-12.3902516338786,-7.03876210460556,
0.0492519096262199));
#39776=CARTESIAN_POINT('Ctrl Pts',(-12.3916053560034,-7.03637809537454,
-0.0876758270660418));
#39777=CARTESIAN_POINT('Ctrl Pts',(-12.3929630026022,-7.03398717484178,
-0.22500052065431));
#39778=CARTESIAN_POINT('Ctrl Pts',(-12.3975129673671,-7.02598155019929,
-0.36210524191276));
#39779=CARTESIAN_POINT('Ctrl Pts',(-12.4052079364271,-7.0123687905019,-0.498460177595606));
#39780=CARTESIAN_POINT('Ctrl Pts',(-12.4129361026924,-6.99869730339788,
-0.635403368116707));
#39781=CARTESIAN_POINT('Ctrl Pts',(-12.4238364813948,-6.97937013765694,
-0.771590289741313));
#39782=CARTESIAN_POINT('Ctrl Pts',(-12.4378151222667,-6.9543694886247,-0.906484242526672));
#39783=CARTESIAN_POINT('Ctrl Pts',(-12.4439512822522,-6.94339503240897,
-0.965698216399908));
#39784=CARTESIAN_POINT('Ctrl Pts',(-12.450680002204,-6.93132701813286,-1.024663045654));
#39785=CARTESIAN_POINT('Ctrl Pts',(-12.4579905368413,-6.91816245718269,
-1.08333333333334));
#39786=CARTESIAN_POINT('',(-13.3303603014234,-7.18268588222787,-1.08333333333334));
#39787=CARTESIAN_POINT('Ctrl Pts',(-12.4579905368413,-6.91816245718265,
-1.08333333333333));
#39788=CARTESIAN_POINT('Ctrl Pts',(-12.6150882655077,-7.02012104908378,
-1.08333333333333));
#39789=CARTESIAN_POINT('Ctrl Pts',(-12.8106174809568,-7.10161229021636,
-1.08333333333333));
#39790=CARTESIAN_POINT('Ctrl Pts',(-13.0925863122299,-7.16596983593587,
-1.08333333333333));
#39791=CARTESIAN_POINT('Ctrl Pts',(-13.2116839714656,-7.18117918553602,
-1.08333333333333));
#39792=CARTESIAN_POINT('Ctrl Pts',(-13.3303603014234,-7.18268588222786,
-1.08333333333333));
#39793=CARTESIAN_POINT('Ctrl Pts',(-13.3303603014234,-7.18268588222788,
-1.08333333333333));
#39794=CARTESIAN_POINT('Ctrl Pts',(-13.312602432605,-7.21564274452362,-0.9568886321034));
#39795=CARTESIAN_POINT('Ctrl Pts',(-13.2978764135175,-7.24268913148589,
-0.828820583351364));
#39796=CARTESIAN_POINT('Ctrl Pts',(-13.2863164700111,-7.26383348564883,
-0.699646919262042));
#39797=CARTESIAN_POINT('Ctrl Pts',(-13.2748173090022,-7.28486666222222,
-0.571152453813466));
#39798=CARTESIAN_POINT('Ctrl Pts',(-13.2664510227833,-7.30005980724142,
-0.441563969171881));
#39799=CARTESIAN_POINT('Ctrl Pts',(-13.2613042752926,-7.30939745578436,
-0.311391073638092));
#39800=CARTESIAN_POINT('Ctrl Pts',(-13.2561988309335,-7.3186601688214,-0.182262827807686));
#39801=CARTESIAN_POINT('Ctrl Pts',(-13.2542614634094,-7.32216103446744,
-0.0525595133522827));
#39802=CARTESIAN_POINT('Ctrl Pts',(-13.2555318677528,-7.31986045983868,
0.0772214321944347));
#39803=CARTESIAN_POINT('Ctrl Pts',(-13.2563983335701,-7.31829137729732,
0.165737150534351));
#39804=CARTESIAN_POINT('Ctrl Pts',(-13.2587560588234,-7.31402308269238,
0.254288981130211));
#39805=CARTESIAN_POINT('Ctrl Pts',(-13.2626054360146,-7.30703628683457,
0.342719102199554));
#39806=CARTESIAN_POINT('Ctrl Pts',(-13.2684086950193,-7.29650310602083,
0.476034927301584));
#39807=CARTESIAN_POINT('Ctrl Pts',(-13.2775701666804,-7.27985434187078,
0.608312350205395));
#39808=CARTESIAN_POINT('Ctrl Pts',(-13.2899434176249,-7.25719547792734,
0.739057191237093));
#39809=CARTESIAN_POINT('Ctrl Pts',(-13.3009290370229,-7.23707775329796,
0.855139299993907));
#39810=CARTESIAN_POINT('Ctrl Pts',(-13.3144456587151,-7.21222189770289,
0.970013302477609));
#39811=CARTESIAN_POINT('Ctrl Pts',(-13.3303603014234,-7.18268588222788,
1.08333333333332));
#39812=CARTESIAN_POINT('',(-15.1266902369927,0.68754979644356,1.08333333333333));
#39813=CARTESIAN_POINT('',(-14.2259398250621,0.827729480997533,1.08333333333333));
#39814=CARTESIAN_POINT('Ctrl Pts',(-15.1266902369927,0.687549796443589,
1.08333333333333));
#39815=CARTESIAN_POINT('Ctrl Pts',(-15.0191128271494,0.737684039417719,
1.08333333333333));
#39816=CARTESIAN_POINT('Ctrl Pts',(-14.905210454464,0.775655426636244,1.08333333333333));
#39817=CARTESIAN_POINT('Ctrl Pts',(-14.6232416231909,0.840012972355744,
1.08333333333333));
#39818=CARTESIAN_POINT('Ctrl Pts',(-14.411718162898,0.851428848194329,1.08333333333333));
#39819=CARTESIAN_POINT('Ctrl Pts',(-14.2259398250622,0.827729480996923,
1.08333333333333));
#39820=CARTESIAN_POINT('',(-15.1266902369927,0.687549796443561,-1.08333333333334));
#39821=CARTESIAN_POINT('Ctrl Pts',(-15.1266902369927,0.687549796443564,
1.08333333333333));
#39822=CARTESIAN_POINT('Ctrl Pts',(-15.1249773086751,0.725235701077295,
0.955915065626697));
#39823=CARTESIAN_POINT('Ctrl Pts',(-15.1234319803901,0.756223536825465,
0.826701571450772));
#39824=CARTESIAN_POINT('Ctrl Pts',(-15.122183667988,0.780412301388329,0.696211209492499));
#39825=CARTESIAN_POINT('Ctrl Pts',(-15.1209550316477,0.804219799510246,
0.567777653525797));
#39826=CARTESIAN_POINT('Ctrl Pts',(-15.12001416535,0.821440959530219,0.438107164856512));
#39827=CARTESIAN_POINT('Ctrl Pts',(-15.1194343523859,0.83197783168462,0.307693975181787));
#39828=CARTESIAN_POINT('Ctrl Pts',(-15.1189800281283,0.840234212474348,
0.205506064179395));
#39829=CARTESIAN_POINT('Ctrl Pts',(-15.1187464308798,0.844386527178334,
0.102862147741089));
#39830=CARTESIAN_POINT('Ctrl Pts',(-15.1187464308798,0.844386527178334,
-1.99840144432528E-15));
#39831=CARTESIAN_POINT('Ctrl Pts',(-15.1187464308798,0.844386527178334,
-0.130666807305563));
#39832=CARTESIAN_POINT('Ctrl Pts',(-15.1191251529677,0.837684329050672,
-0.261069786498716));
#39833=CARTESIAN_POINT('Ctrl Pts',(-15.1198518432089,0.824355801783686,
-0.3907104508711));
#39834=CARTESIAN_POINT('Ctrl Pts',(-15.1205872590302,0.810867235029684,
-0.521907748246278));
#39835=CARTESIAN_POINT('Ctrl Pts',(-15.1216790167187,0.790592205023353,
-0.652324314224286));
#39836=CARTESIAN_POINT('Ctrl Pts',(-15.1230415909943,0.763606761086714,
-0.78144348920301));
#39837=CARTESIAN_POINT('Ctrl Pts',(-15.1241128691977,0.742390363261972,
-0.882959098491598));
#39838=CARTESIAN_POINT('Ctrl Pts',(-15.1253504648421,0.717025942629857,
-0.983672743459549));
#39839=CARTESIAN_POINT('Ctrl Pts',(-15.1266902369927,0.687549796443564,
-1.08333333333333));
#39840=CARTESIAN_POINT('',(-14.2259398250711,0.827729480998061,-1.08333333333334));
#39841=CARTESIAN_POINT('Ctrl Pts',(-15.1266902369927,0.687549796443589,
-1.08333333333333));
#39842=CARTESIAN_POINT('Ctrl Pts',(-15.0191128271494,0.73768403941772,-1.08333333333333));
#39843=CARTESIAN_POINT('Ctrl Pts',(-14.905210454464,0.775655426636245,-1.08333333333333));
#39844=CARTESIAN_POINT('Ctrl Pts',(-14.6232416231937,0.840012972355103,
-1.08333333333333));
#39845=CARTESIAN_POINT('Ctrl Pts',(-14.4117181629048,0.851428848194163,
-1.08333333333333));
#39846=CARTESIAN_POINT('Ctrl Pts',(-14.2259398250711,0.827729480998062,
-1.08333333333333));
#39847=CARTESIAN_POINT('Ctrl Pts',(-14.2259398250621,0.827729480996948,
-1.08333333333319));
#39848=CARTESIAN_POINT('Ctrl Pts',(-14.2239464151202,0.86198962338768,-0.949622058007746));
#39849=CARTESIAN_POINT('Ctrl Pts',(-14.2222079250172,0.889808711690097,
-0.814376693553578));
#39850=CARTESIAN_POINT('Ctrl Pts',(-14.2208398148552,0.911161325029729,
-0.678132403728685));
#39851=CARTESIAN_POINT('Ctrl Pts',(-14.2194782068654,0.932412456504284,
-0.542535637671376));
#39852=CARTESIAN_POINT('Ctrl Pts',(-14.2184834780892,0.947258512328182,
-0.405949418799462));
#39853=CARTESIAN_POINT('Ctrl Pts',(-14.2179179597194,0.955671957675903,
-0.268901316712362));
#39854=CARTESIAN_POINT('Ctrl Pts',(-14.2175487034788,0.961165532005871,
-0.179415511019154));
#39855=CARTESIAN_POINT('Ctrl Pts',(-14.2173613909827,0.963916530719958,
-0.0897327832368514));
#39856=CARTESIAN_POINT('Ctrl Pts',(-14.2173613909827,0.963916530719958,
1.77635683940025E-15));
#39857=CARTESIAN_POINT('Ctrl Pts',(-14.2173613909827,0.963916530719959,
0.137573936980362));
#39858=CARTESIAN_POINT('Ctrl Pts',(-14.2178040883167,0.957451598945575,
0.274951212619699));
#39859=CARTESIAN_POINT('Ctrl Pts',(-14.2186598102071,0.944570379379332,
0.411612406214706));
#39860=CARTESIAN_POINT('Ctrl Pts',(-14.2195221530139,0.931589494866292,
0.549330978772852));
#39861=CARTESIAN_POINT('Ctrl Pts',(-14.2208039138492,0.912092599491199,
0.686322345436968));
#39862=CARTESIAN_POINT('Ctrl Pts',(-14.222421741201,0.886126297665223,0.82205493534731));
#39863=CARTESIAN_POINT('Ctrl Pts',(-14.2234666476786,0.869355437073727,
0.909720570537294));
#39864=CARTESIAN_POINT('Ctrl Pts',(-14.2246506698206,0.849885807806941,
0.996861109122796));
#39865=CARTESIAN_POINT('Ctrl Pts',(-14.2259398250621,0.827729480996951,
1.08333333333318));
#39866=CARTESIAN_POINT('Origin',(-13.892722748591,-3.17092330887753,-3.20017169526126E-15));
#39867=CARTESIAN_POINT('',(-13.6476999686241,-6.55970790622096,-1.08333333333334));
#39868=CARTESIAN_POINT('',(-13.1366786991091,-6.483368720524,-1.08333333333334));
#39869=CARTESIAN_POINT('Origin',(-13.892722748591,-3.17092330887753,-1.08333333333334));
#39870=CARTESIAN_POINT('',(-14.6487667980729,0.141522102768936,-1.08333333333334));
#39871=CARTESIAN_POINT('Origin',(-13.892722748591,-3.17092330887753,-3.20017169526126E-15));
#39872=CARTESIAN_POINT('',(-15.1423033840733,-0.0114224867028857,-1.08333333333334));
#39873=CARTESIAN_POINT('Origin',(-13.892722748591,-3.17092330887753,-1.08333333333334));
#39874=CARTESIAN_POINT('',(-15.1423033840733,-0.0114224867028862,1.08333333333333));
#39875=CARTESIAN_POINT('Ctrl Pts',(-15.1423033840733,-0.0114224867028739,
-1.08333333333334));
#39876=CARTESIAN_POINT('Ctrl Pts',(-15.1423953499066,0.110492695607543,
-0.727666221822802));
#39877=CARTESIAN_POINT('Ctrl Pts',(-15.1413590080604,0.169498193350012,
-0.352782973842781));
#39878=CARTESIAN_POINT('Ctrl Pts',(-15.1413590080604,0.169498193350012,
-2.67362166230902E-15));
#39879=CARTESIAN_POINT('Ctrl Pts',(-15.1413590080604,0.169498193350012,
0.352782973842775));
#39880=CARTESIAN_POINT('Ctrl Pts',(-15.1423953499066,0.110492695607543,
0.727666221822795));
#39881=CARTESIAN_POINT('Ctrl Pts',(-15.1423033840733,-0.0114224867028737,
1.08333333333334));
#39882=CARTESIAN_POINT('',(-14.2484814298548,0.20803111085057,1.08333333333333));
#39883=CARTESIAN_POINT('Origin',(-13.892722748591,-3.17092330887754,1.08333333333333));
#39884=CARTESIAN_POINT('',(-14.2484814298548,0.208031110850571,-1.08333333333334));
#39885=CARTESIAN_POINT('Ctrl Pts',(-14.2484814298548,0.208031110850584,
1.08333333333333));
#39886=CARTESIAN_POINT('Ctrl Pts',(-14.2468058395578,0.322795758952019,
0.725928647976579));
#39887=CARTESIAN_POINT('Ctrl Pts',(-14.2449910310593,0.37779693624925,0.352039859176988));
#39888=CARTESIAN_POINT('Ctrl Pts',(-14.2449910310593,0.37779693624925,-2.46631154156404E-15));
#39889=CARTESIAN_POINT('Ctrl Pts',(-14.2449910310593,0.37779693624925,-0.352039859176994));
#39890=CARTESIAN_POINT('Ctrl Pts',(-14.2468058395578,0.322795758952019,
-0.725928647976587));
#39891=CARTESIAN_POINT('Ctrl Pts',(-14.2484814298548,0.208031110850583,
-1.08333333333334));
#39892=CARTESIAN_POINT('Origin',(-13.892722748591,-3.17092330887753,-1.08333333333334));
#39893=CARTESIAN_POINT('',(-12.7471768669563,-6.36961395396413,-1.08333333333334));
#39894=CARTESIAN_POINT('Origin',(-13.892722748591,-3.17092330887753,-1.08333333333334));
#39895=CARTESIAN_POINT('',(-12.7471768669563,-6.36961395396413,1.08333333333333));
#39896=CARTESIAN_POINT('Ctrl Pts',(-12.7471768669563,-6.36961395396412,
-1.08333333333334));
#39897=CARTESIAN_POINT('Ctrl Pts',(-12.6958726976266,-6.472286317656,-0.725928647976585));
#39898=CARTESIAN_POINT('Ctrl Pts',(-12.6703734952066,-6.52105325020167,
-0.352039859176994));
#39899=CARTESIAN_POINT('Ctrl Pts',(-12.6703734952066,-6.52105325020167,
0.352039859176985));
#39900=CARTESIAN_POINT('Ctrl Pts',(-12.6958726976266,-6.472286317656,0.725928647976577));
#39901=CARTESIAN_POINT('Ctrl Pts',(-12.7471768669563,-6.36961395396412,
1.08333333333333));
#39902=CARTESIAN_POINT('',(-13.6476999686241,-6.55970790622096,1.08333333333333));
#39903=CARTESIAN_POINT('Origin',(-13.892722748591,-3.17092330887754,1.08333333333333));
#39904=CARTESIAN_POINT('Ctrl Pts',(-13.6476999686241,-6.55970790622096,
1.08333333333332));
#39905=CARTESIAN_POINT('Ctrl Pts',(-13.5948858118208,-6.66958959248691,
0.727666221822788));
#39906=CARTESIAN_POINT('Ctrl Pts',(-13.5683505740919,-6.72230205711272,
0.35278297384277));
#39907=CARTESIAN_POINT('Ctrl Pts',(-13.5683505740919,-6.72230205711272,
-0.352782973842779));
#39908=CARTESIAN_POINT('Ctrl Pts',(-13.5948858118208,-6.66958959248691,
-0.727666221822796));
#39909=CARTESIAN_POINT('Ctrl Pts',(-13.6476999686241,-6.55970790622096,
-1.08333333333333));
#39910=CARTESIAN_POINT('',(-13.0227870731057,-2.97236616780882,3.45272288248773));
#39911=CARTESIAN_POINT('Origin',(-13.0227870731057,-2.97236616780882,-2.99978307628674E-15));
#39912=CARTESIAN_POINT('',(-14.7626584240763,-3.36948044994625,3.45272288248773));
#39913=CARTESIAN_POINT('Origin',(-14.7626584240763,-3.36948044994625,-3.40056031423578E-15));
#39914=CARTESIAN_POINT('Origin',(-6.18284328242512,-12.8388063676095,-4.97613300162231E-15));
#39915=CARTESIAN_POINT('',(-6.57000108040694,-13.6427478189686,-3.96060240207311));
#39916=CARTESIAN_POINT('Origin',(-6.57000108040694,-13.6427478189686,-5.28772891427451E-15));
#39917=CARTESIAN_POINT('',(-5.79568548444331,-12.0348649162504,-3.96060240207311));
#39918=CARTESIAN_POINT('Origin',(-6.18284328242512,-12.8388063676095,-2.51985201161581));
#39919=CARTESIAN_POINT('Origin',(-5.79568548444331,-12.0348649162504,-4.66453708897012E-15));
#39920=CARTESIAN_POINT('',(-2.35859284151935,-14.0534529496467,1.08333333333333));
#39921=CARTESIAN_POINT('',(-2.69569375163562,-14.9004267538186,1.08333333333333));
#39922=CARTESIAN_POINT('Ctrl Pts',(-2.35859284151934,-14.0534529496467,
1.08333333333333));
#39923=CARTESIAN_POINT('Ctrl Pts',(-2.37682723618162,-14.2398470420046,
1.08333333333333));
#39924=CARTESIAN_POINT('Ctrl Pts',(-2.43502529011671,-14.4435268961719,
1.08333333333332));
#39925=CARTESIAN_POINT('Ctrl Pts',(-2.56051322547963,-14.7041052789647,
1.08333333333333));
#39926=CARTESIAN_POINT('Ctrl Pts',(-2.62287825309305,-14.806702452812,1.08333333333333));
#39927=CARTESIAN_POINT('Ctrl Pts',(-2.69569375163558,-14.9004267538186,
1.08333333333333));
#39928=CARTESIAN_POINT('',(-2.35859284151935,-14.0534529496467,-1.08333333333334));
#39929=CARTESIAN_POINT('Ctrl Pts',(-2.35859284151935,-14.0534529496467,
1.08333333333333));
#39930=CARTESIAN_POINT('Ctrl Pts',(-2.32474809698527,-14.0591331175362,
0.949622058007895));
#39931=CARTESIAN_POINT('Ctrl Pts',(-2.29723964086638,-14.0636285445206,
0.814376693553736));
#39932=CARTESIAN_POINT('Ctrl Pts',(-2.27611794897253,-14.0670461391994,
0.678132403728853));
#39933=CARTESIAN_POINT('Ctrl Pts',(-2.25509664145098,-14.0704474911881,
0.542535637671543));
#39934=CARTESIAN_POINT('Ctrl Pts',(-2.24040145926613,-14.0727812605466,
0.405949418799629));
#39935=CARTESIAN_POINT('Ctrl Pts',(-2.23207311688321,-14.0741020886196,
0.268901316712528));
#39936=CARTESIAN_POINT('Ctrl Pts',(-2.22663511068775,-14.0749645256946,
0.179415511019263));
#39937=CARTESIAN_POINT('Ctrl Pts',(-2.2239114043034,-14.075394064317,0.0897327832369026));
#39938=CARTESIAN_POINT('Ctrl Pts',(-2.2239114043034,-14.075394064317,-8.43769498715119E-15));
#39939=CARTESIAN_POINT('Ctrl Pts',(-2.2239114043034,-14.075394064317,-0.137573936980349));
#39940=CARTESIAN_POINT('Ctrl Pts',(-2.23031275616482,-14.0743870796481,
-0.274951212619667));
#39941=CARTESIAN_POINT('Ctrl Pts',(-2.24306143269717,-14.0723550057958,
-0.411612406214657));
#39942=CARTESIAN_POINT('Ctrl Pts',(-2.25590874866049,-14.0703072093226,
-0.549330978772813));
#39943=CARTESIAN_POINT('Ctrl Pts',(-2.27520203478074,-14.0672183663696,
-0.68632234543694));
#39944=CARTESIAN_POINT('Ctrl Pts',(-2.30087730766032,-14.0630175856782,
-0.822054935347292));
#39945=CARTESIAN_POINT('Ctrl Pts',(-2.31746020132759,-14.0603044266067,
-0.909720570537337));
#39946=CARTESIAN_POINT('Ctrl Pts',(-2.33670515605249,-14.0571263627534,
-0.996861109122898));
#39947=CARTESIAN_POINT('Ctrl Pts',(-2.35859284151935,-14.0534529496467,
-1.08333333333334));
#39948=CARTESIAN_POINT('',(-2.69569375163563,-14.9004267538187,-1.08333333333334));
#39949=CARTESIAN_POINT('Ctrl Pts',(-2.35859284151934,-14.0534529496467,
-1.08333333333333));
#39950=CARTESIAN_POINT('Ctrl Pts',(-2.37688304383397,-14.2404175142851,
-1.08333333333333));
#39951=CARTESIAN_POINT('Ctrl Pts',(-2.43503901504648,-14.4435553962822,
-1.08333333333334));
#39952=CARTESIAN_POINT('Ctrl Pts',(-2.56054033827446,-14.7041615792632,
-1.08333333333334));
#39953=CARTESIAN_POINT('Ctrl Pts',(-2.62284674626764,-14.8066618988743,
-1.08333333333334));
#39954=CARTESIAN_POINT('Ctrl Pts',(-2.69569375163563,-14.9004267538187,
-1.08333333333334));
#39955=CARTESIAN_POINT('Ctrl Pts',(-2.69569375163559,-14.9004267538186,
-1.08333333333335));
#39956=CARTESIAN_POINT('Ctrl Pts',(-2.65857154890325,-14.9071426748862,
-0.955915065626573));
#39957=CARTESIAN_POINT('Ctrl Pts',(-2.628016775001,-14.9125315333598,-0.826701571450498));
#39958=CARTESIAN_POINT('Ctrl Pts',(-2.60415669762586,-14.9166970252376,
-0.696211209492072));
#39959=CARTESIAN_POINT('Ctrl Pts',(-2.58067270588166,-14.9207968600927,
-0.567777653525379));
#39960=CARTESIAN_POINT('Ctrl Pts',(-2.56367395385075,-14.923711651889,-0.438107164856101));
#39961=CARTESIAN_POINT('Ctrl Pts',(-2.55327224255806,-14.9254910506792,
-0.307693975181385));
#39962=CARTESIAN_POINT('Ctrl Pts',(-2.54512176981446,-14.9268853348437,
-0.205506064179128));
#39963=CARTESIAN_POINT('Ctrl Pts',(-2.54102158203148,-14.9275815713119,
-0.102862147740959));
#39964=CARTESIAN_POINT('Ctrl Pts',(-2.54102158203148,-14.9275815713119,
-4.44089209850063E-15));
#39965=CARTESIAN_POINT('Ctrl Pts',(-2.54102158203148,-14.9275815713119,
0.130666807305524));
#39966=CARTESIAN_POINT('Ctrl Pts',(-2.54764001565181,-14.9264594186595,
0.261069786498646));
#39967=CARTESIAN_POINT('Ctrl Pts',(-2.56079607270382,-14.9242020129234,
0.390710450870999));
#39968=CARTESIAN_POINT('Ctrl Pts',(-2.57411009834303,-14.9219175018628,
0.521907748246163));
#39969=CARTESIAN_POINT('Ctrl Pts',(-2.59411972995703,-14.9184702682937,
0.652324314224157));
#39970=CARTESIAN_POINT('Ctrl Pts',(-2.62073179377387,-14.9137938537994,
0.781443489202868));
#39971=CARTESIAN_POINT('Ctrl Pts',(-2.64165463403551,-14.9101171801624,
0.882959098491507));
#39972=CARTESIAN_POINT('Ctrl Pts',(-2.66665850662476,-14.9056796321318,
0.983672743459509));
#39973=CARTESIAN_POINT('Ctrl Pts',(-2.69569375163559,-14.9004267538186,
1.08333333333334));
#39974=CARTESIAN_POINT('',(-9.96888517526507,-11.3978423664701,1.08333333333333));
#39975=CARTESIAN_POINT('',(-9.516873369993,-10.6062067328295,1.08333333333333));
#39976=CARTESIAN_POINT('Ctrl Pts',(-9.96888517526507,-11.3978423664701,
1.08333333333333));
#39977=CARTESIAN_POINT('Ctrl Pts',(-9.94100828682427,-11.282476771434,1.08333333333333));
#39978=CARTESIAN_POINT('Ctrl Pts',(-9.89967854500783,-11.1697495378475,
1.08333333333333));
#39979=CARTESIAN_POINT('Ctrl Pts',(-9.77419060964491,-10.9091711550547,
1.08333333333333));
#39980=CARTESIAN_POINT('Ctrl Pts',(-9.65123318042897,-10.7366777723525,
1.08333333333333));
#39981=CARTESIAN_POINT('Ctrl Pts',(-9.51687336999256,-10.6062067328299,
1.08333333333333));
#39982=CARTESIAN_POINT('',(-9.96888517526507,-11.3978423664701,-1.08333333333334));
#39983=CARTESIAN_POINT('Ctrl Pts',(-9.96888517526508,-11.3978423664701,
1.08333333333333));
#39984=CARTESIAN_POINT('Ctrl Pts',(-9.99706424266063,-11.3731961327199,
0.956888632103256));
#39985=CARTESIAN_POINT('Ctrl Pts',(-10.020155672713,-11.3528209383891,0.828820583351071));
#39986=CARTESIAN_POINT('Ctrl Pts',(-10.038197564346,-11.3368457653652,0.699646919261599));
#39987=CARTESIAN_POINT('Ctrl Pts',(-10.0561445912219,-11.3209545902358,
0.571152453812953));
#39988=CARTESIAN_POINT('Ctrl Pts',(-10.0690951385517,-11.3094172714603,
0.441563969171296));
#39989=CARTESIAN_POINT('Ctrl Pts',(-10.0770534136919,-11.3023217413999,
0.311391073637437));
#39990=CARTESIAN_POINT('Ctrl Pts',(-10.0849478229272,-11.2952831536342,
0.182262827807044));
#39991=CARTESIAN_POINT('Ctrl Pts',(-10.0879298097314,-11.2926153440655,
0.0525595133516554));
#39992=CARTESIAN_POINT('Ctrl Pts',(-10.0859696068728,-11.2943658227348,
-0.0772214321950453));
#39993=CARTESIAN_POINT('Ctrl Pts',(-10.0846326712896,-11.2955597181575,
-0.165737150534751));
#39994=CARTESIAN_POINT('Ctrl Pts',(-10.0809960349672,-11.2988081152181,
-0.2542889811304));
#39995=CARTESIAN_POINT('Ctrl Pts',(-10.0750409796764,-11.304115688826,-0.342719102199531));
#39996=CARTESIAN_POINT('Ctrl Pts',(-10.0660632343107,-11.3121173012435,
-0.476034927301883));
#39997=CARTESIAN_POINT('Ctrl Pts',(-10.0518705086679,-11.3247537742305,
-0.608312350206005));
#39998=CARTESIAN_POINT('Ctrl Pts',(-10.0325330571073,-11.3418588735079,
-0.739057191238004));
#39999=CARTESIAN_POINT('Ctrl Pts',(-10.0153642561251,-11.3570456753652,
-0.855139299994515));
#40000=CARTESIAN_POINT('Ctrl Pts',(-9.99413932000721,-11.3757543553326,
-0.970013302477919));
#40001=CARTESIAN_POINT('Ctrl Pts',(-9.96888517526508,-11.3978423664701,
-1.08333333333334));
#40002=CARTESIAN_POINT('',(-9.51687336999906,-10.6062067328363,-1.08333333333334));
#40003=CARTESIAN_POINT('Ctrl Pts',(-9.96888517526507,-11.3978423664701,
-1.08333333333333));
#40004=CARTESIAN_POINT('Ctrl Pts',(-9.94100828682427,-11.282476771434,-1.08333333333333));
#40005=CARTESIAN_POINT('Ctrl Pts',(-9.89967854500783,-11.1697495378475,
-1.08333333333333));
#40006=CARTESIAN_POINT('Ctrl Pts',(-9.77419060964618,-10.9091711550573,
-1.08333333333333));
#40007=CARTESIAN_POINT('Ctrl Pts',(-9.6512331804331,-10.7366777723579,-1.08333333333333));
#40008=CARTESIAN_POINT('Ctrl Pts',(-9.51687336999908,-10.6062067328363,
-1.08333333333333));
#40009=CARTESIAN_POINT('Ctrl Pts',(-9.51687336999256,-10.6062067328299,
-1.08333333333319));
#40010=CARTESIAN_POINT('Ctrl Pts',(-9.54248335115827,-10.5832270800755,
-0.949270311030248));
#40011=CARTESIAN_POINT('Ctrl Pts',(-9.56321910180067,-10.5644593135702,
-0.813521288367661));
#40012=CARTESIAN_POINT('Ctrl Pts',(-9.57910097474595,-10.5500390764974,
-0.676607052100613));
#40013=CARTESIAN_POINT('Ctrl Pts',(-9.59267821366648,-10.5377113740467,
-0.559560573777554));
#40014=CARTESIAN_POINT('Ctrl Pts',(-9.6027075928823,-10.5285603838747,-0.44166251627891));
#40015=CARTESIAN_POINT('Ctrl Pts',(-9.6091818848891,-10.5226481221753,-0.323238258334718));
#40016=CARTESIAN_POINT('Ctrl Pts',(-9.61666296645239,-10.5158164698571,
-0.186398348762648));
#40017=CARTESIAN_POINT('Ctrl Pts',(-9.61937600851194,-10.5133302394117,
-0.0492519096262118));
#40018=CARTESIAN_POINT('Ctrl Pts',(-9.61735300288125,-10.5151805128572,
0.08767582706605));
#40019=CARTESIAN_POINT('Ctrl Pts',(-9.61532413250719,-10.5170361502911,
0.225000520654331));
#40020=CARTESIAN_POINT('Ctrl Pts',(-9.60853168799772,-10.5232534570122,
0.362105241912796));
#40021=CARTESIAN_POINT('Ctrl Pts',(-9.59697252030892,-10.5337846211338,
0.498460177595657));
#40022=CARTESIAN_POINT('Ctrl Pts',(-9.5853634847053,-10.5443612182148,0.635403368116659));
#40023=CARTESIAN_POINT('Ctrl Pts',(-9.56894645381043,-10.5592890006364,
0.771590289741169));
#40024=CARTESIAN_POINT('Ctrl Pts',(-9.54768316346852,-10.578480335569,0.906484242526434));
#40025=CARTESIAN_POINT('Ctrl Pts',(-9.53834928383367,-10.5869046954593,
0.965698216399696));
#40026=CARTESIAN_POINT('Ctrl Pts',(-9.52808112091929,-10.5961500981613,
1.02466304565381));
#40027=CARTESIAN_POINT('Ctrl Pts',(-9.51687336999256,-10.6062067328299,
1.08333333333318));
#40028=CARTESIAN_POINT('Origin',(-6.18284328242512,-12.8388063676095,-4.97613300162231E-15));
#40029=CARTESIAN_POINT('',(-3.38061559238688,-14.7601124814492,-1.08333333333334));
#40030=CARTESIAN_POINT('',(-3.12168342103518,-14.3129832609672,-1.08333333333334));
#40031=CARTESIAN_POINT('Origin',(-6.18284328242512,-12.8388063676095,-1.08333333333334));
#40032=CARTESIAN_POINT('',(-9.24400314381506,-11.3646294742518,-1.08333333333334));
#40033=CARTESIAN_POINT('Origin',(-6.18284328242512,-12.8388063676095,-4.97613300162231E-15));
#40034=CARTESIAN_POINT('',(-9.43214127690829,-11.8458513067218,-1.08333333333334));
#40035=CARTESIAN_POINT('Origin',(-6.18284328242512,-12.8388063676095,-1.08333333333334));
#40036=CARTESIAN_POINT('',(-9.43214127690829,-11.8458513067218,1.08333333333333));
#40037=CARTESIAN_POINT('Ctrl Pts',(-9.43214127690829,-11.8458513067218,
-1.08333333333333));
#40038=CARTESIAN_POINT('Ctrl Pts',(-9.52751574438859,-11.7699103356433,
-0.727666221822795));
#40039=CARTESIAN_POINT('Ctrl Pts',(-9.57300195158999,-11.7323107648653,
-0.352782973842778));
#40040=CARTESIAN_POINT('Ctrl Pts',(-9.57300195158999,-11.7323107648653,
-4.85994849902029E-15));
#40041=CARTESIAN_POINT('Ctrl Pts',(-9.57300195158999,-11.7323107648653,
0.352782973842767));
#40042=CARTESIAN_POINT('Ctrl Pts',(-9.52751574438859,-11.7699103356433,
0.727666221822782));
#40043=CARTESIAN_POINT('Ctrl Pts',(-9.43214127690829,-11.8458513067218,
1.08333333333332));
#40044=CARTESIAN_POINT('',(-9.04642813528379,-11.0102060831369,1.08333333333333));
#40045=CARTESIAN_POINT('Origin',(-6.18284328242512,-12.8388063676095,1.08333333333333));
#40046=CARTESIAN_POINT('',(-9.04642813528379,-11.0102060831369,-1.08333333333334));
#40047=CARTESIAN_POINT('Ctrl Pts',(-9.0464281352838,-11.0102060831369,1.08333333333332));
#40048=CARTESIAN_POINT('Ctrl Pts',(-9.13511003678158,-10.9373414661859,
0.725928647976571));
#40049=CARTESIAN_POINT('Ctrl Pts',(-9.17698017417422,-10.901629918632,0.352039859176983));
#40050=CARTESIAN_POINT('Ctrl Pts',(-9.17698017417422,-10.901629918632,-4.5383086406711E-15));
#40051=CARTESIAN_POINT('Ctrl Pts',(-9.17698017417422,-10.901629918632,-0.352039859176993));
#40052=CARTESIAN_POINT('Ctrl Pts',(-9.13511003678158,-10.9373414661859,
-0.725928647976581));
#40053=CARTESIAN_POINT('Ctrl Pts',(-9.0464281352838,-11.0102060831369,-1.08333333333333));
#40054=CARTESIAN_POINT('Origin',(-6.18284328242512,-12.8388063676095,-1.08333333333334));
#40055=CARTESIAN_POINT('',(-2.96777005865995,-13.9375335292483,-1.08333333333334));
#40056=CARTESIAN_POINT('Origin',(-6.18284328242512,-12.8388063676095,-1.08333333333334));
#40057=CARTESIAN_POINT('',(-2.96777005865995,-13.9375335292483,1.08333333333333));
#40058=CARTESIAN_POINT('Ctrl Pts',(-2.96777005865994,-13.9375335292483,
-1.08333333333334));
#40059=CARTESIAN_POINT('Ctrl Pts',(-2.85550994597631,-13.9614374861791,
-0.725928647976589));
#40060=CARTESIAN_POINT('Ctrl Pts',(-2.80148393014434,-13.9719070920595,
-0.352039859176996));
#40061=CARTESIAN_POINT('Ctrl Pts',(-2.80148393014434,-13.9719070920595,
0.352039859176986));
#40062=CARTESIAN_POINT('Ctrl Pts',(-2.85550994597631,-13.9614374861791,
0.725928647976578));
#40063=CARTESIAN_POINT('Ctrl Pts',(-2.96777005865994,-13.9375335292483,
1.08333333333333));
#40064=CARTESIAN_POINT('',(-3.38061559238688,-14.7601124814492,1.08333333333333));
#40065=CARTESIAN_POINT('Origin',(-6.18284328242512,-12.8388063676095,1.08333333333333));
#40066=CARTESIAN_POINT('Ctrl Pts',(-3.38061559238688,-14.7601124814492,
1.08333333333333));
#40067=CARTESIAN_POINT('Ctrl Pts',(-3.26177754255684,-14.7873308217382,
0.727666221822789));
#40068=CARTESIAN_POINT('Ctrl Pts',(-3.20402082808,-14.799450421612,0.35278297384277));
#40069=CARTESIAN_POINT('Ctrl Pts',(-3.20402082808,-14.799450421612,-0.352782973842781));
#40070=CARTESIAN_POINT('Ctrl Pts',(-3.26177754255684,-14.7873308217382,
-0.727666221822799));
#40071=CARTESIAN_POINT('Ctrl Pts',(-3.38061559238688,-14.7601124814492,
-1.08333333333334));
#40072=CARTESIAN_POINT('',(-5.79568548444331,-12.0348649162504,3.45272288248773));
#40073=CARTESIAN_POINT('Origin',(-5.79568548444331,-12.0348649162504,-4.66453708897012E-15));
#40074=CARTESIAN_POINT('',(-6.57000108040694,-13.6427478189686,3.45272288248772));
#40075=CARTESIAN_POINT('Origin',(-6.57000108040694,-13.6427478189686,-5.28772891427451E-15));
#40076=CARTESIAN_POINT('Origin',(6.1828432824253,-12.8388063676094,-4.9761330016223E-15));
#40077=CARTESIAN_POINT('',(6.57000108040713,-13.6427478189685,-3.96060240207311));
#40078=CARTESIAN_POINT('Origin',(6.57000108040713,-13.6427478189685,-5.28772891427449E-15));
#40079=CARTESIAN_POINT('',(5.79568548444348,-12.0348649162503,-3.96060240207311));
#40080=CARTESIAN_POINT('Origin',(6.1828432824253,-12.8388063676094,-2.51985201161581));
#40081=CARTESIAN_POINT('Origin',(5.79568548444348,-12.0348649162504,-4.66453708897011E-15));
#40082=CARTESIAN_POINT('',(9.51687336999268,-10.6062067328298,1.08333333333333));
#40083=CARTESIAN_POINT('',(9.96888517526453,-11.3978423664706,1.08333333333333));
#40084=CARTESIAN_POINT('Ctrl Pts',(9.5168733699927,-10.6062067328298,1.08333333333333));
#40085=CARTESIAN_POINT('Ctrl Pts',(9.65164439811578,-10.737077088181,1.08333333333333));
#40086=CARTESIAN_POINT('Ctrl Pts',(9.77420433457484,-10.9091996551649,1.08333333333333));
#40087=CARTESIAN_POINT('Ctrl Pts',(9.89970565780286,-11.169805838146,1.08333333333333));
#40088=CARTESIAN_POINT('Ctrl Pts',(9.94099622466366,-11.2824268534395,1.08333333333333));
#40089=CARTESIAN_POINT('Ctrl Pts',(9.96888517526534,-11.3978423664704,1.08333333333333));
#40090=CARTESIAN_POINT('',(9.51687336999268,-10.6062067328298,-1.08333333333334));
#40091=CARTESIAN_POINT('Ctrl Pts',(9.51687336999268,-10.6062067328298,1.08333333333333));
#40092=CARTESIAN_POINT('Ctrl Pts',(9.54241615713793,-10.5832873727889,0.949622058007762));
#40093=CARTESIAN_POINT('Ctrl Pts',(9.56308206533645,-10.5645832486408,0.814376693553466));
#40094=CARTESIAN_POINT('Ctrl Pts',(9.5789232079445,-10.5502004803844,0.678132403728444));
#40095=CARTESIAN_POINT('Ctrl Pts',(9.59468906287363,-10.5358860686389,0.542535637671145));
#40096=CARTESIAN_POINT('Ctrl Pts',(9.60567597345963,-10.5258519939611,0.405949418799242));
#40097=CARTESIAN_POINT('Ctrl Pts',(9.61190127497217,-10.5201641565229,0.268901316712153));
#40098=CARTESIAN_POINT('Ctrl Pts',(9.61596609683434,-10.5164502727984,0.179415511019018));
#40099=CARTESIAN_POINT('Ctrl Pts',(9.61800012680612,-10.5145886063487,0.0897327832367887));
#40100=CARTESIAN_POINT('Ctrl Pts',(9.61800012680612,-10.5145886063487,9.32587340685131E-15));
#40101=CARTESIAN_POINT('Ctrl Pts',(9.61800012680612,-10.5145886063487,-0.137573936980381));
#40102=CARTESIAN_POINT('Ctrl Pts',(9.61322165688595,-10.5189655400926,-0.274951212619743));
#40103=CARTESIAN_POINT('Ctrl Pts',(9.6036842477684,-10.5276658794419,-0.411612406214774));
#40104=CARTESIAN_POINT('Ctrl Pts',(9.59407304553156,-10.5364335353099,-0.54933097877281));
#40105=CARTESIAN_POINT('Ctrl Pts',(9.57962892372621,-10.5495917717182,-0.686322345436814));
#40106=CARTESIAN_POINT('Ctrl Pts',(9.5603363503304,-10.5670463644555,-0.822054935347047));
#40107=CARTESIAN_POINT('Ctrl Pts',(9.54787585206456,-10.5783197657831,-0.909720570537174));
#40108=CARTESIAN_POINT('Ctrl Pts',(9.5333921086825,-10.5913845868635,-0.996861109122817));
#40109=CARTESIAN_POINT('Ctrl Pts',(9.51687336999268,-10.6062067328298,-1.08333333333334));
#40110=CARTESIAN_POINT('',(9.9688851752657,-11.3978423664719,-1.08333333333334));
#40111=CARTESIAN_POINT('Ctrl Pts',(9.5168733699927,-10.6062067328298,-1.08333333333333));
#40112=CARTESIAN_POINT('Ctrl Pts',(9.65123318042911,-10.7366777723523,-1.08333333333333));
#40113=CARTESIAN_POINT('Ctrl Pts',(9.77419060964506,-10.9091711550545,-1.08333333333333));
#40114=CARTESIAN_POINT('Ctrl Pts',(9.89967854500826,-11.1697495378479,-1.08333333333333));
#40115=CARTESIAN_POINT('Ctrl Pts',(9.94100828682489,-11.2824767714351,-1.08333333333333));
#40116=CARTESIAN_POINT('Ctrl Pts',(9.96888517526571,-11.3978423664719,-1.08333333333333));
#40117=CARTESIAN_POINT('Ctrl Pts',(9.96888517526519,-11.39784236647,-1.08333333333359));
#40118=CARTESIAN_POINT('Ctrl Pts',(9.99728120861575,-11.3730063679711,-0.955915065626921));
#40119=CARTESIAN_POINT('Ctrl Pts',(10.0205449777511,-11.3524775820965,-0.826701571450959));
#40120=CARTESIAN_POINT('Ctrl Pts',(10.038678205356,-11.3364201641361,-0.696211209492648));
#40121=CARTESIAN_POINT('Ctrl Pts',(10.0565256146782,-11.3206158452779,-0.567777653525928));
#40122=CARTESIAN_POINT('Ctrl Pts',(10.0694030392049,-11.309143028737,-0.438107164856624));
#40123=CARTESIAN_POINT('Ctrl Pts',(10.0772795901119,-11.3021200803759,-0.307693975181881));
#40124=CARTESIAN_POINT('Ctrl Pts',(10.0834514220032,-11.2966171061454,-0.20550606417946));
#40125=CARTESIAN_POINT('Ctrl Pts',(10.0865521868617,-11.2938455465903,-0.102862147741125));
#40126=CARTESIAN_POINT('Ctrl Pts',(10.0865521868617,-11.2938455465903,-4.44089209850063E-15));
#40127=CARTESIAN_POINT('Ctrl Pts',(10.0865521868617,-11.2938455465903,0.130666807305562));
#40128=CARTESIAN_POINT('Ctrl Pts',(10.0815483267233,-11.2983203956244,0.261069786498721));
#40129=CARTESIAN_POINT('Ctrl Pts',(10.0715807484455,-11.3071987457576,0.390710450871112));
#40130=CARTESIAN_POINT('Ctrl Pts',(10.0614934865685,-11.3161837008123,0.521907748246463));
#40131=CARTESIAN_POINT('Ctrl Pts',(10.0463225295865,-11.3296785457857,0.652324314224642));
#40132=CARTESIAN_POINT('Ctrl Pts',(10.0260740111135,-11.3475689983448,0.781443489203535));
#40133=CARTESIAN_POINT('Ctrl Pts',(10.0101542943843,-11.3616347650465,0.88295909849203));
#40134=CARTESIAN_POINT('Ctrl Pts',(9.99109522006272,-11.3784168138781,0.983672743459888));
#40135=CARTESIAN_POINT('Ctrl Pts',(9.96888517526519,-11.39784236647,1.08333333333358));
#40136=CARTESIAN_POINT('',(2.69569375163578,-14.9004267538186,1.08333333333333));
#40137=CARTESIAN_POINT('',(2.35859284151893,-14.0534529496468,1.08333333333333));
#40138=CARTESIAN_POINT('Ctrl Pts',(2.6956937516358,-14.9004267538186,1.08333333333332));
#40139=CARTESIAN_POINT('Ctrl Pts',(2.62284674626782,-14.8066618988742,1.08333333333332));
#40140=CARTESIAN_POINT('Ctrl Pts',(2.56054033827465,-14.7041615792632,1.08333333333332));
#40141=CARTESIAN_POINT('Ctrl Pts',(2.4350390150467,-14.4435553962822,1.08333333333332));
#40142=CARTESIAN_POINT('Ctrl Pts',(2.37688304383419,-14.2404175142851,1.08333333333332));
#40143=CARTESIAN_POINT('Ctrl Pts',(2.35859284151955,-14.0534529496467,1.08333333333332));
#40144=CARTESIAN_POINT('',(2.69569375163578,-14.9004267538186,-1.08333333333334));
#40145=CARTESIAN_POINT('Ctrl Pts',(2.69569375163578,-14.9004267538186,1.08333333333333));
#40146=CARTESIAN_POINT('Ctrl Pts',(2.65885518901859,-14.9070913604575,0.956888632103347));
#40147=CARTESIAN_POINT('Ctrl Pts',(2.62852794948137,-14.9124412415715,0.828820583351256));
#40148=CARTESIAN_POINT('Ctrl Pts',(2.60478912083403,-14.9165866029902,0.699646919261879));
#40149=CARTESIAN_POINT('Ctrl Pts',(2.58117511159368,-14.9207101679857,0.571152453813268));
#40150=CARTESIAN_POINT('Ctrl Pts',(2.56408033836306,-14.9236419130061,0.441563969171648));
#40151=CARTESIAN_POINT('Ctrl Pts',(2.55357092618676,-14.9254399524253,0.311391073637824));
#40152=CARTESIAN_POINT('Ctrl Pts',(2.54314585302948,-14.9272235624095,0.182262827807427));
#40153=CARTESIAN_POINT('Ctrl Pts',(2.53920083715778,-14.927891621514,0.0525595133520343));
#40154=CARTESIAN_POINT('Ctrl Pts',(2.54179158298272,-14.9274504788058,-0.077221432194672));
#40155=CARTESIAN_POINT('Ctrl Pts',(2.54355857371286,-14.9271496020974,-0.165737150534507));
#40156=CARTESIAN_POINT('Ctrl Pts',(2.54836567846244,-14.9263317077699,-0.254288981130285));
#40157=CARTESIAN_POINT('Ctrl Pts',(2.55622822284789,-14.9249850760809,-0.342719102199546));
#40158=CARTESIAN_POINT('Ctrl Pts',(2.56808166802554,-14.9229549158531,-0.47603492730158));
#40159=CARTESIAN_POINT('Ctrl Pts',(2.58681028013297,-14.9197373081624,-0.608312350205393));
#40160=CARTESIAN_POINT('Ctrl Pts',(2.61224028910069,-14.9152835347009,-0.739057191237091));
#40161=CARTESIAN_POINT('Ctrl Pts',(2.63481838123332,-14.9113292416576,-0.855139299993913));
#40162=CARTESIAN_POINT('Ctrl Pts',(2.66267894744191,-14.9063995895532,-0.970013302477622));
#40163=CARTESIAN_POINT('Ctrl Pts',(2.69569375163578,-14.9004267538186,-1.08333333333334));
#40164=CARTESIAN_POINT('',(2.35859284152043,-14.0534529496557,-1.08333333333334));
#40165=CARTESIAN_POINT('Ctrl Pts',(2.6956937516358,-14.9004267538186,-1.08333333333334));
#40166=CARTESIAN_POINT('Ctrl Pts',(2.62284674626782,-14.8066618988742,-1.08333333333334));
#40167=CARTESIAN_POINT('Ctrl Pts',(2.56054033827465,-14.7041615792632,-1.08333333333334));
#40168=CARTESIAN_POINT('Ctrl Pts',(2.43503901504795,-14.4435553962848,-1.08333333333334));
#40169=CARTESIAN_POINT('Ctrl Pts',(2.37688304383586,-14.2404175142916,-1.08333333333334));
#40170=CARTESIAN_POINT('Ctrl Pts',(2.35859284152042,-14.0534529496557,-1.08333333333334));
#40171=CARTESIAN_POINT('Ctrl Pts',(2.35859284151951,-14.0534529496467,-1.08333333333319));
#40172=CARTESIAN_POINT('Ctrl Pts',(2.32465906345733,-14.0591480600448,-0.949270311030372));
#40173=CARTESIAN_POINT('Ctrl Pts',(2.29705730368849,-14.0636584116899,-0.813521288367913));
#40174=CARTESIAN_POINT('Ctrl Pts',(2.27588092254449,-14.0670844892038,-0.676607052100994));
#40175=CARTESIAN_POINT('Ctrl Pts',(2.25777746665768,-14.0700134052785,-0.55956057377781));
#40176=CARTESIAN_POINT('Ctrl Pts',(2.24436971878542,-14.0721491406499,-0.441662516279038));
#40177=CARTESIAN_POINT('Ctrl Pts',(2.23571067141573,-14.073524711092,-0.323238258334718));
#40178=CARTESIAN_POINT('Ctrl Pts',(2.2257050924945,-14.0751141906309,-0.186398348762649));
#40179=CARTESIAN_POINT('Ctrl Pts',(2.22206972520347,-14.0756851929985,-0.0492519096262131));
#40180=CARTESIAN_POINT('Ctrl Pts',(2.22477765061414,-14.0752571701311,0.087675827066048));
#40181=CARTESIAN_POINT('Ctrl Pts',(2.22749342636756,-14.0748279064149,0.225000520654297));
#40182=CARTESIAN_POINT('Ctrl Pts',(2.23658933237962,-14.0733937867901,0.362105241912729));
#40183=CARTESIAN_POINT('Ctrl Pts',(2.25202995120888,-14.0709225390114,0.498460177595558));
#40184=CARTESIAN_POINT('Ctrl Pts',(2.26753718309241,-14.0684406299137,0.635403368116538));
#40185=CARTESIAN_POINT('Ctrl Pts',(2.28944404469282,-14.0649125984157,0.771590289741026));
#40186=CARTESIAN_POINT('Ctrl Pts',(2.31770587921582,-14.0602538902201,0.906484242526269));
#40187=CARTESIAN_POINT('Ctrl Pts',(2.33011188776182,-14.0582088717468,0.965698216399587));
#40188=CARTESIAN_POINT('Ctrl Pts',(2.34374232952329,-14.0559453130119,1.02466304565376));
#40189=CARTESIAN_POINT('Ctrl Pts',(2.35859284151951,-14.0534529496467,1.08333333333318));
#40190=CARTESIAN_POINT('Origin',(6.1828432824253,-12.8388063676094,-4.9761330016223E-15));
#40191=CARTESIAN_POINT('',(9.43214127690845,-11.8458513067217,-1.08333333333334));
#40192=CARTESIAN_POINT('',(9.24400314381522,-11.3646294742516,-1.08333333333334));
#40193=CARTESIAN_POINT('Origin',(6.1828432824253,-12.8388063676094,-1.08333333333334));
#40194=CARTESIAN_POINT('',(3.12168342103538,-14.3129832609672,-1.08333333333334));
#40195=CARTESIAN_POINT('Origin',(6.1828432824253,-12.8388063676094,-4.9761330016223E-15));
#40196=CARTESIAN_POINT('',(3.38061559238708,-14.7601124814491,-1.08333333333334));
#40197=CARTESIAN_POINT('Origin',(6.1828432824253,-12.8388063676094,-1.08333333333334));
#40198=CARTESIAN_POINT('',(3.38061559238708,-14.7601124814491,1.08333333333333));
#40199=CARTESIAN_POINT('Ctrl Pts',(3.3806155923871,-14.7601124814491,-1.08333333333334));
#40200=CARTESIAN_POINT('Ctrl Pts',(3.26177754255705,-14.7873308217381,-0.7276662218228));
#40201=CARTESIAN_POINT('Ctrl Pts',(3.20402082808022,-14.7994504216119,-0.35278297384278));
#40202=CARTESIAN_POINT('Ctrl Pts',(3.20402082808022,-14.7994504216119,-5.42337291349619E-15));
#40203=CARTESIAN_POINT('Ctrl Pts',(3.20402082808022,-14.7994504216119,0.352782973842771));
#40204=CARTESIAN_POINT('Ctrl Pts',(3.26177754255705,-14.7873308217381,0.727666221822789));
#40205=CARTESIAN_POINT('Ctrl Pts',(3.3806155923871,-14.7601124814491,1.08333333333333));
#40206=CARTESIAN_POINT('',(2.96777005866014,-13.9375335292483,1.08333333333333));
#40207=CARTESIAN_POINT('Origin',(6.1828432824253,-12.8388063676094,1.08333333333333));
#40208=CARTESIAN_POINT('',(2.96777005866014,-13.9375335292483,-1.08333333333334));
#40209=CARTESIAN_POINT('Ctrl Pts',(2.96777005866014,-13.9375335292483,1.08333333333333));
#40210=CARTESIAN_POINT('Ctrl Pts',(2.85550994597651,-13.9614374861791,0.725928647976575));
#40211=CARTESIAN_POINT('Ctrl Pts',(2.80148393014454,-13.9719070920595,0.352039859176984));
#40212=CARTESIAN_POINT('Ctrl Pts',(2.80148393014454,-13.9719070920595,-5.10230940761107E-15));
#40213=CARTESIAN_POINT('Ctrl Pts',(2.80148393014454,-13.9719070920595,-0.352039859176994));
#40214=CARTESIAN_POINT('Ctrl Pts',(2.85550994597651,-13.9614374861791,-0.725928647976584));
#40215=CARTESIAN_POINT('Ctrl Pts',(2.96777005866014,-13.9375335292483,-1.08333333333334));
#40216=CARTESIAN_POINT('Origin',(6.1828432824253,-12.8388063676094,-1.08333333333334));
#40217=CARTESIAN_POINT('',(9.04642813528394,-11.0102060831368,-1.08333333333334));
#40218=CARTESIAN_POINT('Origin',(6.1828432824253,-12.8388063676094,-1.08333333333334));
#40219=CARTESIAN_POINT('',(9.04642813528394,-11.0102060831368,1.08333333333333));
#40220=CARTESIAN_POINT('Ctrl Pts',(9.04642813528395,-11.0102060831368,-1.08333333333334));
#40221=CARTESIAN_POINT('Ctrl Pts',(9.13511003678174,-10.9373414661857,-0.725928647976586));
#40222=CARTESIAN_POINT('Ctrl Pts',(9.17698017417438,-10.9016299186319,-0.352039859176995));
#40223=CARTESIAN_POINT('Ctrl Pts',(9.17698017417438,-10.9016299186319,0.352039859176985));
#40224=CARTESIAN_POINT('Ctrl Pts',(9.13511003678174,-10.9373414661857,0.725928647976577));
#40225=CARTESIAN_POINT('Ctrl Pts',(9.04642813528396,-11.0102060831368,1.08333333333333));
#40226=CARTESIAN_POINT('',(9.43214127690845,-11.8458513067217,1.08333333333333));
#40227=CARTESIAN_POINT('Origin',(6.1828432824253,-12.8388063676094,1.08333333333333));
#40228=CARTESIAN_POINT('Ctrl Pts',(9.43214127690846,-11.8458513067217,1.08333333333333));
#40229=CARTESIAN_POINT('Ctrl Pts',(9.52751574438876,-11.7699103356432,0.727666221822791));
#40230=CARTESIAN_POINT('Ctrl Pts',(9.57300195159016,-11.7323107648652,0.352782973842771));
#40231=CARTESIAN_POINT('Ctrl Pts',(9.57300195159016,-11.7323107648652,-0.352782973842781));
#40232=CARTESIAN_POINT('Ctrl Pts',(9.52751574438875,-11.7699103356432,-0.7276662218228));
#40233=CARTESIAN_POINT('Ctrl Pts',(9.43214127690846,-11.8458513067217,-1.08333333333334));
#40234=CARTESIAN_POINT('',(5.79568548444348,-12.0348649162504,3.45272288248773));
#40235=CARTESIAN_POINT('Origin',(5.79568548444348,-12.0348649162504,-4.66453708897011E-15));
#40236=CARTESIAN_POINT('',(6.57000108040713,-13.6427478189685,3.45272288248772));
#40237=CARTESIAN_POINT('Origin',(6.57000108040713,-13.6427478189685,-5.28772891427449E-15));
#40238=CARTESIAN_POINT('Origin',(13.892722748591,-3.17092330887735,-3.20017169526122E-15));
#40239=CARTESIAN_POINT('',(14.7626584240763,-3.36948044994605,-3.96060240207311));
#40240=CARTESIAN_POINT('Origin',(14.7626584240763,-3.36948044994605,-3.40056031423575E-15));
#40241=CARTESIAN_POINT('',(13.0227870731057,-2.97236616780864,-3.96060240207311));
#40242=CARTESIAN_POINT('Origin',(13.892722748591,-3.17092330887735,-2.5198520116158));
#40243=CARTESIAN_POINT('Origin',(13.0227870731057,-2.97236616780865,-2.9997830762867E-15));
#40244=CARTESIAN_POINT('',(14.2259398250621,0.827729480997053,1.08333333333333));
#40245=CARTESIAN_POINT('',(15.1266902369927,0.68754979644376,1.08333333333333));
#40246=CARTESIAN_POINT('Ctrl Pts',(14.2259398250621,0.827729480997104,1.08333333333333));
#40247=CARTESIAN_POINT('Ctrl Pts',(14.4122867506183,0.85150138178118,1.08333333333333));
#40248=CARTESIAN_POINT('Ctrl Pts',(14.6232724628281,0.840005933409976,1.08333333333333));
#40249=CARTESIAN_POINT('Ctrl Pts',(14.9052713763609,0.775641521611009,1.08333333333333));
#40250=CARTESIAN_POINT('Ctrl Pts',(15.0190662790554,0.737705732201359,1.08333333333333));
#40251=CARTESIAN_POINT('Ctrl Pts',(15.1266902369927,0.687549796443767,1.08333333333333));
#40252=CARTESIAN_POINT('',(14.2259398250621,0.827729480997055,-1.08333333333334));
#40253=CARTESIAN_POINT('Ctrl Pts',(14.2259398250621,0.8277294809971,1.08333333333334));
#40254=CARTESIAN_POINT('Ctrl Pts',(14.2239464151202,0.861989623387911,0.949622058007612));
#40255=CARTESIAN_POINT('Ctrl Pts',(14.2222079250172,0.889808711690379,0.814376693553152));
#40256=CARTESIAN_POINT('Ctrl Pts',(14.2208398148552,0.911161325030034,0.678132403727965));
#40257=CARTESIAN_POINT('Ctrl Pts',(14.2194782068654,0.932412456504566,0.542535637670654));
#40258=CARTESIAN_POINT('Ctrl Pts',(14.2184834780892,0.947258512328438,0.40594941879874));
#40259=CARTESIAN_POINT('Ctrl Pts',(14.2179179597194,0.955671957676133,0.268901316711642));
#40260=CARTESIAN_POINT('Ctrl Pts',(14.2175487034788,0.961165532006069,0.179415511018676));
#40261=CARTESIAN_POINT('Ctrl Pts',(14.2173613909827,0.963916530720146,0.0897327832366183));
#40262=CARTESIAN_POINT('Ctrl Pts',(14.2173613909827,0.963916530720146,1.06581410364015E-14));
#40263=CARTESIAN_POINT('Ctrl Pts',(14.2173613909827,0.963916530720146,-0.13757393698032));
#40264=CARTESIAN_POINT('Ctrl Pts',(14.2178040883167,0.957451598945758,-0.274951212619625));
#40265=CARTESIAN_POINT('Ctrl Pts',(14.2186598102071,0.944570379379524,-0.411612406214599));
#40266=CARTESIAN_POINT('Ctrl Pts',(14.2195221530139,0.931589494866494,-0.549330978772693));
#40267=CARTESIAN_POINT('Ctrl Pts',(14.2208039138492,0.912092599491427,-0.686322345436757));
#40268=CARTESIAN_POINT('Ctrl Pts',(14.222421741201,0.886126297665472,-0.822054935347047));
#40269=CARTESIAN_POINT('Ctrl Pts',(14.2234666476786,0.869355437073955,-0.909720570537178));
#40270=CARTESIAN_POINT('Ctrl Pts',(14.2246506698206,0.849885807807131,-0.996861109122824));
#40271=CARTESIAN_POINT('Ctrl Pts',(14.2259398250621,0.827729480997101,-1.08333333333335));
#40272=CARTESIAN_POINT('',(15.1266902369927,0.687549796443762,-1.08333333333334));
#40273=CARTESIAN_POINT('Ctrl Pts',(14.2259398250621,0.827729480997104,-1.08333333333333));
#40274=CARTESIAN_POINT('Ctrl Pts',(14.4122867506183,0.85150138178118,-1.08333333333333));
#40275=CARTESIAN_POINT('Ctrl Pts',(14.6232724628281,0.840005933409977,-1.08333333333333));
#40276=CARTESIAN_POINT('Ctrl Pts',(14.9052713763609,0.775641521611009,-1.08333333333333));
#40277=CARTESIAN_POINT('Ctrl Pts',(15.0190662790554,0.73770573220136,-1.08333333333333));
#40278=CARTESIAN_POINT('Ctrl Pts',(15.1266902369927,0.687549796443768,-1.08333333333333));
#40279=CARTESIAN_POINT('Ctrl Pts',(15.1266902369927,0.687549796443768,-1.08333333333334));
#40280=CARTESIAN_POINT('Ctrl Pts',(15.1249773086751,0.725235701077452,-0.955915065626868));
#40281=CARTESIAN_POINT('Ctrl Pts',(15.1234319803901,0.756223536825589,-0.826701571451108));
#40282=CARTESIAN_POINT('Ctrl Pts',(15.122183667988,0.780412301388443,-0.696211209493001));
#40283=CARTESIAN_POINT('Ctrl Pts',(15.1209550316477,0.804219799510377,-0.567777653526322));
#40284=CARTESIAN_POINT('Ctrl Pts',(15.12001416535,0.821440959530357,-0.43810716485706));
#40285=CARTESIAN_POINT('Ctrl Pts',(15.1194343523859,0.831977831684773,-0.307693975182356));
#40286=CARTESIAN_POINT('Ctrl Pts',(15.1189800281283,0.840234212474528,-0.205506064179778));
#40287=CARTESIAN_POINT('Ctrl Pts',(15.1187464308798,0.844386527178536,-0.102862147741283));
#40288=CARTESIAN_POINT('Ctrl Pts',(15.1187464308798,0.844386527178536,-1.99840144432528E-15));
#40289=CARTESIAN_POINT('Ctrl Pts',(15.1187464308798,0.844386527178536,0.130666807305585));
#40290=CARTESIAN_POINT('Ctrl Pts',(15.1191251529677,0.837684329050871,0.261069786498764));
#40291=CARTESIAN_POINT('Ctrl Pts',(15.1198518432089,0.824355801783881,0.390710450871172));
#40292=CARTESIAN_POINT('Ctrl Pts',(15.1205872590302,0.810867235029882,0.521907748246314));
#40293=CARTESIAN_POINT('Ctrl Pts',(15.1216790167187,0.790592205023559,0.652324314224285));
#40294=CARTESIAN_POINT('Ctrl Pts',(15.1230415909943,0.763606761086929,0.781443489202972));
#40295=CARTESIAN_POINT('Ctrl Pts',(15.1241128691977,0.742390363262186,0.882959098491574));
#40296=CARTESIAN_POINT('Ctrl Pts',(15.1253504648421,0.717025942630064,0.983672743459537));
#40297=CARTESIAN_POINT('Ctrl Pts',(15.1266902369927,0.687549796443768,1.08333333333333));
#40298=CARTESIAN_POINT('',(13.3303603014235,-7.18268588222768,1.08333333333333));
#40299=CARTESIAN_POINT('',(12.4579905368411,-6.91816245718305,1.08333333333333));
#40300=CARTESIAN_POINT('Ctrl Pts',(13.3303603014235,-7.18268588222769,1.08333333333333));
#40301=CARTESIAN_POINT('Ctrl Pts',(13.2116326209361,-7.18117853359731,1.08333333333333));
#40302=CARTESIAN_POINT('Ctrl Pts',(13.0926472341269,-7.16598374096113,1.08333333333333));
#40303=CARTESIAN_POINT('Ctrl Pts',(12.8106483205942,-7.10161932916216,1.08333333333333));
#40304=CARTESIAN_POINT('Ctrl Pts',(12.6155690741987,-7.02043310055321,1.08333333333333));
#40305=CARTESIAN_POINT('Ctrl Pts',(12.4579905368414,-6.91816245718254,1.08333333333333));
#40306=CARTESIAN_POINT('',(13.3303603014235,-7.18268588222768,-1.08333333333334));
#40307=CARTESIAN_POINT('Ctrl Pts',(13.3303603014235,-7.18268588222769,1.08333333333333));
#40308=CARTESIAN_POINT('Ctrl Pts',(13.3126024326051,-7.21564274452345,0.956888632103319));
#40309=CARTESIAN_POINT('Ctrl Pts',(13.2978764135175,-7.24268913148574,0.828820583351199));
#40310=CARTESIAN_POINT('Ctrl Pts',(13.2863164700112,-7.26383348564869,0.699646919261793));
#40311=CARTESIAN_POINT('Ctrl Pts',(13.2748173090023,-7.28486666222208,0.57115245381317));
#40312=CARTESIAN_POINT('Ctrl Pts',(13.2664510227834,-7.30005980724128,0.441563969171537));
#40313=CARTESIAN_POINT('Ctrl Pts',(13.2613042752927,-7.30939745578421,0.311391073637702));
#40314=CARTESIAN_POINT('Ctrl Pts',(13.2561988309336,-7.31866016882124,0.182262827807302));
#40315=CARTESIAN_POINT('Ctrl Pts',(13.2542614634095,-7.32216103446727,0.0525595133519065));
#40316=CARTESIAN_POINT('Ctrl Pts',(13.2555318677529,-7.3198604598385,-0.0772214321948015));
#40317=CARTESIAN_POINT('Ctrl Pts',(13.2563983335702,-7.31829137729713,-0.16573715053459));
#40318=CARTESIAN_POINT('Ctrl Pts',(13.2587560588235,-7.31402308269219,-0.254288981130321));
#40319=CARTESIAN_POINT('Ctrl Pts',(13.2626054360147,-7.30703628683439,-0.342719102199534));
#40320=CARTESIAN_POINT('Ctrl Pts',(13.2684086950193,-7.29650310602066,-0.476034927301568));
#40321=CARTESIAN_POINT('Ctrl Pts',(13.2775701666805,-7.2798543418706,-0.608312350205377));
#40322=CARTESIAN_POINT('Ctrl Pts',(13.289943417625,-7.25719547792716,-0.739057191237071));
#40323=CARTESIAN_POINT('Ctrl Pts',(13.300929037023,-7.23707775329776,-0.8551392999939));
#40324=CARTESIAN_POINT('Ctrl Pts',(13.3144456587152,-7.21222189770271,-0.970013302477615));
#40325=CARTESIAN_POINT('Ctrl Pts',(13.3303603014235,-7.18268588222769,-1.08333333333334));
#40326=CARTESIAN_POINT('',(12.4579905368491,-6.91816245718746,-1.08333333333334));
#40327=CARTESIAN_POINT('Ctrl Pts',(13.3303603014235,-7.18268588222769,-1.08333333333333));
#40328=CARTESIAN_POINT('Ctrl Pts',(13.2116326209361,-7.18117853359731,-1.08333333333333));
#40329=CARTESIAN_POINT('Ctrl Pts',(13.0926472341269,-7.16598374096113,-1.08333333333333));
#40330=CARTESIAN_POINT('Ctrl Pts',(12.810648320597,-7.10161932916281,-1.08333333333333));
#40331=CARTESIAN_POINT('Ctrl Pts',(12.6155690742049,-7.020433100556,-1.08333333333333));
#40332=CARTESIAN_POINT('Ctrl Pts',(12.4579905368491,-6.91816245718749,-1.08333333333333));
#40333=CARTESIAN_POINT('Ctrl Pts',(12.4579905368414,-6.91816245718254,-1.08333333333318));
#40334=CARTESIAN_POINT('Ctrl Pts',(12.4412857888865,-6.94824379644432,-0.949270311030419));
#40335=CARTESIAN_POINT('Ctrl Pts',(12.4276027080704,-6.97263587945666,-0.813521288368017));
#40336=CARTESIAN_POINT('Ctrl Pts',(12.4170780656486,-6.99132836531005,-0.676607052101155));
#40337=CARTESIAN_POINT('Ctrl Pts',(12.4080806643215,-7.00730836636693,-0.559560573777918));
#40338=CARTESIAN_POINT('Ctrl Pts',(12.4013908554088,-7.019122574986,-0.441662516279092));
#40339=CARTESIAN_POINT('Ctrl Pts',(12.397067491958,-7.0267501449702,-0.323238258334718));
#40340=CARTESIAN_POINT('Ctrl Pts',(12.3920718206831,-7.03556384585387,-0.186398348762654));
#40341=CARTESIAN_POINT('Ctrl Pts',(12.3902516338787,-7.03876210460539,-0.0492519096262223));
#40342=CARTESIAN_POINT('Ctrl Pts',(12.3916053560035,-7.03637809537437,0.0876758270660355));
#40343=CARTESIAN_POINT('Ctrl Pts',(12.3929630026023,-7.03398717484161,0.225000520654302));
#40344=CARTESIAN_POINT('Ctrl Pts',(12.3975129673672,-7.02598155019911,0.362105241912753));
#40345=CARTESIAN_POINT('Ctrl Pts',(12.4052079364272,-7.01236879050172,0.498460177595601));
#40346=CARTESIAN_POINT('Ctrl Pts',(12.4129361026925,-6.99869730339771,0.635403368116608));
#40347=CARTESIAN_POINT('Ctrl Pts',(12.4238364813948,-6.9793701376568,0.771590289741124));
#40348=CARTESIAN_POINT('Ctrl Pts',(12.4378151222668,-6.95436948862457,0.906484242526394));
#40349=CARTESIAN_POINT('Ctrl Pts',(12.4439512822523,-6.94339503240884,0.96569821639967));
#40350=CARTESIAN_POINT('Ctrl Pts',(12.4506800022041,-6.93132701813272,1.0246630456538));
#40351=CARTESIAN_POINT('Ctrl Pts',(12.4579905368414,-6.91816245718254,1.08333333333318));
#40352=CARTESIAN_POINT('Origin',(13.892722748591,-3.17092330887735,-3.20017169526122E-15));
#40353=CARTESIAN_POINT('',(15.1423033840733,-0.0114224867026808,-1.08333333333334));
#40354=CARTESIAN_POINT('',(14.6487667980729,0.141522102769127,-1.08333333333334));
#40355=CARTESIAN_POINT('Origin',(13.892722748591,-3.17092330887735,-1.08333333333334));
#40356=CARTESIAN_POINT('',(13.1366786991091,-6.48336872052383,-1.08333333333334));
#40357=CARTESIAN_POINT('Origin',(13.892722748591,-3.17092330887735,-3.20017169526122E-15));
#40358=CARTESIAN_POINT('',(13.6476999686242,-6.55970790622078,-1.08333333333334));
#40359=CARTESIAN_POINT('Origin',(13.892722748591,-3.17092330887735,-1.08333333333334));
#40360=CARTESIAN_POINT('',(13.6476999686242,-6.55970790622078,1.08333333333333));
#40361=CARTESIAN_POINT('Ctrl Pts',(13.6476999686242,-6.55970790622078,-1.08333333333334));
#40362=CARTESIAN_POINT('Ctrl Pts',(13.5948858118209,-6.66958959248674,-0.727666221822799));
#40363=CARTESIAN_POINT('Ctrl Pts',(13.5683505740919,-6.72230205711255,-0.35278297384278));
#40364=CARTESIAN_POINT('Ctrl Pts',(13.5683505740919,-6.72230205711255,-3.93962482987281E-15));
#40365=CARTESIAN_POINT('Ctrl Pts',(13.5683505740919,-6.72230205711255,0.352782973842772));
#40366=CARTESIAN_POINT('Ctrl Pts',(13.5948858118209,-6.66958959248674,0.727666221822791));
#40367=CARTESIAN_POINT('Ctrl Pts',(13.6476999686242,-6.55970790622078,1.08333333333333));
#40368=CARTESIAN_POINT('',(12.7471768669564,-6.36961395396396,1.08333333333333));
#40369=CARTESIAN_POINT('Origin',(13.892722748591,-3.17092330887735,1.08333333333333));
#40370=CARTESIAN_POINT('',(12.7471768669564,-6.36961395396396,-1.08333333333334));
#40371=CARTESIAN_POINT('Ctrl Pts',(12.7471768669564,-6.36961395396397,1.08333333333334));
#40372=CARTESIAN_POINT('Ctrl Pts',(12.6958726976266,-6.47228631765585,0.725928647976583));
#40373=CARTESIAN_POINT('Ctrl Pts',(12.6703734952067,-6.52105325020152,0.352039859176988));
#40374=CARTESIAN_POINT('Ctrl Pts',(12.6703734952067,-6.52105325020152,-3.73360976135914E-15));
#40375=CARTESIAN_POINT('Ctrl Pts',(12.6703734952067,-6.52105325020152,-0.352039859176996));
#40376=CARTESIAN_POINT('Ctrl Pts',(12.6958726976266,-6.47228631765585,-0.72592864797659));
#40377=CARTESIAN_POINT('Ctrl Pts',(12.7471768669564,-6.36961395396397,-1.08333333333335));
#40378=CARTESIAN_POINT('Origin',(13.892722748591,-3.17092330887735,-1.08333333333334));
#40379=CARTESIAN_POINT('',(14.2484814298548,0.208031110850763,-1.08333333333334));
#40380=CARTESIAN_POINT('Origin',(13.892722748591,-3.17092330887735,-1.08333333333334));
#40381=CARTESIAN_POINT('',(14.2484814298548,0.208031110850763,1.08333333333333));
#40382=CARTESIAN_POINT('Ctrl Pts',(14.2484814298548,0.208031110850765,-1.08333333333334));
#40383=CARTESIAN_POINT('Ctrl Pts',(14.2468058395578,0.322795758952199,-0.725928647976584));
#40384=CARTESIAN_POINT('Ctrl Pts',(14.2449910310593,0.377796936249431,-0.352039859176992));
#40385=CARTESIAN_POINT('Ctrl Pts',(14.2449910310593,0.37779693624943,0.352039859176986));
#40386=CARTESIAN_POINT('Ctrl Pts',(14.2468058395578,0.322795758952199,0.725928647976576));
#40387=CARTESIAN_POINT('Ctrl Pts',(14.2484814298548,0.208031110850766,1.08333333333333));
#40388=CARTESIAN_POINT('',(15.1423033840733,-0.0114224867026808,1.08333333333333));
#40389=CARTESIAN_POINT('Origin',(13.892722748591,-3.17092330887735,1.08333333333333));
#40390=CARTESIAN_POINT('Ctrl Pts',(15.1423033840733,-0.0114224867026912,
1.08333333333333));
#40391=CARTESIAN_POINT('Ctrl Pts',(15.1423953499066,0.110492695607724,0.727666221822789));
#40392=CARTESIAN_POINT('Ctrl Pts',(15.1413590080604,0.169498193350193,0.352782973842772));
#40393=CARTESIAN_POINT('Ctrl Pts',(15.1413590080604,0.169498193350193,-0.352782973842778));
#40394=CARTESIAN_POINT('Ctrl Pts',(15.1423953499066,0.110492695607724,-0.727666221822797));
#40395=CARTESIAN_POINT('Ctrl Pts',(15.1423033840733,-0.0114224867026924,
-1.08333333333334));
#40396=CARTESIAN_POINT('',(13.0227870731057,-2.97236616780865,3.45272288248773));
#40397=CARTESIAN_POINT('Origin',(13.0227870731057,-2.97236616780865,-2.9997830762867E-15));
#40398=CARTESIAN_POINT('',(14.7626584240763,-3.36948044994605,3.45272288248773));
#40399=CARTESIAN_POINT('Origin',(14.7626584240763,-3.36948044994605,-3.40056031423575E-15));
#40400=CARTESIAN_POINT('Origin',(11.1410986251693,8.88472967648709,-9.85584169237555E-16));
#40401=CARTESIAN_POINT('',(11.8387328710639,9.44107442276104,-3.96060240207311));
#40402=CARTESIAN_POINT('Origin',(11.8387328710639,9.44107442276104,-1.0472995612114E-15));
#40403=CARTESIAN_POINT('',(10.4434643792748,8.32838493021314,-3.96060240207311));
#40404=CARTESIAN_POINT('Origin',(11.1410986251693,8.88472967648709,-2.5198520116158));
#40405=CARTESIAN_POINT('Origin',(10.4434643792748,8.32838493021314,-9.23868777263706E-16));
#40406=CARTESIAN_POINT('',(8.89378902201275,12.2552029391784,1.08333333331655));
#40407=CARTESIAN_POINT('',(8.89378902201677,12.2552029391754,-1.08333333333333));
#40408=CARTESIAN_POINT('Ctrl Pts',(8.89378902201274,12.2552029391784,1.08333333331655));
#40409=CARTESIAN_POINT('Ctrl Pts',(8.86335293025879,12.2772908784853,0.956315399884826));
#40410=CARTESIAN_POINT('Ctrl Pts',(8.83824313040494,12.2953456493747,0.827586922367285));
#40411=CARTESIAN_POINT('Ctrl Pts',(8.81859777764014,12.3094197866805,0.69766772380084));
#40412=CARTESIAN_POINT('Ctrl Pts',(8.7991879276401,12.3233252073292,0.569305958731489));
#40413=CARTESIAN_POINT('Ctrl Pts',(8.78511225071473,12.3333449381983,0.439781849534452));
#40414=CARTESIAN_POINT('Ctrl Pts',(8.77647376760361,12.3394890678296,0.309596747993595));
#40415=CARTESIAN_POINT('Ctrl Pts',(8.76964787761092,12.344343988818,0.206728088024587));
#40416=CARTESIAN_POINT('Ctrl Pts',(8.76621624622163,12.3467783236357,0.103446722778746));
#40417=CARTESIAN_POINT('Ctrl Pts',(8.76621624622163,12.3467783236357,7.54951656745106E-15));
#40418=CARTESIAN_POINT('Ctrl Pts',(8.76621624622163,12.3467783236357,-0.130951008152141));
#40419=CARTESIAN_POINT('Ctrl Pts',(8.77171477448527,12.3428797767713,-0.261548325668487));
#40420=CARTESIAN_POINT('Ctrl Pts',(8.78261416841303,12.3351194002049,-0.391301356121213));
#40421=CARTESIAN_POINT('Ctrl Pts',(8.79368558213778,12.3272365454154,-0.523102215114213));
#40422=CARTESIAN_POINT('Ctrl Pts',(8.81032969837903,12.3153689336875,-0.654031926803563));
#40423=CARTESIAN_POINT('Ctrl Pts',(8.83241243050519,12.2995110840219,-0.783576297698762));
#40424=CARTESIAN_POINT('Ctrl Pts',(8.84960195907419,12.2871670969504,-0.88441557119687));
#40425=CARTESIAN_POINT('Ctrl Pts',(8.87008627043973,12.2724043900869,-0.984415425401903));
#40426=CARTESIAN_POINT('Ctrl Pts',(8.89378902201675,12.2552029391755,-1.08333333333333));
#40427=CARTESIAN_POINT('',(8.22258343557175,11.6383685130288,1.08333333333333));
#40428=CARTESIAN_POINT('Ctrl Pts',(8.89378902201473,12.2552029391744,1.08333333333333));
#40429=CARTESIAN_POINT('Ctrl Pts',(8.7875190745609,12.202353722575,1.08333333333333));
#40430=CARTESIAN_POINT('Ctrl Pts',(8.68681488082435,12.1369760343753,1.08333333333333));
#40431=CARTESIAN_POINT('Ctrl Pts',(8.46069343470619,11.9566501984405,1.08333333333333));
#40432=CARTESIAN_POINT('Ctrl Pts',(8.31988542322913,11.7983921800676,1.08333333333333));
#40433=CARTESIAN_POINT('Ctrl Pts',(8.22258343557172,11.6383685130288,1.08333333333333));
#40434=CARTESIAN_POINT('',(8.22258343557123,11.6383685130292,-1.08333333333333));
#40435=CARTESIAN_POINT('Ctrl Pts',(8.2225834355717,11.6383685130289,-1.08333333333318));
#40436=CARTESIAN_POINT('Ctrl Pts',(8.19448780675769,11.6582182584498,-0.949301954017324));
#40437=CARTESIAN_POINT('Ctrl Pts',(8.17159767874311,11.6742430454627,-0.81366496302888));
#40438=CARTESIAN_POINT('Ctrl Pts',(8.15402161030241,11.6865063889394,-0.67695567866062));
#40439=CARTESIAN_POINT('Ctrl Pts',(8.13658119548769,11.6986750828637,-0.541301528447691));
#40440=CARTESIAN_POINT('Ctrl Pts',(8.12437307855494,11.7071402381473,-0.40459157308691));
#40441=CARTESIAN_POINT('Ctrl Pts',(8.1174733585697,11.7119223986889,-0.26734687734235));
#40442=CARTESIAN_POINT('Ctrl Pts',(8.11300215046573,11.7150213700985,-0.178408544025479));
#40443=CARTESIAN_POINT('Ctrl Pts',(8.11075954642938,11.7165728598428,-0.0892456520429063));
#40444=CARTESIAN_POINT('Ctrl Pts',(8.11075954642938,11.7165728598428,1.33226762955019E-15));
#40445=CARTESIAN_POINT('Ctrl Pts',(8.11075954642938,11.7165728598428,0.137335411050026));
#40446=CARTESIAN_POINT('Ctrl Pts',(8.11607262981309,11.7129002012938,0.274553571737022));
#40447=CARTESIAN_POINT('Ctrl Pts',(8.12665801674411,11.7055512249056,0.411127959090392));
#40448=CARTESIAN_POINT('Ctrl Pts',(8.13729388250879,11.698167203246,0.548353632582512));
#40449=CARTESIAN_POINT('Ctrl Pts',(8.15325248641432,11.6870716767896,0.684929378140945));
#40450=CARTESIAN_POINT('Ctrl Pts',(8.17446212457132,11.6722178258439,0.820321104282498));
#40451=CARTESIAN_POINT('Ctrl Pts',(8.18828255682692,11.6625388940673,0.908543834215877));
#40452=CARTESIAN_POINT('Ctrl Pts',(8.20433194575505,11.6512633098961,0.9962638332735));
#40453=CARTESIAN_POINT('Ctrl Pts',(8.22258343557176,11.6383685130288,1.08333333333334));
#40454=CARTESIAN_POINT('Ctrl Pts',(8.89378902201675,12.2552029391755,-1.08333333333333));
#40455=CARTESIAN_POINT('Ctrl Pts',(8.78751907456219,12.2023537225759,-1.08333333333333));
#40456=CARTESIAN_POINT('Ctrl Pts',(8.68681488082489,12.1369760343758,-1.08333333333333));
#40457=CARTESIAN_POINT('Ctrl Pts',(8.46069343470621,11.9566501984405,-1.08333333333333));
#40458=CARTESIAN_POINT('Ctrl Pts',(8.31988542322917,11.7983921800676,-1.08333333333333));
#40459=CARTESIAN_POINT('Ctrl Pts',(8.22258343557176,11.6383685130289,-1.08333333333333));
#40460=CARTESIAN_POINT('',(13.9269936544443,5.94376395877129,1.08333333333333));
#40461=CARTESIAN_POINT('',(13.1762672612271,5.42664547033562,1.08333333333333));
#40462=CARTESIAN_POINT('Ctrl Pts',(13.9269936544443,5.94376395877129,1.08333333333333));
#40463=CARTESIAN_POINT('Ctrl Pts',(13.8517896638478,5.85187873682469,1.08333333333333));
#40464=CARTESIAN_POINT('Ctrl Pts',(13.7657237213495,5.76832601371371,1.08333333333333));
#40465=CARTESIAN_POINT('Ctrl Pts',(13.5395781511316,5.5879809394513,1.08333333333333));
#40466=CARTESIAN_POINT('Ctrl Pts',(13.3544742809805,5.48608062863226,1.08333333333333));
#40467=CARTESIAN_POINT('Ctrl Pts',(13.1762672612269,5.42664547033621,1.08333333333333));
#40468=CARTESIAN_POINT('',(13.9269936544443,5.94376395877129,-1.08333333333333));
#40469=CARTESIAN_POINT('Ctrl Pts',(13.9269936544443,5.9437639587713,1.08333333333333));
#40470=CARTESIAN_POINT('Ctrl Pts',(13.9416885168395,5.90933203032488,0.95688863210334));
#40471=CARTESIAN_POINT('Ctrl Pts',(13.9536527109305,5.88095561854266,0.828820583351241));
#40472=CARTESIAN_POINT('Ctrl Pts',(13.9629765258053,5.85873440158633,0.699646919261855));
#40473=CARTESIAN_POINT('Ctrl Pts',(13.9722513158077,5.83663002439342,0.571152453813261));
#40474=CARTESIAN_POINT('Ctrl Pts',(13.9789135007645,5.82061622745854,0.441563969171658));
#40475=CARTESIAN_POINT('Ctrl Pts',(13.9830050237944,5.81077040959811,0.31139107363785));
#40476=CARTESIAN_POINT('Ctrl Pts',(13.987063711968,5.80100360535004,0.182262827807452));
#40477=CARTESIAN_POINT('Ctrl Pts',(13.9885928700522,5.79730615639857,0.0525595133520559));
#40478=CARTESIAN_POINT('Ctrl Pts',(13.9875862925321,5.79973378332923,-0.077221432194654));
#40479=CARTESIAN_POINT('Ctrl Pts',(13.9868997670033,5.80138952054645,-0.165737150534494));
#40480=CARTESIAN_POINT('Ctrl Pts',(13.9850326975557,5.80589410253397,-0.254288981130278));
#40481=CARTESIAN_POINT('Ctrl Pts',(13.9819702480148,5.81325986277498,-0.342719102199545));
#40482=CARTESIAN_POINT('Ctrl Pts',(13.977353348451,5.82436436418423,-0.476034927301432));
#40483=CARTESIAN_POINT('Ctrl Pts',(13.9700489046451,5.84190742581571,-0.608312350205104));
#40484=CARTESIAN_POINT('Ctrl Pts',(13.9600480872369,5.86570879353505,-0.739057191236667));
#40485=CARTESIAN_POINT('Ctrl Pts',(13.9511688384277,5.88684089277784,-0.855139299993628));
#40486=CARTESIAN_POINT('Ctrl Pts',(13.9401632237805,5.91290598563348,-0.970013302477476));
#40487=CARTESIAN_POINT('Ctrl Pts',(13.9269936544443,5.9437639587713,-1.08333333333333));
#40488=CARTESIAN_POINT('',(13.1762672612355,5.42664547033908,-1.08333333333333));
#40489=CARTESIAN_POINT('Ctrl Pts',(13.9269936544443,5.94376395877129,-1.08333333333333));
#40490=CARTESIAN_POINT('Ctrl Pts',(13.8517896638478,5.85187873682469,-1.08333333333333));
#40491=CARTESIAN_POINT('Ctrl Pts',(13.7657237213495,5.76832601371371,-1.08333333333333));
#40492=CARTESIAN_POINT('Ctrl Pts',(13.5395781511339,5.5879809394531,-1.08333333333333));
#40493=CARTESIAN_POINT('Ctrl Pts',(13.3544742809865,5.48608062863536,-1.08333333333333));
#40494=CARTESIAN_POINT('Ctrl Pts',(13.1762672612355,5.42664547033908,-1.08333333333333));
#40495=CARTESIAN_POINT('Ctrl Pts',(13.1762672612269,5.42664547033617,-1.08333333333318));
#40496=CARTESIAN_POINT('Ctrl Pts',(13.1893705593041,5.39482976422236,-0.949270311030452));
#40497=CARTESIAN_POINT('Ctrl Pts',(13.1999097963792,5.36892368585892,-0.813521288368082));
#40498=CARTESIAN_POINT('Ctrl Pts',(13.2079621630868,5.34904061477083,-0.676607052101254));
#40499=CARTESIAN_POINT('Ctrl Pts',(13.2148460430323,5.33204279546023,-0.559560573777983));
#40500=CARTESIAN_POINT('Ctrl Pts',(13.2199117356377,5.31944645364959,-0.441662516279123));
#40501=CARTESIAN_POINT('Ctrl Pts',(13.2231796369647,5.31131059989547,-0.323238258334714));
#40502=CARTESIAN_POINT('Ctrl Pts',(13.2269557156993,5.30190957419912,-0.186398348762647));
#40503=CARTESIAN_POINT('Ctrl Pts',(13.2283213471703,5.2984924131362,-0.0492519096262126));
#40504=CARTESIAN_POINT('Ctrl Pts',(13.2273014856384,5.30103720115497,0.087675827066048));
#40505=CARTESIAN_POINT('Ctrl Pts',(13.2262786675026,5.30358936657715,0.225000520654307));
#40506=CARTESIAN_POINT('Ctrl Pts',(13.22285647475,5.31213809759657,0.362105241912749));
#40507=CARTESIAN_POINT('Ctrl Pts',(13.2170113253899,5.32664168351083,0.498460177595588));
#40508=CARTESIAN_POINT('Ctrl Pts',(13.2111409592133,5.34120783998435,0.635403368116607));
#40509=CARTESIAN_POINT('Ctrl Pts',(13.2028266475275,5.36178038996296,0.771590289741134));
#40510=CARTESIAN_POINT('Ctrl Pts',(13.1919958930594,5.38829698119018,0.906484242526414));
#40511=CARTESIAN_POINT('Ctrl Pts',(13.1872415508606,5.3999368857798,0.965698216399684));
#40512=CARTESIAN_POINT('Ctrl Pts',(13.1820016856381,5.41272189470467,1.02466304565381));
#40513=CARTESIAN_POINT('Ctrl Pts',(13.1762672612269,5.42664547033617,1.08333333333318));
#40514=CARTESIAN_POINT('Origin',(11.1410986251693,8.88472967648709,-9.85584169237555E-16));
#40515=CARTESIAN_POINT('',(8.72113759169208,11.2696166353064,-1.08333333333333));
#40516=CARTESIAN_POINT('',(9.02271027299523,11.54110464988,-1.08333333333333));
#40517=CARTESIAN_POINT('Origin',(11.1410986251693,8.88472967648709,-1.08333333333333));
#40518=CARTESIAN_POINT('',(8.72113759169208,11.2696166353064,1.08333333333333));
#40519=CARTESIAN_POINT('Ctrl Pts',(8.72113759169207,11.2696166353064,1.08333333333334));
#40520=CARTESIAN_POINT('Ctrl Pts',(8.63036626326973,11.3398611937657,0.725928647976583));
#40521=CARTESIAN_POINT('Ctrl Pts',(8.5862330966948,11.3727349924819,0.35203985917699));
#40522=CARTESIAN_POINT('Ctrl Pts',(8.5862330966948,11.3727349924819,-0.352039859176991));
#40523=CARTESIAN_POINT('Ctrl Pts',(8.63036626326973,11.3398611937657,-0.725928647976582));
#40524=CARTESIAN_POINT('Ctrl Pts',(8.72113759169207,11.2696166353064,-1.08333333333334));
#40525=CARTESIAN_POINT('',(9.4500021963329,11.8316076987797,1.08333333333333));
#40526=CARTESIAN_POINT('Origin',(11.1410986251693,8.88472967648709,1.08333333333333));
#40527=CARTESIAN_POINT('',(9.4500021963329,11.8316076987797,-1.08333333333333));
#40528=CARTESIAN_POINT('Ctrl Pts',(9.4500021963329,11.8316076987798,-1.08333333333334));
#40529=CARTESIAN_POINT('Ctrl Pts',(9.35474240837097,11.9076924734258,-0.7276662218228));
#40530=CARTESIAN_POINT('Ctrl Pts',(9.30796390402485,11.9436715548399,-0.352782973842779));
#40531=CARTESIAN_POINT('Ctrl Pts',(9.30796390402485,11.9436715548399,0.352782973842777));
#40532=CARTESIAN_POINT('Ctrl Pts',(9.35474240837097,11.9076924734258,0.727666221822799));
#40533=CARTESIAN_POINT('Ctrl Pts',(9.4500021963329,11.8316076987798,1.08333333333334));
#40534=CARTESIAN_POINT('Origin',(11.1410986251693,8.88472967648709,-1.08333333333333));
#40535=CARTESIAN_POINT('',(13.2594869773434,6.22835470309422,-1.08333333333333));
#40536=CARTESIAN_POINT('Origin',(11.1410986251693,8.88472967648709,-9.85584169237555E-16));
#40537=CARTESIAN_POINT('',(13.6377879061428,6.58029051604763,-1.08333333333333));
#40538=CARTESIAN_POINT('Origin',(11.1410986251693,8.88472967648709,-1.08333333333333));
#40539=CARTESIAN_POINT('',(13.6377879061428,6.58029051604763,1.08333333333333));
#40540=CARTESIAN_POINT('Ctrl Pts',(13.6377879061428,6.58029051604764,-1.08333333333332));
#40541=CARTESIAN_POINT('Ctrl Pts',(13.6907677796515,6.47048863474093,-0.727666221822788));
#40542=CARTESIAN_POINT('Ctrl Pts',(13.7154355939006,6.41687686636464,-0.352782973842773));
#40543=CARTESIAN_POINT('Ctrl Pts',(13.7154355939006,6.41687686636464,-9.86054494281319E-16));
#40544=CARTESIAN_POINT('Ctrl Pts',(13.7154355939006,6.41687686636464,0.352782973842772));
#40545=CARTESIAN_POINT('Ctrl Pts',(13.6907677796515,6.47048863474094,0.727666221822788));
#40546=CARTESIAN_POINT('Ctrl Pts',(13.6377879061428,6.58029051604764,1.08333333333332));
#40547=CARTESIAN_POINT('',(12.9276994994135,5.9947548451011,1.08333333333333));
#40548=CARTESIAN_POINT('Origin',(11.1410986251693,8.88472967648709,1.08333333333333));
#40549=CARTESIAN_POINT('',(12.9276994994135,5.9947548451011,-1.08333333333333));
#40550=CARTESIAN_POINT('Ctrl Pts',(12.9276994994135,5.9947548451011,1.08333333333333));
#40551=CARTESIAN_POINT('Ctrl Pts',(12.9759843593573,5.89062845864264,0.72592864797658));
#40552=CARTESIAN_POINT('Ctrl Pts',(12.9982133898606,5.84028669430273,0.352039859176989));
#40553=CARTESIAN_POINT('Ctrl Pts',(12.9982133898606,5.84028669430273,-9.85141416048961E-16));
#40554=CARTESIAN_POINT('Ctrl Pts',(12.9982133898606,5.84028669430273,-0.35203985917699));
#40555=CARTESIAN_POINT('Ctrl Pts',(12.9759843593573,5.89062845864264,-0.72592864797658));
#40556=CARTESIAN_POINT('Ctrl Pts',(12.9276994994135,5.9947548451011,-1.08333333333333));
#40557=CARTESIAN_POINT('Origin',(11.1410986251693,8.88472967648709,-1.08333333333333));
#40558=CARTESIAN_POINT('',(10.4434643792748,8.32838493021314,3.45272288248773));
#40559=CARTESIAN_POINT('Origin',(10.4434643792748,8.32838493021314,-9.23868777263706E-16));
#40560=CARTESIAN_POINT('',(11.8387328710639,9.44107442276105,3.45272288248773));
#40561=CARTESIAN_POINT('Origin',(11.8387328710639,9.44107442276104,-1.0472995612114E-15));
#40562=CARTESIAN_POINT('Origin',(0.,14.25,0.));
#40563=CARTESIAN_POINT('',(-3.35834339016074,14.7651959662676,-1.08333333333333));
#40564=CARTESIAN_POINT('',(-3.39763111739558,14.25,-1.08333333333333));
#40565=CARTESIAN_POINT('Origin',(1.55588456152529E-16,14.25,-1.08333333333333));
#40566=CARTESIAN_POINT('',(3.39763111739558,14.25,-1.08333333333333));
#40567=CARTESIAN_POINT('Origin',(0.,14.25,0.));
#40568=CARTESIAN_POINT('',(3.35834339016074,14.7651959662676,-1.08333333333333));
#40569=CARTESIAN_POINT('Origin',(0.,14.25,-1.08333333333333));
#40570=CARTESIAN_POINT('',(3.35834339016074,14.7651959662676,1.08333333333333));
#40571=CARTESIAN_POINT('Ctrl Pts',(3.35834339016074,14.7651959662676,-1.08333333333333));
#40572=CARTESIAN_POINT('Ctrl Pts',(3.47722236863702,14.7381569460943,-0.727666221822793));
#40573=CARTESIAN_POINT('Ctrl Pts',(3.53451786760282,14.7240166290356,-0.352782973842775));
#40574=CARTESIAN_POINT('Ctrl Pts',(3.53451786760282,14.7240166290356,0.));
#40575=CARTESIAN_POINT('Ctrl Pts',(3.53451786760282,14.7240166290356,0.352782973842776));
#40576=CARTESIAN_POINT('Ctrl Pts',(3.47722236863702,14.7381569460943,0.727666221822795));
#40577=CARTESIAN_POINT('Ctrl Pts',(3.35834339016074,14.7651959662676,1.08333333333333));
#40578=CARTESIAN_POINT('',(3.37340073180097,13.8449509750914,1.08333333333333));
#40579=CARTESIAN_POINT('Origin',(0.,14.25,1.08333333333333));
#40580=CARTESIAN_POINT('',(3.37340073180097,13.8449509750914,-1.08333333333333));
#40581=CARTESIAN_POINT('Ctrl Pts',(3.37340073180098,13.8449509750914,1.08333333333333));
#40582=CARTESIAN_POINT('Ctrl Pts',(3.48491513664897,13.8177798586608,0.725928647976577));
#40583=CARTESIAN_POINT('Ctrl Pts',(3.53813348671686,13.8037716378594,0.352039859176988));
#40584=CARTESIAN_POINT('Ctrl Pts',(3.53813348671686,13.8037716378594,0.));
#40585=CARTESIAN_POINT('Ctrl Pts',(3.53813348671686,13.8037716378594,-0.352039859176988));
#40586=CARTESIAN_POINT('Ctrl Pts',(3.48491513664897,13.8177798586608,-0.725928647976578));
#40587=CARTESIAN_POINT('Ctrl Pts',(3.37340073180098,13.8449509750914,-1.08333333333333));
#40588=CARTESIAN_POINT('Origin',(0.,14.25,-1.08333333333333));
#40589=CARTESIAN_POINT('',(-3.37340073180097,13.8449509750914,-1.08333333333333));
#40590=CARTESIAN_POINT('Origin',(1.55588456152529E-16,14.25,-1.08333333333333));
#40591=CARTESIAN_POINT('',(-3.37340073180097,13.8449509750914,1.08333333333333));
#40592=CARTESIAN_POINT('Ctrl Pts',(-3.37340073180098,13.8449509750914,-1.08333333333333));
#40593=CARTESIAN_POINT('Ctrl Pts',(-3.48491513664897,13.8177798586608,-0.725928647976578));
#40594=CARTESIAN_POINT('Ctrl Pts',(-3.53813348671686,13.8037716378594,-0.352039859176988));
#40595=CARTESIAN_POINT('Ctrl Pts',(-3.53813348671686,13.8037716378594,0.352039859176988));
#40596=CARTESIAN_POINT('Ctrl Pts',(-3.48491513664897,13.8177798586608,0.725928647976578));
#40597=CARTESIAN_POINT('Ctrl Pts',(-3.37340073180098,13.8449509750914,1.08333333333333));
#40598=CARTESIAN_POINT('',(-3.35834339016074,14.7651959662676,1.08333333333333));
#40599=CARTESIAN_POINT('Origin',(-1.5558845615253E-16,14.25,1.08333333333333));
#40600=CARTESIAN_POINT('Ctrl Pts',(-3.35834339016074,14.7651959662676,1.08333333333333));
#40601=CARTESIAN_POINT('Ctrl Pts',(-3.47722236863702,14.7381569460943,0.727666221822794));
#40602=CARTESIAN_POINT('Ctrl Pts',(-3.53451786760282,14.7240166290356,0.352782973842775));
#40603=CARTESIAN_POINT('Ctrl Pts',(-3.53451786760282,14.7240166290356,-0.352782973842776));
#40604=CARTESIAN_POINT('Ctrl Pts',(-3.47722236863702,14.7381569460943,-0.727666221822794));
#40605=CARTESIAN_POINT('Ctrl Pts',(-3.35834339016074,14.7651959662676,-1.08333333333333));
#40606=CARTESIAN_POINT('',(0.,13.3576923076923,3.45272288248773));
#40607=CARTESIAN_POINT('Origin',(0.,13.3576923076923,0.));
#40608=CARTESIAN_POINT('',(0.,15.1423076923077,3.45272288248773));
#40609=CARTESIAN_POINT('Origin',(0.,15.1423076923077,0.));
#40610=CARTESIAN_POINT('Origin',(0.,14.25,0.));
#40611=CARTESIAN_POINT('',(-4.85033905439415E-16,15.1423076923077,-3.96060240207311));
#40612=CARTESIAN_POINT('Origin',(0.,15.1423076923077,0.));
#40613=CARTESIAN_POINT('',(-4.85033905439415E-16,13.3576923076923,-3.96060240207311));
#40614=CARTESIAN_POINT('Origin',(-3.08592870035031E-16,14.25,-2.5198520116158));
#40615=CARTESIAN_POINT('Origin',(0.,13.3576923076923,0.));
#40616=CARTESIAN_POINT('',(-3.97254599103887,13.6850786752975,1.08333333333333));
#40617=CARTESIAN_POINT('',(-4.03631672677061,14.5944383081266,1.08333333333333));
#40618=CARTESIAN_POINT('Ctrl Pts',(-3.97254599103889,13.6850786752975,1.08333333333333));
#40619=CARTESIAN_POINT('Ctrl Pts',(-4.03699073486477,13.8609255570095,1.08333333333333));
#40620=CARTESIAN_POINT('Ctrl Pts',(-4.07292947680577,14.0696859538838,1.08333333333333));
#40621=CARTESIAN_POINT('Ctrl Pts',(-4.07292947680577,14.358906139038,1.08333333333333));
#40622=CARTESIAN_POINT('Ctrl Pts',(-4.06125577389194,14.4784021699804,1.08333333333333));
#40623=CARTESIAN_POINT('Ctrl Pts',(-4.03631672677123,14.5944383081267,1.08333333333333));
#40624=CARTESIAN_POINT('',(-3.97254599103887,13.6850786752975,-1.08333333333333));
#40625=CARTESIAN_POINT('Ctrl Pts',(-3.97254599103885,13.6850786752975,1.08333333333333));
#40626=CARTESIAN_POINT('Ctrl Pts',(-4.0055902844374,13.6754864779574,0.949270311030653));
#40627=CARTESIAN_POINT('Ctrl Pts',(-4.03241557892495,13.6675742096383,0.813521288368336));
#40628=CARTESIAN_POINT('Ctrl Pts',(-4.05298135839275,13.6614729113855,0.67660705210156));
#40629=CARTESIAN_POINT('Ctrl Pts',(-4.07056281760631,13.6562569784544,0.559560573778188));
#40630=CARTESIAN_POINT('Ctrl Pts',(-4.08356944187665,13.6523638057542,0.441662516279225));
#40631=CARTESIAN_POINT('Ctrl Pts',(-4.09196781162929,13.6498461320482,0.32323825833471));
#40632=CARTESIAN_POINT('Ctrl Pts',(-4.10167217606822,13.6469369456345,0.186398348762652));
#40633=CARTESIAN_POINT('Ctrl Pts',(-4.10519527746315,13.6458740742379,0.0492519096262281));
#40634=CARTESIAN_POINT('Ctrl Pts',(-4.1025698088094,13.6466633637621,-0.0876758270660229));
#40635=CARTESIAN_POINT('Ctrl Pts',(-4.09993672885708,13.6474549414561,-0.225000520654293));
#40636=CARTESIAN_POINT('Ctrl Pts',(-4.0911193595297,13.6501094100325,-0.362105241912746));
#40637=CARTESIAN_POINT('Ctrl Pts',(-4.07613560843688,13.6545823261509,-0.498460177595596));
#40638=CARTESIAN_POINT('Ctrl Pts',(-4.06108721528303,13.659074539074,-0.635403368116582));
#40639=CARTESIAN_POINT('Ctrl Pts',(-4.03981905948952,13.6654009235528,-0.771590289741077));
#40640=CARTESIAN_POINT('Ctrl Pts',(-4.01233468870309,13.673465922941,-0.906484242526326));
#40641=CARTESIAN_POINT('Ctrl Pts',(-4.00026996096645,13.6770061903378,-0.965698216399675));
#40642=CARTESIAN_POINT('Ctrl Pts',(-3.98700723595603,13.6808808214243,-1.02466304565388));
#40643=CARTESIAN_POINT('Ctrl Pts',(-3.97254599103885,13.6850786752975,-1.08333333333333));
#40644=CARTESIAN_POINT('',(-4.03631672677098,14.5944383081279,-1.08333333333333));
#40645=CARTESIAN_POINT('Ctrl Pts',(-3.97254599103889,13.6850786752975,-1.08333333333333));
#40646=CARTESIAN_POINT('Ctrl Pts',(-4.03718797255354,13.8614637488071,-1.08333333333333));
#40647=CARTESIAN_POINT('Ctrl Pts',(-4.07292947680577,14.0697175866198,-1.08333333333333));
#40648=CARTESIAN_POINT('Ctrl Pts',(-4.07292947680577,14.3589686276554,-1.08333333333333));
#40649=CARTESIAN_POINT('Ctrl Pts',(-4.06126656486658,14.4783519618466,-1.08333333333333));
#40650=CARTESIAN_POINT('Ctrl Pts',(-4.03631672677098,14.5944383081279,-1.08333333333333));
#40651=CARTESIAN_POINT('Ctrl Pts',(-4.03631672677125,14.5944383081264,-1.08333333333353));
#40652=CARTESIAN_POINT('Ctrl Pts',(-4.07239878927587,14.5844592579328,-0.956888632103535));
#40653=CARTESIAN_POINT('Ctrl Pts',(-4.10204391436992,14.576120838176,-0.828820583351431));
#40654=CARTESIAN_POINT('Ctrl Pts',(-4.12523046485396,14.5695557880246,-0.699646919262042));
#40655=CARTESIAN_POINT('Ctrl Pts',(-4.14829509982461,14.5630252570856,-0.571152453813459));
#40656=CARTESIAN_POINT('Ctrl Pts',(-4.16496899480084,14.5582495239489,-0.441563969171867));
#40657=CARTESIAN_POINT('Ctrl Pts',(-4.17521778805797,14.555309638438,-0.311391073638072));
#40658=CARTESIAN_POINT('Ctrl Pts',(-4.18538433378736,14.5523933457842,-0.182262827807668));
#40659=CARTESIAN_POINT('Ctrl Pts',(-4.18922853025337,14.5512835680019,-0.0525595133522669));
#40660=CARTESIAN_POINT('Ctrl Pts',(-4.18670294427272,14.5520101946411,0.0772214321944475));
#40661=CARTESIAN_POINT('Ctrl Pts',(-4.18498039512374,14.5525057826387,0.165737150534356));
#40662=CARTESIAN_POINT('Ctrl Pts',(-4.1802944723506,14.5538546098955,0.254288981130209));
#40663=CARTESIAN_POINT('Ctrl Pts',(-4.17262628304436,14.5560527668241,0.342719102199544));
#40664=CARTESIAN_POINT('Ctrl Pts',(-4.16106584445129,14.5593666727772,0.476034927301542));
#40665=CARTESIAN_POINT('Ctrl Pts',(-4.14279588034764,14.5645937486684,0.608312350205319));
#40666=CARTESIAN_POINT('Ctrl Pts',(-4.11795181407459,14.5716147048116,0.739057191236983));
#40667=CARTESIAN_POINT('Ctrl Pts',(-4.09589395251526,14.5778482769217,0.855139299993905));
#40668=CARTESIAN_POINT('Ctrl Pts',(-4.06865355383155,14.5854950604866,0.970013302477714));
#40669=CARTESIAN_POINT('Ctrl Pts',(-4.03631672677125,14.5944383081264,1.08333333333353));
#40670=CARTESIAN_POINT('',(4.0363167267713,14.5944383081264,1.08333333333333));
#40671=CARTESIAN_POINT('',(3.97254599103947,13.6850786752973,1.08333333333333));
#40672=CARTESIAN_POINT('Ctrl Pts',(4.0363167267713,14.5944383081264,1.08333333333333));
#40673=CARTESIAN_POINT('Ctrl Pts',(4.06125577389196,14.4784021699801,1.08333333333333));
#40674=CARTESIAN_POINT('Ctrl Pts',(4.07292947680577,14.3589061390379,1.08333333333333));
#40675=CARTESIAN_POINT('Ctrl Pts',(4.07292947680577,14.0696859538838,1.08333333333333));
#40676=CARTESIAN_POINT('Ctrl Pts',(4.03699073486477,13.8609255570095,1.08333333333333));
#40677=CARTESIAN_POINT('Ctrl Pts',(3.97254599103889,13.6850786752975,1.08333333333333));
#40678=CARTESIAN_POINT('',(4.0363167267713,14.5944383081264,-1.08333333333333));
#40679=CARTESIAN_POINT('Ctrl Pts',(4.0363167267713,14.5944383081264,1.08333333333333));
#40680=CARTESIAN_POINT('Ctrl Pts',(4.07267660468553,14.5843824238018,0.955915065626592));
#40681=CARTESIAN_POINT('Ctrl Pts',(4.10254364280131,14.5759803979714,0.826701571450557));
#40682=CARTESIAN_POINT('Ctrl Pts',(4.12584816889326,14.5693808768856,0.696211209492171));
#40683=CARTESIAN_POINT('Ctrl Pts',(4.14878536602558,14.5628853783063,0.567777653525462));
#40684=CARTESIAN_POINT('Ctrl Pts',(4.16536539316191,14.5581360328796,0.438107164856169));
#40685=CARTESIAN_POINT('Ctrl Pts',(4.17550906341001,14.5552260824043,0.307693975181436));
#40686=CARTESIAN_POINT('Ctrl Pts',(4.18345734283739,14.55294593144,0.205506064179161));
#40687=CARTESIAN_POINT('Ctrl Pts',(4.18745357006455,14.5517942140162,0.102862147740973));
#40688=CARTESIAN_POINT('Ctrl Pts',(4.18745357006455,14.5517942140162,-4.44089209850063E-16));
#40689=CARTESIAN_POINT('Ctrl Pts',(4.18745357006455,14.5517942140162,-0.13066680730557));
#40690=CARTESIAN_POINT('Ctrl Pts',(4.18100368362964,14.5536548201376,-0.261069786498731));
#40691=CARTESIAN_POINT('Ctrl Pts',(4.16817103415993,14.5573291670729,-0.390710450871123));
#40692=CARTESIAN_POINT('Ctrl Pts',(4.15518429935153,14.561047632956,-0.521907748246283));
#40693=CARTESIAN_POINT('Ctrl Pts',(4.13566054561854,14.5666236366129,-0.652324314224272));
#40694=CARTESIAN_POINT('Ctrl Pts',(4.10965488440249,14.5739568744946,-0.781443489202978));
#40695=CARTESIAN_POINT('Ctrl Pts',(4.08920880779353,14.5797223861759,-0.882959098491578));
#40696=CARTESIAN_POINT('Ctrl Pts',(4.06475571708163,14.586573067282,-0.983672743459539));
#40697=CARTESIAN_POINT('Ctrl Pts',(4.0363167267713,14.5944383081264,-1.08333333333333));
#40698=CARTESIAN_POINT('',(3.972545991042,13.685078675306,-1.08333333333333));
#40699=CARTESIAN_POINT('Ctrl Pts',(4.0363167267713,14.5944383081264,-1.08333333333333));
#40700=CARTESIAN_POINT('Ctrl Pts',(4.06125577389196,14.4784021699801,-1.08333333333333));
#40701=CARTESIAN_POINT('Ctrl Pts',(4.07292947680577,14.3589061390379,-1.08333333333333));
#40702=CARTESIAN_POINT('Ctrl Pts',(4.07292947680577,14.0696859538867,-1.08333333333333));
#40703=CARTESIAN_POINT('Ctrl Pts',(4.03699073486612,13.8609255570161,-1.08333333333333));
#40704=CARTESIAN_POINT('Ctrl Pts',(3.97254599104201,13.685078675306,-1.08333333333333));
#40705=CARTESIAN_POINT('Ctrl Pts',(3.97254599103891,13.6850786752974,-1.08333333333318));
#40706=CARTESIAN_POINT('Ctrl Pts',(4.00550358468898,13.6755116454224,-0.949622058007565));
#40707=CARTESIAN_POINT('Ctrl Pts',(4.03223833992508,13.667626413385,-0.814376693553222));
#40708=CARTESIAN_POINT('Ctrl Pts',(4.05275116551691,13.6615412011384,-0.678132403728152));
#40709=CARTESIAN_POINT('Ctrl Pts',(4.07316650047532,13.6554849098804,-0.542535637670838));
#40710=CARTESIAN_POINT('Ctrl Pts',(4.0874189867075,13.6512115628239,-0.40594941879892));
#40711=CARTESIAN_POINT('Ctrl Pts',(4.09549564973878,13.6487880554638,-0.268901316711817));
#40712=CARTESIAN_POINT('Ctrl Pts',(4.10076932144717,13.6472056219574,-0.179415511018788));
#40713=CARTESIAN_POINT('Ctrl Pts',(4.10340966592831,13.6464108509735,-0.0897327832366672));
#40714=CARTESIAN_POINT('Ctrl Pts',(4.10340966592831,13.6464108509735,4.66293670342566E-15));
#40715=CARTESIAN_POINT('Ctrl Pts',(4.10340966592831,13.6464108509735,0.137573936980382));
#40716=CARTESIAN_POINT('Ctrl Pts',(4.09720533291532,13.6482810316174,0.274951212619736));
#40717=CARTESIAN_POINT('Ctrl Pts',(4.08483748845152,13.6519816397819,0.41161240621476));
#40718=CARTESIAN_POINT('Ctrl Pts',(4.07237395114171,13.6557108803995,0.549330978772818));
#40719=CARTESIAN_POINT('Ctrl Pts',(4.05365110225785,13.6612989721827,0.686322345436846));
#40720=CARTESIAN_POINT('Ctrl Pts',(4.02869583028489,13.6686542829587,0.822054935347102));
#40721=CARTESIAN_POINT('Ctrl Pts',(4.01257796374822,13.6734048590114,0.909720570537157));
#40722=CARTESIAN_POINT('Ctrl Pts',(3.99385994844905,13.6788915953345,0.996861109122728));
#40723=CARTESIAN_POINT('Ctrl Pts',(3.97254599103891,13.6850786752974,1.08333333333318));
#40724=CARTESIAN_POINT('Origin',(0.,0.,1.08333333333333));
#40725=CARTESIAN_POINT('Origin',(0.,0.,-1.08333333333333));
#40726=CARTESIAN_POINT('Origin',(0.,0.,1.08333333333333));
#40727=CARTESIAN_POINT('Origin',(0.,0.,1.08333333333333));
#40728=CARTESIAN_POINT('Origin',(0.,0.,1.08333333333333));
#40729=CARTESIAN_POINT('Origin',(0.,0.,-1.08333333333333));
#40730=CARTESIAN_POINT('Origin',(0.,0.,1.08333333333333));
#40731=CARTESIAN_POINT('Origin',(0.,0.,-1.08333333333333));
#40732=CARTESIAN_POINT('Origin',(0.,15.1423076923077,3.45272288248773));
#40733=CARTESIAN_POINT('Origin',(0.,13.3576923076923,3.45272288248773));
#40734=CARTESIAN_POINT('Origin',(0.,0.,1.08333333333333));
#40735=CARTESIAN_POINT('Origin',(0.,0.,1.08333333333333));
#40736=CARTESIAN_POINT('Origin',(0.,0.,1.08333333333333));
#40737=CARTESIAN_POINT('Origin',(0.,0.,-1.08333333333333));
#40738=CARTESIAN_POINT('Origin',(0.,0.,-1.08333333333333));
#40739=CARTESIAN_POINT('Origin',(0.,0.,-1.08333333333333));
#40740=CARTESIAN_POINT('Origin',(0.,0.,1.08333333333333));
#40741=CARTESIAN_POINT('Origin',(0.,0.,1.08333333333333));
#40742=CARTESIAN_POINT('Origin',(10.4434643792748,8.32838493021314,3.45272288248773));
#40743=CARTESIAN_POINT('Origin',(11.8387328710639,9.44107442276104,3.45272288248773));
#40744=CARTESIAN_POINT('Origin',(-1.55588456152528E-16,7.49274514625042E-17,
-1.08333333333333));
#40745=CARTESIAN_POINT('Origin',(-1.55588456152528E-16,7.49274514625042E-17,
-1.08333333333333));
#40746=CARTESIAN_POINT('Origin',(-1.55588456152528E-16,7.49274514625042E-17,
-1.08333333333333));
#40747=CARTESIAN_POINT('Origin',(1.55588456152528E-16,-7.49274514625042E-17,
1.08333333333333));
#40748=CARTESIAN_POINT('Origin',(1.55588456152528E-16,-7.49274514625042E-17,
1.08333333333333));
#40749=CARTESIAN_POINT('Origin',(1.55588456152528E-16,-7.49274514625042E-17,
1.08333333333333));
#40750=CARTESIAN_POINT('Origin',(1.55588456152528E-16,-7.49274514625042E-17,
1.08333333333333));
#40751=CARTESIAN_POINT('Origin',(1.55588456152528E-16,-7.49274514625042E-17,
1.08333333333333));
#40752=CARTESIAN_POINT('Origin',(1.94015631396094E-16,-2.43287906657286E-16,
1.08333333333333));
#40753=CARTESIAN_POINT('Origin',(1.94015631396094E-16,-2.43287906657286E-16,
1.08333333333333));
#40754=CARTESIAN_POINT('Origin',(-1.94015631396094E-16,2.43287906657286E-16,
-1.08333333333333));
#40755=CARTESIAN_POINT('Origin',(1.94015631396094E-16,-2.43287906657286E-16,
1.08333333333333));
#40756=CARTESIAN_POINT('Origin',(-1.94015631396094E-16,2.43287906657286E-16,
-1.08333333333333));
#40757=CARTESIAN_POINT('Origin',(1.94015631396094E-16,-2.43287906657286E-16,
1.08333333333333));
#40758=CARTESIAN_POINT('Origin',(-1.94015631396094E-16,2.43287906657286E-16,
-1.08333333333333));
#40759=CARTESIAN_POINT('Origin',(1.94015631396094E-16,-2.43287906657286E-16,
1.08333333333333));
#40760=CARTESIAN_POINT('Origin',(13.0227870731057,-2.97236616780865,3.45272288248773));
#40761=CARTESIAN_POINT('Origin',(14.7626584240763,-3.36948044994605,3.45272288248773));
#40762=CARTESIAN_POINT('Origin',(-1.94015631396094E-16,2.43287906657286E-16,
-1.08333333333333));
#40763=CARTESIAN_POINT('Origin',(-1.94015631396094E-16,2.43287906657286E-16,
-1.08333333333333));
#40764=CARTESIAN_POINT('Origin',(-1.94015631396094E-16,2.43287906657286E-16,
-1.08333333333333));
#40765=CARTESIAN_POINT('Origin',(1.94015631396094E-16,-2.43287906657286E-16,
1.08333333333333));
#40766=CARTESIAN_POINT('Origin',(1.94015631396094E-16,-2.43287906657286E-16,
1.08333333333333));
#40767=CARTESIAN_POINT('Origin',(1.94015631396094E-16,-2.43287906657286E-16,
1.08333333333333));
#40768=CARTESIAN_POINT('Origin',(1.94015631396094E-16,-2.43287906657286E-16,
1.08333333333333));
#40769=CARTESIAN_POINT('Origin',(1.94015631396094E-16,-2.43287906657286E-16,
1.08333333333333));
#40770=CARTESIAN_POINT('Origin',(8.63450790007668E-17,-3.78302508895262E-16,
1.08333333333333));
#40771=CARTESIAN_POINT('Origin',(8.63450790007668E-17,-3.78302508895262E-16,
1.08333333333333));
#40772=CARTESIAN_POINT('Origin',(-8.63450790007668E-17,3.78302508895262E-16,
-1.08333333333333));
#40773=CARTESIAN_POINT('Origin',(8.63450790007668E-17,-3.78302508895262E-16,
1.08333333333333));
#40774=CARTESIAN_POINT('Origin',(-8.63450790007668E-17,3.78302508895262E-16,
-1.08333333333333));
#40775=CARTESIAN_POINT('Origin',(8.63450790007668E-17,-3.78302508895262E-16,
1.08333333333333));
#40776=CARTESIAN_POINT('Origin',(-8.63450790007668E-17,3.78302508895262E-16,
-1.08333333333333));
#40777=CARTESIAN_POINT('Origin',(8.63450790007668E-17,-3.78302508895262E-16,
1.08333333333333));
#40778=CARTESIAN_POINT('Origin',(5.79568548444348,-12.0348649162504,3.45272288248773));
#40779=CARTESIAN_POINT('Origin',(6.57000108040713,-13.6427478189685,3.45272288248772));
#40780=CARTESIAN_POINT('Origin',(-8.63450790007668E-17,3.78302508895262E-16,
-1.08333333333333));
#40781=CARTESIAN_POINT('Origin',(-8.63450790007668E-17,3.78302508895262E-16,
-1.08333333333333));
#40782=CARTESIAN_POINT('Origin',(-8.63450790007668E-17,3.78302508895262E-16,
-1.08333333333333));
#40783=CARTESIAN_POINT('Origin',(8.63450790007668E-17,-3.78302508895262E-16,
1.08333333333333));
#40784=CARTESIAN_POINT('Origin',(8.63450790007668E-17,-3.78302508895262E-16,
1.08333333333333));
#40785=CARTESIAN_POINT('Origin',(8.63450790007668E-17,-3.78302508895262E-16,
1.08333333333333));
#40786=CARTESIAN_POINT('Origin',(8.63450790007668E-17,-3.78302508895262E-16,
1.08333333333333));
#40787=CARTESIAN_POINT('Origin',(8.63450790007668E-17,-3.78302508895262E-16,
1.08333333333333));
#40788=CARTESIAN_POINT('Origin',(-8.63450790007644E-17,-3.78302508895264E-16,
1.08333333333333));
#40789=CARTESIAN_POINT('Origin',(-8.63450790007644E-17,-3.78302508895264E-16,
1.08333333333333));
#40790=CARTESIAN_POINT('Origin',(8.63450790007644E-17,3.78302508895264E-16,
-1.08333333333333));
#40791=CARTESIAN_POINT('Origin',(-8.63450790007644E-17,-3.78302508895264E-16,
1.08333333333333));
#40792=CARTESIAN_POINT('Origin',(8.63450790007644E-17,3.78302508895264E-16,
-1.08333333333333));
#40793=CARTESIAN_POINT('Origin',(-8.63450790007644E-17,-3.78302508895264E-16,
1.08333333333333));
#40794=CARTESIAN_POINT('Origin',(8.63450790007644E-17,3.78302508895264E-16,
-1.08333333333333));
#40795=CARTESIAN_POINT('Origin',(-8.63450790007644E-17,-3.78302508895264E-16,
1.08333333333333));
#40796=CARTESIAN_POINT('Origin',(-5.79568548444331,-12.0348649162504,3.45272288248773));
#40797=CARTESIAN_POINT('Origin',(-6.57000108040694,-13.6427478189686,3.45272288248772));
#40798=CARTESIAN_POINT('Origin',(8.63450790007644E-17,3.78302508895264E-16,
-1.08333333333333));
#40799=CARTESIAN_POINT('Origin',(8.63450790007644E-17,3.78302508895264E-16,
-1.08333333333333));
#40800=CARTESIAN_POINT('Origin',(8.63450790007644E-17,3.78302508895264E-16,
-1.08333333333333));
#40801=CARTESIAN_POINT('Origin',(-8.63450790007644E-17,-3.78302508895264E-16,
1.08333333333333));
#40802=CARTESIAN_POINT('Origin',(-8.63450790007644E-17,-3.78302508895264E-16,
1.08333333333333));
#40803=CARTESIAN_POINT('Origin',(-8.63450790007644E-17,-3.78302508895264E-16,
1.08333333333333));
#40804=CARTESIAN_POINT('Origin',(-8.63450790007644E-17,-3.78302508895264E-16,
1.08333333333333));
#40805=CARTESIAN_POINT('Origin',(-8.63450790007644E-17,-3.78302508895264E-16,
1.08333333333333));
#40806=CARTESIAN_POINT('Origin',(-1.94015631396093E-16,-2.43287906657289E-16,
1.08333333333333));
#40807=CARTESIAN_POINT('Origin',(-1.94015631396093E-16,-2.43287906657289E-16,
1.08333333333333));
#40808=CARTESIAN_POINT('Origin',(1.94015631396093E-16,2.43287906657289E-16,
-1.08333333333333));
#40809=CARTESIAN_POINT('Origin',(-1.94015631396093E-16,-2.43287906657289E-16,
1.08333333333333));
#40810=CARTESIAN_POINT('Origin',(1.94015631396093E-16,2.43287906657289E-16,
-1.08333333333333));
#40811=CARTESIAN_POINT('Origin',(-1.94015631396093E-16,-2.43287906657289E-16,
1.08333333333333));
#40812=CARTESIAN_POINT('Origin',(1.94015631396093E-16,2.43287906657289E-16,
-1.08333333333333));
#40813=CARTESIAN_POINT('Origin',(-1.94015631396093E-16,-2.43287906657289E-16,
1.08333333333333));
#40814=CARTESIAN_POINT('Origin',(-13.0227870731057,-2.97236616780882,3.45272288248773));
#40815=CARTESIAN_POINT('Origin',(-14.7626584240763,-3.36948044994625,3.45272288248773));
#40816=CARTESIAN_POINT('Origin',(1.94015631396093E-16,2.43287906657289E-16,
-1.08333333333333));
#40817=CARTESIAN_POINT('Origin',(1.94015631396093E-16,2.43287906657289E-16,
-1.08333333333333));
#40818=CARTESIAN_POINT('Origin',(1.94015631396093E-16,2.43287906657289E-16,
-1.08333333333333));
#40819=CARTESIAN_POINT('Origin',(-1.94015631396093E-16,-2.43287906657289E-16,
1.08333333333333));
#40820=CARTESIAN_POINT('Origin',(-1.94015631396093E-16,-2.43287906657289E-16,
1.08333333333333));
#40821=CARTESIAN_POINT('Origin',(-1.94015631396093E-16,-2.43287906657289E-16,
1.08333333333333));
#40822=CARTESIAN_POINT('Origin',(-1.94015631396093E-16,-2.43287906657289E-16,
1.08333333333333));
#40823=CARTESIAN_POINT('Origin',(-1.94015631396093E-16,-2.43287906657289E-16,
1.08333333333333));
#40824=CARTESIAN_POINT('Origin',(-1.55588456152529E-16,-7.49274514625064E-17,
1.08333333333333));
#40825=CARTESIAN_POINT('Origin',(-1.55588456152529E-16,-7.49274514625064E-17,
1.08333333333333));
#40826=CARTESIAN_POINT('Origin',(1.55588456152529E-16,7.49274514625064E-17,
-1.08333333333333));
#40827=CARTESIAN_POINT('Origin',(-1.55588456152529E-16,-7.49274514625064E-17,
1.08333333333333));
#40828=CARTESIAN_POINT('Origin',(1.55588456152529E-16,7.49274514625064E-17,
-1.08333333333333));
#40829=CARTESIAN_POINT('Origin',(-1.55588456152529E-16,-7.49274514625064E-17,
1.08333333333333));
#40830=CARTESIAN_POINT('Origin',(1.55588456152529E-16,7.49274514625064E-17,
-1.08333333333333));
#40831=CARTESIAN_POINT('Origin',(-1.55588456152529E-16,-7.49274514625064E-17,
1.08333333333333));
#40832=CARTESIAN_POINT('Origin',(-10.4434643792749,8.32838493021299,3.45272288248773));
#40833=CARTESIAN_POINT('Origin',(-11.838732871064,9.44107442276088,3.45272288248773));
#40834=CARTESIAN_POINT('Origin',(1.55588456152529E-16,7.49274514625064E-17,
-1.08333333333333));
#40835=CARTESIAN_POINT('Origin',(1.55588456152529E-16,7.49274514625064E-17,
-1.08333333333333));
#40836=CARTESIAN_POINT('Origin',(1.55588456152529E-16,7.49274514625064E-17,
-1.08333333333333));
#40837=CARTESIAN_POINT('Origin',(-1.55588456152529E-16,-7.49274514625064E-17,
1.08333333333333));
#40838=CARTESIAN_POINT('Origin',(-1.55588456152529E-16,-7.49274514625064E-17,
1.08333333333333));
#40839=CARTESIAN_POINT('Origin',(-1.55588456152529E-16,-7.49274514625064E-17,
1.08333333333333));
#40840=CARTESIAN_POINT('Origin',(-1.55588456152529E-16,-7.49274514625064E-17,
1.08333333333333));
#40841=CARTESIAN_POINT('Origin',(-1.55588456152529E-16,-7.49274514625064E-17,
1.08333333333333));
#40842=CARTESIAN_POINT('Origin',(0.,0.,1.08333333333333));
#40843=CARTESIAN_POINT('Origin',(0.,0.,1.08333333333333));
#40844=CARTESIAN_POINT('Origin',(0.,0.,1.08333333333333));
#40845=CARTESIAN_POINT('Origin',(0.,0.,-1.08333333333333));
#40846=CARTESIAN_POINT('Origin',(0.,0.,-1.08333333333333));
#40847=CARTESIAN_POINT('Origin',(0.,0.,-1.08333333333333));
#40848=CARTESIAN_POINT('Origin',(0.,0.,1.08333333333333));
#40849=CARTESIAN_POINT('Origin',(0.,0.,1.08333333333333));
#40850=CARTESIAN_POINT('',(0.,0.,0.));
#40851=CARTESIAN_POINT('Origin',(0.,1.73472347597681E-15,6.67403582113016E-15));
#40852=CARTESIAN_POINT('',(1.52656933693714E-15,12.4653846153846,-3.0875));
#40853=CARTESIAN_POINT('Origin',(0.,6.26866080313552E-16,-3.0875));
#40854=CARTESIAN_POINT('',(-1.52656933693714E-15,12.4653846153846,3.0875));
#40855=CARTESIAN_POINT('Origin',(1.74512168878498E-15,14.25,4.05635328795269E-15));
#40856=CARTESIAN_POINT('Origin',(0.,1.76119517802379E-15,3.0875));
#40857=CARTESIAN_POINT('Origin',(0.,1.56496838953657E-16,-5.64807088834312));
#40858=CARTESIAN_POINT('',(9.67029207191279E-16,7.64278544417155,-5.99278544417156));
#40859=CARTESIAN_POINT('',(9.35971273077467E-16,-7.64278544417155,-5.99278544417156));
#40860=CARTESIAN_POINT('Origin',(0.,9.31738023414375E-17,-5.99278544417156));
#40861=CARTESIAN_POINT('',(9.18485099360515E-16,-7.5,-5.64807088834312));
#40862=CARTESIAN_POINT('Origin',(9.78186630818948E-16,-7.9875,-5.64807088834312));
#40863=CARTESIAN_POINT('',(9.18485099360515E-16,7.5,-5.64807088834312));
#40864=CARTESIAN_POINT('Origin',(0.,1.56496838953657E-16,-5.64807088834312));
#40865=CARTESIAN_POINT('Origin',(0.,1.56496838953657E-16,-5.64807088834312));
#40866=CARTESIAN_POINT('Origin',(0.,9.31738023414375E-17,-5.99278544417156));
#40867=CARTESIAN_POINT('Origin',(0.,2.23156441938368E-15,5.64807088834312));
#40868=CARTESIAN_POINT('',(9.18485099360515E-16,7.5,5.64807088834312));
#40869=CARTESIAN_POINT('',(9.18485099360515E-16,-7.5,5.64807088834312));
#40870=CARTESIAN_POINT('Origin',(0.,2.23156441938368E-15,5.64807088834312));
#40871=CARTESIAN_POINT('',(-9.35971273077467E-16,-7.64278544417155,5.99278544417156));
#40872=CARTESIAN_POINT('Origin',(9.78186630818948E-16,-7.9875,5.64807088834312));
#40873=CARTESIAN_POINT('Origin',(0.,2.2948874559959E-15,5.99278544417156));
#40874=CARTESIAN_POINT('Origin',(0.,2.23156441938368E-15,5.64807088834312));
#40875=CARTESIAN_POINT('Origin',(0.,-9.99635681210842E-31,-6.5));
#40876=CARTESIAN_POINT('',(-9.98087141305092E-16,8.14999999999999,-6.50000000000001));
#40877=CARTESIAN_POINT('',(9.98087141305092E-16,8.14999999999999,-6.5));
#40878=CARTESIAN_POINT('Origin',(0.,-9.99635681210842E-31,-6.5));
#40879=CARTESIAN_POINT('Origin',(0.,0.,-6.5));
#40880=CARTESIAN_POINT('',(-9.18485099360515E-16,7.5,-6.5));
#40881=CARTESIAN_POINT('Origin',(0.,2.26865819542047E-15,5.85));
#40882=CARTESIAN_POINT('',(-9.98087141305091E-16,-8.14999999999998,6.50000000000001));
#40883=CARTESIAN_POINT('',(9.18485099360515E-16,-7.5,5.85));
#40884=CARTESIAN_POINT('Origin',(0.,2.38806125833734E-15,6.50000000000001));
#40885=CARTESIAN_POINT('Origin',(0.,0.,-6.5));
#40886=CARTESIAN_POINT('',(-1.52656933693714E-15,12.4653846153846,6.50000000000001));
#40887=CARTESIAN_POINT('Origin',(0.,2.38806125833734E-15,6.50000000000001));
#40888=CARTESIAN_POINT('',(-1.52656933693714E-15,12.4653846153846,-6.5));
#40889=CARTESIAN_POINT('Origin',(0.,0.,-6.5));
#40890=CARTESIAN_POINT('',(-1.52656933693714E-15,12.4653846153846,-6.50000000000001));
#40891=CARTESIAN_POINT('',(-1.52656933693714E-15,12.4653846153846,-6.5));
#40892=CARTESIAN_POINT('Origin',(0.,-1.17267830746035E-30,-6.50000000000001));
#40893=CARTESIAN_POINT('Origin',(0.,8.14999999999999,-6.50000000000001));
#40894=CARTESIAN_POINT('Origin',(0.,8.14999999999999,6.50000000000001));
#40895=CARTESIAN_POINT('Origin',(0.,14.25,4.07195060716495E-15));
#40896=CARTESIAN_POINT('',(-3.56616156686793,14.25,4.07195060716495E-15));
#40897=CARTESIAN_POINT('',(3.56616156686793,14.25,4.07195060716495E-15));
#40898=CARTESIAN_POINT('Origin',(0.,14.25,4.07195060716495E-15));
#40899=CARTESIAN_POINT('Origin',(11.1410986251694,8.88472967648693,5.05753477640253E-15));
#40900=CARTESIAN_POINT('',(8.91763325644669,11.6728670610318,4.54536224786764E-15));
#40901=CARTESIAN_POINT('',(13.3645639938921,6.09659229194206,5.56970730493742E-15));
#40902=CARTESIAN_POINT('Origin',(11.1410986251694,8.88472967648693,5.05753477640253E-15));
#40903=CARTESIAN_POINT('Origin',(13.892722748591,-3.17092330887753,7.27212230242621E-15));
#40904=CARTESIAN_POINT('',(14.6862683510896,0.305827142012077,6.6334536057588E-15));
#40905=CARTESIAN_POINT('',(13.0991771460924,-6.64767375976714,7.91079099909362E-15));
#40906=CARTESIAN_POINT('Origin',(13.892722748591,-3.17092330887753,7.27212230242621E-15));
#40907=CARTESIAN_POINT('Origin',(6.18284328242512,-12.8388063676095,9.04808360878726E-15));
#40908=CARTESIAN_POINT('',(9.39584383208325,-11.2915068526795,8.76384929904507E-15));
#40909=CARTESIAN_POINT('',(2.96984273276699,-14.3861058825395,9.33231791852945E-15));
#40910=CARTESIAN_POINT('Origin',(6.18284328242512,-12.8388063676095,9.04808360878726E-15));
#40911=CARTESIAN_POINT('Origin',(-6.1828432824253,-12.8388063676094,9.04808360878725E-15));
#40912=CARTESIAN_POINT('',(-2.9698427327672,-14.3861058825394,9.33231791852944E-15));
#40913=CARTESIAN_POINT('',(-9.39584383208341,-11.2915068526794,8.76384929904506E-15));
#40914=CARTESIAN_POINT('Origin',(-6.1828432824253,-12.8388063676094,9.04808360878725E-15));
#40915=CARTESIAN_POINT('Origin',(-13.892722748591,-3.17092330887735,7.27212230242617E-15));
#40916=CARTESIAN_POINT('',(-13.0991771460925,-6.64767375976697,7.91079099909359E-15));
#40917=CARTESIAN_POINT('',(-14.6862683510895,0.30582714201227,6.63345360575876E-15));
#40918=CARTESIAN_POINT('Origin',(-13.892722748591,-3.17092330887735,7.27212230242617E-15));
#40919=CARTESIAN_POINT('Origin',(-11.1410986251693,8.88472967648709,5.0575347764025E-15));
#40920=CARTESIAN_POINT('',(-13.3645639938921,6.09659229194225,5.56970730493739E-15));
#40921=CARTESIAN_POINT('',(-8.91763325644655,11.6728670610319,4.54536224786761E-15));
#40922=CARTESIAN_POINT('Origin',(-11.1410986251693,8.88472967648709,5.0575347764025E-15));
#40923=CARTESIAN_POINT('Origin',(0.,1.07462756625201E-17,-6.44149999999999));
#40924=CARTESIAN_POINT('',(-1.99949495950787E-15,-16.3271153846154,-6.49999999999999));
#40925=CARTESIAN_POINT('Origin',(0.,2.01169401222323E-30,-6.49999999999999));
#40926=CARTESIAN_POINT('',(1.99233077573286E-15,-16.2686153846154,-6.44149999999999));
#40927=CARTESIAN_POINT('Origin',(1.99949495950788E-15,-16.3271153846154,
-6.44149999999999));
#40928=CARTESIAN_POINT('',(1.99233077573286E-15,16.2686153846154,-6.44149999999999));
#40929=CARTESIAN_POINT('Origin',(0.,1.07462756625199E-17,-6.44149999999999));
#40930=CARTESIAN_POINT('Origin',(0.,1.07462756625199E-17,-6.44149999999999));
#40931=CARTESIAN_POINT('Origin',(0.,1.30149338579385E-16,-5.7915));
#40932=CARTESIAN_POINT('',(-1.96367404063281E-15,16.0346153846154,-5.7915));
#40933=CARTESIAN_POINT('Origin',(0.,1.30149338579385E-16,-5.7915));
#40934=CARTESIAN_POINT('',(-1.97083822440782E-15,16.0931153846154,-5.85));
#40935=CARTESIAN_POINT('Origin',(1.97083822440783E-15,16.0931153846154,
-5.7915));
#40936=CARTESIAN_POINT('Origin',(0.,1.19403062916867E-16,-5.85));
#40937=CARTESIAN_POINT('Origin',(0.,2.37731498267482E-15,6.44150000000001));
#40938=CARTESIAN_POINT('',(-1.99949495950787E-15,16.3271153846154,6.5));
#40939=CARTESIAN_POINT('Origin',(0.,2.38806125833734E-15,6.50000000000001));
#40940=CARTESIAN_POINT('',(-1.99233077573286E-15,16.2686153846154,6.4415));
#40941=CARTESIAN_POINT('Origin',(1.99949495950788E-15,16.3271153846154,
6.44150000000001));
#40942=CARTESIAN_POINT('Origin',(0.,2.37731498267482E-15,6.44150000000001));
#40943=CARTESIAN_POINT('Origin',(0.,2.25791191975795E-15,5.7915));
#40944=CARTESIAN_POINT('',(1.96367404063281E-15,16.0346153846154,5.7915));
#40945=CARTESIAN_POINT('',(1.96367404063282E-15,-16.0346153846154,5.7915));
#40946=CARTESIAN_POINT('Origin',(0.,2.25791191975795E-15,5.7915));
#40947=CARTESIAN_POINT('',(-1.97083822440782E-15,-16.0931153846154,5.85000000000001));
#40948=CARTESIAN_POINT('Origin',(1.97083822440783E-15,-16.0931153846154,
5.7915));
#40949=CARTESIAN_POINT('Origin',(0.,2.26865819542047E-15,5.85));
#40950=CARTESIAN_POINT('Origin',(0.,2.25791191975795E-15,5.7915));
#40951=CARTESIAN_POINT('Origin',(0.,0.,-6.5));
#40952=CARTESIAN_POINT('',(-2.16636878649169E-15,17.6897435897436,-6.084));
#40953=CARTESIAN_POINT('Origin',(0.,7.6417960266795E-17,-6.084));
#40954=CARTESIAN_POINT('',(-2.16636878649169E-15,17.6897435897436,-5.85));
#40955=CARTESIAN_POINT('',(-2.16636878649169E-15,17.6897435897436,-6.5));
#40956=CARTESIAN_POINT('Origin',(0.,1.19403062916867E-16,-5.85));
#40957=CARTESIAN_POINT('Origin',(0.,0.,-6.5));
#40958=CARTESIAN_POINT('',(-1.99233077573286E-15,16.2686153846154,-6.084));
#40959=CARTESIAN_POINT('',(-1.99233077573286E-15,16.2686153846154,-6.5));
#40960=CARTESIAN_POINT('Origin',(0.,7.6417960266795E-17,-6.084));
#40961=CARTESIAN_POINT('Origin',(0.,0.,-6.5));
#40962=CARTESIAN_POINT('',(-1.96367404063281E-15,16.0346153846154,3.0875));
#40963=CARTESIAN_POINT('Origin',(0.,1.76119517802379E-15,3.08750000000001));
#40964=CARTESIAN_POINT('',(-1.96367404063282E-15,16.0346153846154,-6.5));
#40965=CARTESIAN_POINT('Origin',(0.,1.73472347597681E-15,6.67403582113016E-15));
#40966=CARTESIAN_POINT('',(-1.96367404063281E-15,16.0346153846154,-3.0875));
#40967=CARTESIAN_POINT('Origin',(1.74512168878498E-15,14.25,4.05635328795269E-15));
#40968=CARTESIAN_POINT('Origin',(0.,6.26866080313552E-16,-3.08749999999999));
#40969=CARTESIAN_POINT('Origin',(0.,0.,-6.5));
#40970=CARTESIAN_POINT('',(-1.96367404063282E-15,16.0346153846154,-6.5));
#40971=CARTESIAN_POINT('Origin',(0.,0.,-6.5));
#40972=CARTESIAN_POINT('',(-1.99233077573286E-15,16.2686153846154,6.084));
#40973=CARTESIAN_POINT('Origin',(0.,2.31164329807054E-15,6.084));
#40974=CARTESIAN_POINT('',(-1.99233077573286E-15,16.2686153846154,-6.5));
#40975=CARTESIAN_POINT('Origin',(0.,0.,-6.5));
#40976=CARTESIAN_POINT('',(-2.16636878649169E-15,17.6897435897436,5.85));
#40977=CARTESIAN_POINT('Origin',(0.,2.26865819542047E-15,5.85));
#40978=CARTESIAN_POINT('',(-2.16636878649169E-15,17.6897435897436,6.084));
#40979=CARTESIAN_POINT('',(-2.16636878649169E-15,17.6897435897436,-6.5));
#40980=CARTESIAN_POINT('Origin',(0.,2.31164329807054E-15,6.084));
#40981=CARTESIAN_POINT('Origin',(0.,2.38806125833734E-15,6.50000000000001));
#40982=CARTESIAN_POINT('',(-2.57175827820944E-15,21.,5.85));
#40983=CARTESIAN_POINT('Origin',(0.,2.26865819542047E-15,5.85000000000001));
#40984=CARTESIAN_POINT('',(-2.49215623626487E-15,20.35,6.5));
#40985=CARTESIAN_POINT('',(2.49215623626486E-15,20.35,6.50000000000001));
#40986=CARTESIAN_POINT('Origin',(0.,2.38806125833734E-15,6.50000000000001));
#40987=CARTESIAN_POINT('Origin',(0.,1.19403062916869E-16,-5.84999999999999));
#40988=CARTESIAN_POINT('',(2.57175827820944E-15,21.,-5.84999999999999));
#40989=CARTESIAN_POINT('',(2.57175827820944E-15,-21.,-5.84999999999999));
#40990=CARTESIAN_POINT('Origin',(0.,1.19403062916869E-16,-5.84999999999999));
#40991=CARTESIAN_POINT('Origin',(0.,1.19403062916869E-16,-5.84999999999999));
#40992=CARTESIAN_POINT('',(-2.49215623626487E-15,-20.35,-6.49999999999999));
#40993=CARTESIAN_POINT('',(2.57175827820944E-15,-21.,-5.84999999999999));
#40994=CARTESIAN_POINT('Origin',(0.,1.96135664184276E-30,-6.49999999999999));
#40995=CARTESIAN_POINT('Origin',(0.,0.,-6.5));
#40996=CARTESIAN_POINT('',(-2.57175827820944E-15,21.,-6.5));
#40997=CARTESIAN_POINT('Origin',(0.,20.35,-6.49999999999999));
#40998=CARTESIAN_POINT('Origin',(0.,20.35,6.5));
#40999=CARTESIAN_POINT('Origin',(0.,16.0346153846154,5.85));
#41000=CARTESIAN_POINT('Origin',(0.,16.2686153846154,6.084));
#41001=CARTESIAN_POINT('Origin',(0.,16.2686153846154,-6.084));
#41002=CARTESIAN_POINT('Origin',(0.,16.0346153846154,-5.85));
#41003=CARTESIAN_POINT('Origin',(-11.1410986251694,8.88472967648693,9.85584169237584E-16));
#41004=CARTESIAN_POINT('',(-11.838732871064,9.44107442276088,3.96060240207311));
#41005=CARTESIAN_POINT('Origin',(-11.838732871064,9.44107442276088,1.04729956121144E-15));
#41006=CARTESIAN_POINT('',(-10.4434643792749,8.32838493021299,3.96060240207311));
#41007=CARTESIAN_POINT('Origin',(-11.1410986251694,8.88472967648693,2.5198520116158));
#41008=CARTESIAN_POINT('Origin',(-10.4434643792749,8.32838493021299,9.23868777263733E-16));
#41009=CARTESIAN_POINT('',(-13.176267261227,5.42664547033602,-1.08333333333333));
#41010=CARTESIAN_POINT('',(-13.9269936544441,5.94376395877182,-1.08333333333333));
#41011=CARTESIAN_POINT('Ctrl Pts',(-13.176267261227,5.42664547033603,-1.08333333333333));
#41012=CARTESIAN_POINT('Ctrl Pts',(-13.3544742809805,5.48608062863209,-1.08333333333333));
#41013=CARTESIAN_POINT('Ctrl Pts',(-13.5395781511317,5.58798093945111,-1.08333333333333));
#41014=CARTESIAN_POINT('Ctrl Pts',(-13.7657237213497,5.76832601371359,-1.08333333333333));
#41015=CARTESIAN_POINT('Ctrl Pts',(-13.851789663848,5.85187873682469,-1.08333333333333));
#41016=CARTESIAN_POINT('Ctrl Pts',(-13.9269936544446,5.9437639587714,-1.08333333333333));
#41017=CARTESIAN_POINT('',(-13.9269936544455,5.94376395877242,1.08333333333333));
#41018=CARTESIAN_POINT('Ctrl Pts',(-13.9269936544444,5.94376395877114,1.08333333333355));
#41019=CARTESIAN_POINT('Ctrl Pts',(-13.9416885168396,5.90933203032471,0.95688863210348));
#41020=CARTESIAN_POINT('Ctrl Pts',(-13.9536527109306,5.88095561854246,0.828820583351296));
#41021=CARTESIAN_POINT('Ctrl Pts',(-13.9629765258054,5.85873440158612,0.699646919261824));
#41022=CARTESIAN_POINT('Ctrl Pts',(-13.9722513158078,5.83663002439321,0.571152453813156));
#41023=CARTESIAN_POINT('Ctrl Pts',(-13.9789135007646,5.82061622745832,0.441563969171476));
#41024=CARTESIAN_POINT('Ctrl Pts',(-13.9830050237945,5.81077040959789,0.311391073637591));
#41025=CARTESIAN_POINT('Ctrl Pts',(-13.9870637119681,5.80100360534983,0.182262827807202));
#41026=CARTESIAN_POINT('Ctrl Pts',(-13.9885928700523,5.79730615639837,0.0525595133518154));
#41027=CARTESIAN_POINT('Ctrl Pts',(-13.9875862925321,5.79973378332902,-0.0772214321948836));
#41028=CARTESIAN_POINT('Ctrl Pts',(-13.9868997670034,5.80138952054624,-0.16573715053464));
#41029=CARTESIAN_POINT('Ctrl Pts',(-13.9850326975558,5.80589410253377,-0.25428898113034));
#41030=CARTESIAN_POINT('Ctrl Pts',(-13.9819702480149,5.81325986277477,-0.342719102199523));
#41031=CARTESIAN_POINT('Ctrl Pts',(-13.9773533484511,5.82436436418404,-0.476034927301742));
#41032=CARTESIAN_POINT('Ctrl Pts',(-13.9700489046451,5.84190742581559,-0.608312350205735));
#41033=CARTESIAN_POINT('Ctrl Pts',(-13.9600480872369,5.86570879353503,-0.739057191237609));
#41034=CARTESIAN_POINT('Ctrl Pts',(-13.9511688384278,5.8868408927778,-0.855139299994326));
#41035=CARTESIAN_POINT('Ctrl Pts',(-13.9401632237806,5.9129059856334,-0.970013302477931));
#41036=CARTESIAN_POINT('Ctrl Pts',(-13.9269936544444,5.94376395877114,-1.08333333333355));
#41037=CARTESIAN_POINT('',(-13.176267261227,5.42664547033602,1.08333333333333));
#41038=CARTESIAN_POINT('Ctrl Pts',(-13.176267261227,5.42664547033603,1.08333333333333));
#41039=CARTESIAN_POINT('Ctrl Pts',(-13.3544742809805,5.48608062863209,1.08333333333333));
#41040=CARTESIAN_POINT('Ctrl Pts',(-13.5395781511317,5.58798093945111,1.08333333333333));
#41041=CARTESIAN_POINT('Ctrl Pts',(-13.76572372135,5.76832601371385,1.08333333333333));
#41042=CARTESIAN_POINT('Ctrl Pts',(-13.8517896638487,5.85187873682532,1.08333333333333));
#41043=CARTESIAN_POINT('Ctrl Pts',(-13.9269936544455,5.94376395877245,1.08333333333333));
#41044=CARTESIAN_POINT('Ctrl Pts',(-13.176267261227,5.426645470336,-1.08333333333333));
#41045=CARTESIAN_POINT('Ctrl Pts',(-13.1893705593041,5.39482976422217,-0.949270311030458));
#41046=CARTESIAN_POINT('Ctrl Pts',(-13.1999097963793,5.36892368585873,-0.813521288367943));
#41047=CARTESIAN_POINT('Ctrl Pts',(-13.2079621630869,5.34904061477063,-0.676607052100963));
#41048=CARTESIAN_POINT('Ctrl Pts',(-13.2148460430323,5.33204279546006,-0.559560573777783));
#41049=CARTESIAN_POINT('Ctrl Pts',(-13.2199117356377,5.31944645364942,-0.441662516279014));
#41050=CARTESIAN_POINT('Ctrl Pts',(-13.2231796369648,5.31131059989529,-0.323238258334693));
#41051=CARTESIAN_POINT('Ctrl Pts',(-13.2269557156994,5.30190957419894,-0.186398348762648));
#41052=CARTESIAN_POINT('Ctrl Pts',(-13.2283213471704,5.29849241313602,-0.0492519096262365));
#41053=CARTESIAN_POINT('Ctrl Pts',(-13.2273014856384,5.30103720115478,0.0876758270660023));
#41054=CARTESIAN_POINT('Ctrl Pts',(-13.2262786675027,5.30358936657696,0.225000520654269));
#41055=CARTESIAN_POINT('Ctrl Pts',(-13.2228564747501,5.31213809759637,0.362105241912721));
#41056=CARTESIAN_POINT('Ctrl Pts',(-13.21701132539,5.32664168351063,0.498460177595569));
#41057=CARTESIAN_POINT('Ctrl Pts',(-13.2111409592134,5.34120783998416,0.635403368116636));
#41058=CARTESIAN_POINT('Ctrl Pts',(-13.2028266475275,5.36178038996277,0.771590289741212));
#41059=CARTESIAN_POINT('Ctrl Pts',(-13.1919958930595,5.38829698119001,0.90648424252654));
#41060=CARTESIAN_POINT('Ctrl Pts',(-13.1872415508606,5.39993688577963,0.965698216399817));
#41061=CARTESIAN_POINT('Ctrl Pts',(-13.1820016856382,5.4127218947045,1.02466304565395));
#41062=CARTESIAN_POINT('Ctrl Pts',(-13.176267261227,5.426645470336,1.08333333333333));
#41063=CARTESIAN_POINT('',(-8.89378902201695,12.2552029391753,-1.08333333333333));
#41064=CARTESIAN_POINT('',(-8.22258343557141,11.6383685130291,-1.08333333333333));
#41065=CARTESIAN_POINT('Ctrl Pts',(-8.89378902201693,12.2552029391753,-1.08333333333333));
#41066=CARTESIAN_POINT('Ctrl Pts',(-8.78747309219938,12.2023308550396,-1.08333333333333));
#41067=CARTESIAN_POINT('Ctrl Pts',(-8.68686373639314,12.1370149953911,-1.08333333333333));
#41068=CARTESIAN_POINT('Ctrl Pts',(-8.46071816617524,11.9566699211287,-1.08333333333333));
#41069=CARTESIAN_POINT('Ctrl Pts',(-8.32018322283281,11.7988819437994,-1.08333333333333));
#41070=CARTESIAN_POINT('Ctrl Pts',(-8.22258343557192,11.6383685130288,-1.08333333333333));
#41071=CARTESIAN_POINT('',(-8.22258343557665,11.6383685130365,1.08333333333333));
#41072=CARTESIAN_POINT('Ctrl Pts',(-8.22258343557191,11.6383685130287,1.08333333333318));
#41073=CARTESIAN_POINT('Ctrl Pts',(-8.19455490688727,11.6581708517696,0.949622058007629));
#41074=CARTESIAN_POINT('Ctrl Pts',(-8.17172113698899,11.6741565633286,0.814376693553349));
#41075=CARTESIAN_POINT('Ctrl Pts',(-8.15417398891324,11.6864000683928,0.678132403728345));
#41076=CARTESIAN_POINT('Ctrl Pts',(-8.13671023659264,11.698585384152,0.542535637671064));
#41077=CARTESIAN_POINT('Ctrl Pts',(-8.12448291951145,11.7070640382822,0.405949418799179));
#41078=CARTESIAN_POINT('Ctrl Pts',(-8.11755242812626,11.7118675955896,0.268901316712111));
#41079=CARTESIAN_POINT('Ctrl Pts',(-8.11302715126356,11.7150040870061,0.179415511018989));
#41080=CARTESIAN_POINT('Ctrl Pts',(-8.11075954642953,11.7165728598427,0.0897327832367744));
#41081=CARTESIAN_POINT('Ctrl Pts',(-8.11075954642953,11.7165728598427,9.99200722162641E-15));
#41082=CARTESIAN_POINT('Ctrl Pts',(-8.11075954642954,11.7165728598427,-0.137573936980354));
#41083=CARTESIAN_POINT('Ctrl Pts',(-8.11609005089583,11.7128881555246,-0.274951212619692));
#41084=CARTESIAN_POINT('Ctrl Pts',(-8.12669452775723,11.7055258768037,-0.4116124062147));
#41085=CARTESIAN_POINT('Ctrl Pts',(-8.13738105388554,11.6981066344457,-0.549330978772881));
#41086=CARTESIAN_POINT('Ctrl Pts',(-8.15342350530942,11.6869526399855,-0.686322345437031));
#41087=CARTESIAN_POINT('Ctrl Pts',(-8.17473347641523,11.6720277839618,-0.822054935347404));
#41088=CARTESIAN_POINT('Ctrl Pts',(-8.18849695174643,11.662388264195,-0.909720570537357));
#41089=CARTESIAN_POINT('Ctrl Pts',(-8.20445714658991,11.6511748546878,-0.996861109122827));
#41090=CARTESIAN_POINT('Ctrl Pts',(-8.22258343557191,11.6383685130287,-1.08333333333318));
#41091=CARTESIAN_POINT('',(-8.89378902201695,12.2552029391753,1.08333333333333));
#41092=CARTESIAN_POINT('Ctrl Pts',(-8.89378902201693,12.2552029391753,1.08333333333333));
#41093=CARTESIAN_POINT('Ctrl Pts',(-8.78747309219938,12.2023308550396,1.08333333333333));
#41094=CARTESIAN_POINT('Ctrl Pts',(-8.68686373639314,12.1370149953911,1.08333333333333));
#41095=CARTESIAN_POINT('Ctrl Pts',(-8.46071816617751,11.9566699211305,1.08333333333333));
#41096=CARTESIAN_POINT('Ctrl Pts',(-8.32018322283717,11.7988819438045,1.08333333333333));
#41097=CARTESIAN_POINT('Ctrl Pts',(-8.22258343557662,11.6383685130365,1.08333333333333));
#41098=CARTESIAN_POINT('Ctrl Pts',(-8.89378902201696,12.2552029391753,-1.08333333333333));
#41099=CARTESIAN_POINT('Ctrl Pts',(-8.86325700199161,12.2773604951023,-0.955915065626613));
#41100=CARTESIAN_POINT('Ctrl Pts',(-8.83806624000395,12.2954729083691,-0.8267015714506));
#41101=CARTESIAN_POINT('Ctrl Pts',(-8.81837639229442,12.3095783864577,-0.696211209492237));
#41102=CARTESIAN_POINT('Ctrl Pts',(-8.79899689851553,12.3234615321731,-0.567777653525536));
#41103=CARTESIAN_POINT('Ctrl Pts',(-8.7849462329058,12.3334631509294,-0.438107164856251));
#41104=CARTESIAN_POINT('Ctrl Pts',(-8.77634666705863,12.3395794672318,-0.307693975181527));
#41105=CARTESIAN_POINT('Ctrl Pts',(-8.76960830208466,12.3443720314467,-0.205506064179221));
#41106=CARTESIAN_POINT('Ctrl Pts',(-8.76621624622179,12.3467783236356,-0.102862147741002));
#41107=CARTESIAN_POINT('Ctrl Pts',(-8.76621624622179,12.3467783236356,2.44249065417534E-15));
#41108=CARTESIAN_POINT('Ctrl Pts',(-8.76621624622179,12.3467783236356,0.130666807305558));
#41109=CARTESIAN_POINT('Ctrl Pts',(-8.77169236507929,12.3428956683044,0.261069786498707));
#41110=CARTESIAN_POINT('Ctrl Pts',(-8.78256611126601,12.3351536167882,0.390710450871087));
#41111=CARTESIAN_POINT('Ctrl Pts',(-8.79357042167237,12.3273186042172,0.521907748246256));
#41112=CARTESIAN_POINT('Ctrl Pts',(-8.8101027782242,12.315530900308,0.652324314224256));
#41113=CARTESIAN_POINT('Ctrl Pts',(-8.83205039902736,12.2997710546807,0.781443489202971));
#41114=CARTESIAN_POINT('Ctrl Pts',(-8.84930597782606,12.2873804060307,0.882959098491573));
#41115=CARTESIAN_POINT('Ctrl Pts',(-8.86990830867396,12.2725335396739,0.983672743459536));
#41116=CARTESIAN_POINT('Ctrl Pts',(-8.89378902201696,12.2552029391753,1.08333333333333));
#41117=CARTESIAN_POINT('Origin',(-11.1410986251694,8.88472967648693,9.85584169237584E-16));
#41118=CARTESIAN_POINT('',(-13.6377879061429,6.58029051604744,1.08333333333333));
#41119=CARTESIAN_POINT('',(-13.2594869773434,6.22835470309403,1.08333333333333));
#41120=CARTESIAN_POINT('Origin',(-11.1410986251694,8.88472967648693,1.08333333333333));
#41121=CARTESIAN_POINT('',(-13.6377879061429,6.58029051604744,-1.08333333333333));
#41122=CARTESIAN_POINT('Ctrl Pts',(-13.6377879061429,6.58029051604746,-1.08333333333332));
#41123=CARTESIAN_POINT('Ctrl Pts',(-13.6907677796516,6.47048863474076,-0.727666221822785));
#41124=CARTESIAN_POINT('Ctrl Pts',(-13.7154355939007,6.41687686636447,-0.35278297384277));
#41125=CARTESIAN_POINT('Ctrl Pts',(-13.7154355939007,6.41687686636447,0.352782973842772));
#41126=CARTESIAN_POINT('Ctrl Pts',(-13.6907677796516,6.47048863474076,0.727666221822785));
#41127=CARTESIAN_POINT('Ctrl Pts',(-13.6377879061429,6.58029051604746,1.08333333333332));
#41128=CARTESIAN_POINT('',(-12.9276994994136,5.99475484510091,-1.08333333333333));
#41129=CARTESIAN_POINT('Origin',(-11.1410986251694,8.88472967648693,-1.08333333333333));
#41130=CARTESIAN_POINT('',(-12.9276994994136,5.99475484510091,1.08333333333333));
#41131=CARTESIAN_POINT('Ctrl Pts',(-12.9276994994136,5.99475484510092,1.08333333333333));
#41132=CARTESIAN_POINT('Ctrl Pts',(-12.9759843593574,5.89062845864246,0.725928647976576));
#41133=CARTESIAN_POINT('Ctrl Pts',(-12.9982133898606,5.84028669430256,0.352039859176989));
#41134=CARTESIAN_POINT('Ctrl Pts',(-12.9982133898606,5.84028669430256,-0.352039859176986));
#41135=CARTESIAN_POINT('Ctrl Pts',(-12.9759843593574,5.89062845864246,-0.725928647976575));
#41136=CARTESIAN_POINT('Ctrl Pts',(-12.9276994994136,5.99475484510092,-1.08333333333332));
#41137=CARTESIAN_POINT('Origin',(-11.1410986251694,8.88472967648693,1.08333333333333));
#41138=CARTESIAN_POINT('',(-9.02271027299537,11.5411046498798,1.08333333333333));
#41139=CARTESIAN_POINT('Origin',(-11.1410986251694,8.88472967648693,9.85584169237584E-16));
#41140=CARTESIAN_POINT('',(-8.72113759169224,11.2696166353063,1.08333333333333));
#41141=CARTESIAN_POINT('Origin',(-11.1410986251694,8.88472967648693,1.08333333333333));
#41142=CARTESIAN_POINT('',(-8.72113759169224,11.2696166353063,-1.08333333333333));
#41143=CARTESIAN_POINT('Ctrl Pts',(-8.72113759169222,11.2696166353063,-1.08333333333334));
#41144=CARTESIAN_POINT('Ctrl Pts',(-8.63036626326988,11.3398611937656,-0.725928647976585));
#41145=CARTESIAN_POINT('Ctrl Pts',(-8.58623309669495,11.3727349924818,-0.352039859176991));
#41146=CARTESIAN_POINT('Ctrl Pts',(-8.58623309669495,11.3727349924818,4.46574186955748E-16));
#41147=CARTESIAN_POINT('Ctrl Pts',(-8.58623309669495,11.3727349924818,0.352039859176991));
#41148=CARTESIAN_POINT('Ctrl Pts',(-8.63036626326988,11.3398611937656,0.725928647976585));
#41149=CARTESIAN_POINT('Ctrl Pts',(-8.72113759169222,11.2696166353063,1.08333333333334));
#41150=CARTESIAN_POINT('',(-9.45000219633307,11.8316076987796,-1.08333333333333));
#41151=CARTESIAN_POINT('Origin',(-11.1410986251694,8.88472967648693,-1.08333333333333));
#41152=CARTESIAN_POINT('',(-9.45000219633307,11.8316076987796,1.08333333333333));
#41153=CARTESIAN_POINT('Ctrl Pts',(-9.45000219633306,11.8316076987796,1.08333333333334));
#41154=CARTESIAN_POINT('Ctrl Pts',(-9.35474240837113,11.9076924734257,0.727666221822798));
#41155=CARTESIAN_POINT('Ctrl Pts',(-9.30796390402501,11.9436715548398,0.352782973842778));
#41156=CARTESIAN_POINT('Ctrl Pts',(-9.30796390402501,11.9436715548398,5.10741104345864E-16));
#41157=CARTESIAN_POINT('Ctrl Pts',(-9.30796390402501,11.9436715548398,-0.352782973842777));
#41158=CARTESIAN_POINT('Ctrl Pts',(-9.35474240837113,11.9076924734257,-0.727666221822798));
#41159=CARTESIAN_POINT('Ctrl Pts',(-9.45000219633306,11.8316076987796,-1.08333333333334));
#41160=CARTESIAN_POINT('Origin',(-11.1410986251694,8.88472967648693,1.08333333333333));
#41161=CARTESIAN_POINT('',(-10.4434643792749,8.32838493021299,-3.45272288248773));
#41162=CARTESIAN_POINT('Origin',(-10.4434643792749,8.32838493021299,9.23868777263733E-16));
#41163=CARTESIAN_POINT('',(-11.838732871064,9.44107442276088,-3.45272288248773));
#41164=CARTESIAN_POINT('Origin',(-11.838732871064,9.44107442276088,1.04729956121144E-15));
#41165=CARTESIAN_POINT('Origin',(-13.892722748591,-3.17092330887753,3.20017169526126E-15));
#41166=CARTESIAN_POINT('',(-14.7626584240763,-3.36948044994625,3.96060240207311));
#41167=CARTESIAN_POINT('Origin',(-14.7626584240763,-3.36948044994625,3.40056031423578E-15));
#41168=CARTESIAN_POINT('',(-13.0227870731057,-2.97236616780882,3.96060240207311));
#41169=CARTESIAN_POINT('Origin',(-13.892722748591,-3.17092330887753,2.5198520116158));
#41170=CARTESIAN_POINT('Origin',(-13.0227870731057,-2.97236616780882,2.99978307628674E-15));
#41171=CARTESIAN_POINT('',(-12.4579905368413,-6.91816245718267,-1.08333333333333));
#41172=CARTESIAN_POINT('',(-13.3303603014234,-7.18268588222789,-1.08333333333333));
#41173=CARTESIAN_POINT('Ctrl Pts',(-12.4579905368413,-6.91816245718265,
-1.08333333333333));
#41174=CARTESIAN_POINT('Ctrl Pts',(-12.6155690741986,-7.02043310055334,
-1.08333333333333));
#41175=CARTESIAN_POINT('Ctrl Pts',(-12.8106483205941,-7.10161932916232,
-1.08333333333333));
#41176=CARTESIAN_POINT('Ctrl Pts',(-13.0926472341269,-7.16598374096129,
-1.08333333333333));
#41177=CARTESIAN_POINT('Ctrl Pts',(-13.211632620936,-7.18117853359748,-1.08333333333333));
#41178=CARTESIAN_POINT('Ctrl Pts',(-13.3303603014234,-7.18268588222786,
-1.08333333333333));
#41179=CARTESIAN_POINT('',(-13.3303603014234,-7.18268588222787,1.08333333333334));
#41180=CARTESIAN_POINT('Ctrl Pts',(-13.3303603014234,-7.18268588222788,
1.08333333333333));
#41181=CARTESIAN_POINT('Ctrl Pts',(-13.312602432605,-7.21564274452362,0.9568886321034));
#41182=CARTESIAN_POINT('Ctrl Pts',(-13.2978764135175,-7.24268913148589,
0.828820583351364));
#41183=CARTESIAN_POINT('Ctrl Pts',(-13.2863164700111,-7.26383348564883,
0.699646919262042));
#41184=CARTESIAN_POINT('Ctrl Pts',(-13.2748173090022,-7.28486666222222,
0.571152453813466));
#41185=CARTESIAN_POINT('Ctrl Pts',(-13.2664510227833,-7.30005980724142,
0.441563969171881));
#41186=CARTESIAN_POINT('Ctrl Pts',(-13.2613042752926,-7.30939745578436,
0.311391073638092));
#41187=CARTESIAN_POINT('Ctrl Pts',(-13.2561988309335,-7.3186601688214,0.182262827807686));
#41188=CARTESIAN_POINT('Ctrl Pts',(-13.2542614634094,-7.32216103446744,
0.0525595133522827));
#41189=CARTESIAN_POINT('Ctrl Pts',(-13.2555318677528,-7.31986045983868,
-0.0772214321944347));
#41190=CARTESIAN_POINT('Ctrl Pts',(-13.2563983335701,-7.31829137729732,
-0.165737150534351));
#41191=CARTESIAN_POINT('Ctrl Pts',(-13.2587560588234,-7.31402308269238,
-0.254288981130211));
#41192=CARTESIAN_POINT('Ctrl Pts',(-13.2626054360146,-7.30703628683457,
-0.342719102199554));
#41193=CARTESIAN_POINT('Ctrl Pts',(-13.2684086950193,-7.29650310602083,
-0.476034927301584));
#41194=CARTESIAN_POINT('Ctrl Pts',(-13.2775701666804,-7.27985434187078,
-0.608312350205395));
#41195=CARTESIAN_POINT('Ctrl Pts',(-13.2899434176249,-7.25719547792734,
-0.739057191237093));
#41196=CARTESIAN_POINT('Ctrl Pts',(-13.3009290370229,-7.23707775329796,
-0.855139299993907));
#41197=CARTESIAN_POINT('Ctrl Pts',(-13.3144456587151,-7.21222189770289,
-0.970013302477609));
#41198=CARTESIAN_POINT('Ctrl Pts',(-13.3303603014234,-7.18268588222788,
-1.08333333333332));
#41199=CARTESIAN_POINT('',(-12.4579905368413,-6.91816245718267,1.08333333333334));
#41200=CARTESIAN_POINT('Ctrl Pts',(-12.4579905368413,-6.91816245718265,
1.08333333333333));
#41201=CARTESIAN_POINT('Ctrl Pts',(-12.6150882655077,-7.02012104908378,
1.08333333333333));
#41202=CARTESIAN_POINT('Ctrl Pts',(-12.8106174809568,-7.10161229021636,
1.08333333333333));
#41203=CARTESIAN_POINT('Ctrl Pts',(-13.0925863122299,-7.16596983593587,
1.08333333333333));
#41204=CARTESIAN_POINT('Ctrl Pts',(-13.2116839714656,-7.18117918553602,
1.08333333333333));
#41205=CARTESIAN_POINT('Ctrl Pts',(-13.3303603014234,-7.18268588222786,
1.08333333333333));
#41206=CARTESIAN_POINT('Ctrl Pts',(-12.4579905368413,-6.91816245718269,
-1.08333333333333));
#41207=CARTESIAN_POINT('Ctrl Pts',(-12.4412857888864,-6.94824379644449,
-0.949270311030495));
#41208=CARTESIAN_POINT('Ctrl Pts',(-12.4276027080703,-6.97263587945683,
-0.813521288368019));
#41209=CARTESIAN_POINT('Ctrl Pts',(-12.4170780656485,-6.99132836531023,
-0.676607052101084));
#41210=CARTESIAN_POINT('Ctrl Pts',(-12.4080806643214,-7.0073083663671,-0.559560573777871));
#41211=CARTESIAN_POINT('Ctrl Pts',(-12.4013908554087,-7.01912257498617,
-0.441662516279072));
#41212=CARTESIAN_POINT('Ctrl Pts',(-12.3970674919579,-7.02675014497037,
-0.323238258334728));
#41213=CARTESIAN_POINT('Ctrl Pts',(-12.392071820683,-7.03556384585404,-0.186398348762656));
#41214=CARTESIAN_POINT('Ctrl Pts',(-12.3902516338786,-7.03876210460556,
-0.0492519096262199));
#41215=CARTESIAN_POINT('Ctrl Pts',(-12.3916053560034,-7.03637809537454,
0.0876758270660418));
#41216=CARTESIAN_POINT('Ctrl Pts',(-12.3929630026022,-7.03398717484178,
0.22500052065431));
#41217=CARTESIAN_POINT('Ctrl Pts',(-12.3975129673671,-7.02598155019929,
0.36210524191276));
#41218=CARTESIAN_POINT('Ctrl Pts',(-12.4052079364271,-7.0123687905019,0.498460177595606));
#41219=CARTESIAN_POINT('Ctrl Pts',(-12.4129361026924,-6.99869730339788,
0.635403368116707));
#41220=CARTESIAN_POINT('Ctrl Pts',(-12.4238364813948,-6.97937013765694,
0.771590289741313));
#41221=CARTESIAN_POINT('Ctrl Pts',(-12.4378151222667,-6.9543694886247,0.906484242526672));
#41222=CARTESIAN_POINT('Ctrl Pts',(-12.4439512822522,-6.94339503240897,
0.965698216399908));
#41223=CARTESIAN_POINT('Ctrl Pts',(-12.450680002204,-6.93132701813286,1.024663045654));
#41224=CARTESIAN_POINT('Ctrl Pts',(-12.4579905368413,-6.91816245718269,
1.08333333333334));
#41225=CARTESIAN_POINT('',(-15.1266902369927,0.68754979644356,-1.08333333333333));
#41226=CARTESIAN_POINT('',(-14.2259398250621,0.827729480997533,-1.08333333333333));
#41227=CARTESIAN_POINT('Ctrl Pts',(-15.1266902369927,0.687549796443589,
-1.08333333333333));
#41228=CARTESIAN_POINT('Ctrl Pts',(-15.0191128271494,0.737684039417719,
-1.08333333333333));
#41229=CARTESIAN_POINT('Ctrl Pts',(-14.905210454464,0.775655426636244,-1.08333333333333));
#41230=CARTESIAN_POINT('Ctrl Pts',(-14.6232416231909,0.840012972355744,
-1.08333333333333));
#41231=CARTESIAN_POINT('Ctrl Pts',(-14.411718162898,0.851428848194329,-1.08333333333333));
#41232=CARTESIAN_POINT('Ctrl Pts',(-14.2259398250622,0.827729480996923,
-1.08333333333333));
#41233=CARTESIAN_POINT('',(-14.2259398250711,0.827729480998061,1.08333333333334));
#41234=CARTESIAN_POINT('Ctrl Pts',(-14.2259398250621,0.827729480996948,
1.08333333333319));
#41235=CARTESIAN_POINT('Ctrl Pts',(-14.2239464151202,0.86198962338768,0.949622058007746));
#41236=CARTESIAN_POINT('Ctrl Pts',(-14.2222079250172,0.889808711690097,
0.814376693553578));
#41237=CARTESIAN_POINT('Ctrl Pts',(-14.2208398148552,0.911161325029729,
0.678132403728685));
#41238=CARTESIAN_POINT('Ctrl Pts',(-14.2194782068654,0.932412456504284,
0.542535637671376));
#41239=CARTESIAN_POINT('Ctrl Pts',(-14.2184834780892,0.947258512328182,
0.405949418799462));
#41240=CARTESIAN_POINT('Ctrl Pts',(-14.2179179597194,0.955671957675903,
0.268901316712362));
#41241=CARTESIAN_POINT('Ctrl Pts',(-14.2175487034788,0.961165532005871,
0.179415511019154));
#41242=CARTESIAN_POINT('Ctrl Pts',(-14.2173613909827,0.963916530719958,
0.0897327832368514));
#41243=CARTESIAN_POINT('Ctrl Pts',(-14.2173613909827,0.963916530719958,
-1.77635683940025E-15));
#41244=CARTESIAN_POINT('Ctrl Pts',(-14.2173613909827,0.963916530719959,
-0.137573936980362));
#41245=CARTESIAN_POINT('Ctrl Pts',(-14.2178040883167,0.957451598945575,
-0.274951212619699));
#41246=CARTESIAN_POINT('Ctrl Pts',(-14.2186598102071,0.944570379379332,
-0.411612406214706));
#41247=CARTESIAN_POINT('Ctrl Pts',(-14.2195221530139,0.931589494866292,
-0.549330978772852));
#41248=CARTESIAN_POINT('Ctrl Pts',(-14.2208039138492,0.912092599491199,
-0.686322345436968));
#41249=CARTESIAN_POINT('Ctrl Pts',(-14.222421741201,0.886126297665223,-0.82205493534731));
#41250=CARTESIAN_POINT('Ctrl Pts',(-14.2234666476786,0.869355437073727,
-0.909720570537294));
#41251=CARTESIAN_POINT('Ctrl Pts',(-14.2246506698206,0.849885807806941,
-0.996861109122796));
#41252=CARTESIAN_POINT('Ctrl Pts',(-14.2259398250621,0.827729480996951,
-1.08333333333318));
#41253=CARTESIAN_POINT('',(-15.1266902369927,0.687549796443561,1.08333333333334));
#41254=CARTESIAN_POINT('Ctrl Pts',(-15.1266902369927,0.687549796443589,
1.08333333333333));
#41255=CARTESIAN_POINT('Ctrl Pts',(-15.0191128271494,0.73768403941772,1.08333333333333));
#41256=CARTESIAN_POINT('Ctrl Pts',(-14.905210454464,0.775655426636245,1.08333333333333));
#41257=CARTESIAN_POINT('Ctrl Pts',(-14.6232416231937,0.840012972355103,
1.08333333333333));
#41258=CARTESIAN_POINT('Ctrl Pts',(-14.4117181629048,0.851428848194163,
1.08333333333333));
#41259=CARTESIAN_POINT('Ctrl Pts',(-14.2259398250711,0.827729480998062,
1.08333333333333));
#41260=CARTESIAN_POINT('Ctrl Pts',(-15.1266902369927,0.687549796443564,
-1.08333333333333));
#41261=CARTESIAN_POINT('Ctrl Pts',(-15.1249773086751,0.725235701077295,
-0.955915065626697));
#41262=CARTESIAN_POINT('Ctrl Pts',(-15.1234319803901,0.756223536825465,
-0.826701571450772));
#41263=CARTESIAN_POINT('Ctrl Pts',(-15.122183667988,0.780412301388329,-0.696211209492499));
#41264=CARTESIAN_POINT('Ctrl Pts',(-15.1209550316477,0.804219799510246,
-0.567777653525797));
#41265=CARTESIAN_POINT('Ctrl Pts',(-15.12001416535,0.821440959530219,-0.438107164856512));
#41266=CARTESIAN_POINT('Ctrl Pts',(-15.1194343523859,0.83197783168462,-0.307693975181787));
#41267=CARTESIAN_POINT('Ctrl Pts',(-15.1189800281283,0.840234212474348,
-0.205506064179395));
#41268=CARTESIAN_POINT('Ctrl Pts',(-15.1187464308798,0.844386527178334,
-0.102862147741089));
#41269=CARTESIAN_POINT('Ctrl Pts',(-15.1187464308798,0.844386527178334,
1.99840144432528E-15));
#41270=CARTESIAN_POINT('Ctrl Pts',(-15.1187464308798,0.844386527178334,
0.130666807305563));
#41271=CARTESIAN_POINT('Ctrl Pts',(-15.1191251529677,0.837684329050672,
0.261069786498716));
#41272=CARTESIAN_POINT('Ctrl Pts',(-15.1198518432089,0.824355801783686,
0.3907104508711));
#41273=CARTESIAN_POINT('Ctrl Pts',(-15.1205872590302,0.810867235029684,
0.521907748246278));
#41274=CARTESIAN_POINT('Ctrl Pts',(-15.1216790167187,0.790592205023353,
0.652324314224286));
#41275=CARTESIAN_POINT('Ctrl Pts',(-15.1230415909943,0.763606761086714,
0.78144348920301));
#41276=CARTESIAN_POINT('Ctrl Pts',(-15.1241128691977,0.742390363261972,
0.882959098491598));
#41277=CARTESIAN_POINT('Ctrl Pts',(-15.1253504648421,0.717025942629857,
0.983672743459549));
#41278=CARTESIAN_POINT('Ctrl Pts',(-15.1266902369927,0.687549796443564,
1.08333333333333));
#41279=CARTESIAN_POINT('Origin',(-13.892722748591,-3.17092330887753,3.20017169526126E-15));
#41280=CARTESIAN_POINT('',(-13.6476999686241,-6.55970790622096,1.08333333333334));
#41281=CARTESIAN_POINT('',(-13.1366786991091,-6.483368720524,1.08333333333334));
#41282=CARTESIAN_POINT('Origin',(-13.892722748591,-3.17092330887753,1.08333333333334));
#41283=CARTESIAN_POINT('',(-13.6476999686241,-6.55970790622096,-1.08333333333333));
#41284=CARTESIAN_POINT('Ctrl Pts',(-13.6476999686241,-6.55970790622096,
-1.08333333333332));
#41285=CARTESIAN_POINT('Ctrl Pts',(-13.5948858118208,-6.66958959248691,
-0.727666221822786));
#41286=CARTESIAN_POINT('Ctrl Pts',(-13.5683505740919,-6.72230205711272,
-0.35278297384277));
#41287=CARTESIAN_POINT('Ctrl Pts',(-13.5683505740919,-6.72230205711272,
0.352782973842779));
#41288=CARTESIAN_POINT('Ctrl Pts',(-13.5948858118208,-6.66958959248691,
0.727666221822796));
#41289=CARTESIAN_POINT('Ctrl Pts',(-13.6476999686241,-6.55970790622096,
1.08333333333333));
#41290=CARTESIAN_POINT('',(-12.7471768669563,-6.36961395396413,-1.08333333333333));
#41291=CARTESIAN_POINT('Origin',(-13.892722748591,-3.17092330887754,-1.08333333333333));
#41292=CARTESIAN_POINT('',(-12.7471768669563,-6.36961395396413,1.08333333333334));
#41293=CARTESIAN_POINT('Ctrl Pts',(-12.7471768669563,-6.36961395396412,
1.08333333333334));
#41294=CARTESIAN_POINT('Ctrl Pts',(-12.6958726976266,-6.472286317656,0.725928647976585));
#41295=CARTESIAN_POINT('Ctrl Pts',(-12.6703734952066,-6.52105325020167,
0.352039859176994));
#41296=CARTESIAN_POINT('Ctrl Pts',(-12.6703734952066,-6.52105325020167,
-0.352039859176985));
#41297=CARTESIAN_POINT('Ctrl Pts',(-12.6958726976266,-6.472286317656,-0.725928647976576));
#41298=CARTESIAN_POINT('Ctrl Pts',(-12.7471768669563,-6.36961395396413,
-1.08333333333333));
#41299=CARTESIAN_POINT('Origin',(-13.892722748591,-3.17092330887753,1.08333333333334));
#41300=CARTESIAN_POINT('',(-14.6487667980729,0.141522102768936,1.08333333333334));
#41301=CARTESIAN_POINT('Origin',(-13.892722748591,-3.17092330887753,3.20017169526126E-15));
#41302=CARTESIAN_POINT('',(-14.2484814298548,0.208031110850571,1.08333333333334));
#41303=CARTESIAN_POINT('Origin',(-13.892722748591,-3.17092330887753,1.08333333333334));
#41304=CARTESIAN_POINT('',(-14.2484814298548,0.20803111085057,-1.08333333333333));
#41305=CARTESIAN_POINT('Ctrl Pts',(-14.2484814298548,0.208031110850584,
-1.08333333333333));
#41306=CARTESIAN_POINT('Ctrl Pts',(-14.2468058395578,0.322795758952019,
-0.725928647976579));
#41307=CARTESIAN_POINT('Ctrl Pts',(-14.2449910310593,0.37779693624925,-0.352039859176988));
#41308=CARTESIAN_POINT('Ctrl Pts',(-14.2449910310593,0.37779693624925,2.46631154156404E-15));
#41309=CARTESIAN_POINT('Ctrl Pts',(-14.2449910310593,0.37779693624925,0.352039859176994));
#41310=CARTESIAN_POINT('Ctrl Pts',(-14.2468058395578,0.322795758952019,
0.725928647976587));
#41311=CARTESIAN_POINT('Ctrl Pts',(-14.2484814298548,0.208031110850583,
1.08333333333334));
#41312=CARTESIAN_POINT('',(-15.1423033840733,-0.0114224867028862,-1.08333333333333));
#41313=CARTESIAN_POINT('Origin',(-13.892722748591,-3.17092330887754,-1.08333333333333));
#41314=CARTESIAN_POINT('',(-15.1423033840733,-0.0114224867028857,1.08333333333334));
#41315=CARTESIAN_POINT('Ctrl Pts',(-15.1423033840733,-0.0114224867028744,
1.08333333333334));
#41316=CARTESIAN_POINT('Ctrl Pts',(-15.1423953499066,0.110492695607543,
0.727666221822802));
#41317=CARTESIAN_POINT('Ctrl Pts',(-15.1413590080604,0.169498193350012,
0.352782973842781));
#41318=CARTESIAN_POINT('Ctrl Pts',(-15.1413590080604,0.169498193350012,
2.67362166230902E-15));
#41319=CARTESIAN_POINT('Ctrl Pts',(-15.1413590080604,0.169498193350012,
-0.352782973842774));
#41320=CARTESIAN_POINT('Ctrl Pts',(-15.1423953499066,0.110492695607543,
-0.727666221822795));
#41321=CARTESIAN_POINT('Ctrl Pts',(-15.1423033840733,-0.0114224867028733,
-1.08333333333333));
#41322=CARTESIAN_POINT('Origin',(-13.892722748591,-3.17092330887753,1.08333333333334));
#41323=CARTESIAN_POINT('',(-13.0227870731057,-2.97236616780882,-3.45272288248773));
#41324=CARTESIAN_POINT('Origin',(-13.0227870731057,-2.97236616780882,2.99978307628674E-15));
#41325=CARTESIAN_POINT('',(-14.7626584240763,-3.36948044994625,-3.45272288248773));
#41326=CARTESIAN_POINT('Origin',(-14.7626584240763,-3.36948044994625,3.40056031423578E-15));
#41327=CARTESIAN_POINT('Origin',(-6.18284328242512,-12.8388063676095,4.97613300162231E-15));
#41328=CARTESIAN_POINT('',(-6.57000108040694,-13.6427478189686,3.96060240207311));
#41329=CARTESIAN_POINT('Origin',(-6.57000108040694,-13.6427478189686,5.28772891427451E-15));
#41330=CARTESIAN_POINT('',(-5.79568548444331,-12.0348649162504,3.96060240207311));
#41331=CARTESIAN_POINT('Origin',(-6.18284328242512,-12.8388063676095,2.51985201161581));
#41332=CARTESIAN_POINT('Origin',(-5.79568548444331,-12.0348649162504,4.66453708897012E-15));
#41333=CARTESIAN_POINT('',(-2.35859284151935,-14.0534529496467,-1.08333333333333));
#41334=CARTESIAN_POINT('',(-2.69569375163562,-14.9004267538186,-1.08333333333333));
#41335=CARTESIAN_POINT('Ctrl Pts',(-2.35859284151934,-14.0534529496467,
-1.08333333333333));
#41336=CARTESIAN_POINT('Ctrl Pts',(-2.37682723618162,-14.2398470420046,
-1.08333333333333));
#41337=CARTESIAN_POINT('Ctrl Pts',(-2.43502529011671,-14.4435268961719,
-1.08333333333332));
#41338=CARTESIAN_POINT('Ctrl Pts',(-2.56051322547963,-14.7041052789647,
-1.08333333333333));
#41339=CARTESIAN_POINT('Ctrl Pts',(-2.62287825309305,-14.806702452812,-1.08333333333333));
#41340=CARTESIAN_POINT('Ctrl Pts',(-2.69569375163558,-14.9004267538186,
-1.08333333333333));
#41341=CARTESIAN_POINT('',(-2.69569375163563,-14.9004267538187,1.08333333333334));
#41342=CARTESIAN_POINT('Ctrl Pts',(-2.69569375163559,-14.9004267538186,
1.08333333333335));
#41343=CARTESIAN_POINT('Ctrl Pts',(-2.65857154890325,-14.9071426748862,
0.955915065626573));
#41344=CARTESIAN_POINT('Ctrl Pts',(-2.628016775001,-14.9125315333598,0.826701571450498));
#41345=CARTESIAN_POINT('Ctrl Pts',(-2.60415669762586,-14.9166970252376,
0.696211209492072));
#41346=CARTESIAN_POINT('Ctrl Pts',(-2.58067270588166,-14.9207968600927,
0.567777653525379));
#41347=CARTESIAN_POINT('Ctrl Pts',(-2.56367395385075,-14.923711651889,0.438107164856101));
#41348=CARTESIAN_POINT('Ctrl Pts',(-2.55327224255806,-14.9254910506792,
0.307693975181385));
#41349=CARTESIAN_POINT('Ctrl Pts',(-2.54512176981446,-14.9268853348437,
0.205506064179128));
#41350=CARTESIAN_POINT('Ctrl Pts',(-2.54102158203148,-14.9275815713119,
0.102862147740959));
#41351=CARTESIAN_POINT('Ctrl Pts',(-2.54102158203148,-14.9275815713119,
4.44089209850063E-15));
#41352=CARTESIAN_POINT('Ctrl Pts',(-2.54102158203148,-14.9275815713119,
-0.130666807305524));
#41353=CARTESIAN_POINT('Ctrl Pts',(-2.54764001565181,-14.9264594186595,
-0.261069786498646));
#41354=CARTESIAN_POINT('Ctrl Pts',(-2.56079607270382,-14.9242020129234,
-0.390710450870999));
#41355=CARTESIAN_POINT('Ctrl Pts',(-2.57411009834303,-14.9219175018628,
-0.521907748246163));
#41356=CARTESIAN_POINT('Ctrl Pts',(-2.59411972995703,-14.9184702682937,
-0.652324314224157));
#41357=CARTESIAN_POINT('Ctrl Pts',(-2.62073179377387,-14.9137938537994,
-0.781443489202868));
#41358=CARTESIAN_POINT('Ctrl Pts',(-2.64165463403551,-14.9101171801624,
-0.882959098491507));
#41359=CARTESIAN_POINT('Ctrl Pts',(-2.66665850662476,-14.9056796321318,
-0.983672743459509));
#41360=CARTESIAN_POINT('Ctrl Pts',(-2.69569375163559,-14.9004267538186,
-1.08333333333334));
#41361=CARTESIAN_POINT('',(-2.35859284151935,-14.0534529496467,1.08333333333334));
#41362=CARTESIAN_POINT('Ctrl Pts',(-2.35859284151934,-14.0534529496467,
1.08333333333333));
#41363=CARTESIAN_POINT('Ctrl Pts',(-2.37688304383397,-14.2404175142851,
1.08333333333333));
#41364=CARTESIAN_POINT('Ctrl Pts',(-2.43503901504648,-14.4435553962822,
1.08333333333334));
#41365=CARTESIAN_POINT('Ctrl Pts',(-2.56054033827446,-14.7041615792632,
1.08333333333334));
#41366=CARTESIAN_POINT('Ctrl Pts',(-2.62284674626764,-14.8066618988743,
1.08333333333334));
#41367=CARTESIAN_POINT('Ctrl Pts',(-2.69569375163563,-14.9004267538187,
1.08333333333334));
#41368=CARTESIAN_POINT('Ctrl Pts',(-2.35859284151935,-14.0534529496467,
-1.08333333333333));
#41369=CARTESIAN_POINT('Ctrl Pts',(-2.32474809698527,-14.0591331175362,
-0.949622058007895));
#41370=CARTESIAN_POINT('Ctrl Pts',(-2.29723964086638,-14.0636285445206,
-0.814376693553736));
#41371=CARTESIAN_POINT('Ctrl Pts',(-2.27611794897253,-14.0670461391994,
-0.678132403728853));
#41372=CARTESIAN_POINT('Ctrl Pts',(-2.25509664145098,-14.0704474911881,
-0.542535637671543));
#41373=CARTESIAN_POINT('Ctrl Pts',(-2.24040145926613,-14.0727812605466,
-0.405949418799629));
#41374=CARTESIAN_POINT('Ctrl Pts',(-2.23207311688321,-14.0741020886196,
-0.268901316712528));
#41375=CARTESIAN_POINT('Ctrl Pts',(-2.22663511068775,-14.0749645256946,
-0.179415511019263));
#41376=CARTESIAN_POINT('Ctrl Pts',(-2.2239114043034,-14.075394064317,-0.0897327832369026));
#41377=CARTESIAN_POINT('Ctrl Pts',(-2.2239114043034,-14.075394064317,8.43769498715119E-15));
#41378=CARTESIAN_POINT('Ctrl Pts',(-2.2239114043034,-14.075394064317,0.137573936980349));
#41379=CARTESIAN_POINT('Ctrl Pts',(-2.23031275616482,-14.0743870796481,
0.274951212619667));
#41380=CARTESIAN_POINT('Ctrl Pts',(-2.24306143269717,-14.0723550057958,
0.411612406214657));
#41381=CARTESIAN_POINT('Ctrl Pts',(-2.25590874866049,-14.0703072093226,
0.549330978772813));
#41382=CARTESIAN_POINT('Ctrl Pts',(-2.27520203478074,-14.0672183663696,
0.68632234543694));
#41383=CARTESIAN_POINT('Ctrl Pts',(-2.30087730766032,-14.0630175856782,
0.822054935347292));
#41384=CARTESIAN_POINT('Ctrl Pts',(-2.31746020132759,-14.0603044266067,
0.909720570537337));
#41385=CARTESIAN_POINT('Ctrl Pts',(-2.33670515605249,-14.0571263627534,
0.996861109122898));
#41386=CARTESIAN_POINT('Ctrl Pts',(-2.35859284151935,-14.0534529496467,
1.08333333333334));
#41387=CARTESIAN_POINT('',(-9.96888517526507,-11.3978423664701,-1.08333333333333));
#41388=CARTESIAN_POINT('',(-9.516873369993,-10.6062067328295,-1.08333333333333));
#41389=CARTESIAN_POINT('Ctrl Pts',(-9.96888517526507,-11.3978423664701,
-1.08333333333333));
#41390=CARTESIAN_POINT('Ctrl Pts',(-9.94100828682427,-11.282476771434,-1.08333333333333));
#41391=CARTESIAN_POINT('Ctrl Pts',(-9.89967854500783,-11.1697495378475,
-1.08333333333333));
#41392=CARTESIAN_POINT('Ctrl Pts',(-9.77419060964491,-10.9091711550547,
-1.08333333333333));
#41393=CARTESIAN_POINT('Ctrl Pts',(-9.65123318042897,-10.7366777723525,
-1.08333333333333));
#41394=CARTESIAN_POINT('Ctrl Pts',(-9.51687336999256,-10.6062067328299,
-1.08333333333333));
#41395=CARTESIAN_POINT('',(-9.51687336999906,-10.6062067328363,1.08333333333334));
#41396=CARTESIAN_POINT('Ctrl Pts',(-9.51687336999256,-10.6062067328299,
1.08333333333319));
#41397=CARTESIAN_POINT('Ctrl Pts',(-9.54248335115827,-10.5832270800755,
0.949270311030248));
#41398=CARTESIAN_POINT('Ctrl Pts',(-9.56321910180067,-10.5644593135702,
0.813521288367661));
#41399=CARTESIAN_POINT('Ctrl Pts',(-9.57910097474595,-10.5500390764974,
0.676607052100613));
#41400=CARTESIAN_POINT('Ctrl Pts',(-9.59267821366648,-10.5377113740467,
0.559560573777554));
#41401=CARTESIAN_POINT('Ctrl Pts',(-9.6027075928823,-10.5285603838747,0.44166251627891));
#41402=CARTESIAN_POINT('Ctrl Pts',(-9.6091818848891,-10.5226481221753,0.323238258334718));
#41403=CARTESIAN_POINT('Ctrl Pts',(-9.61666296645239,-10.5158164698571,
0.186398348762648));
#41404=CARTESIAN_POINT('Ctrl Pts',(-9.61937600851194,-10.5133302394117,
0.0492519096262118));
#41405=CARTESIAN_POINT('Ctrl Pts',(-9.61735300288125,-10.5151805128572,
-0.08767582706605));
#41406=CARTESIAN_POINT('Ctrl Pts',(-9.61532413250719,-10.5170361502911,
-0.225000520654331));
#41407=CARTESIAN_POINT('Ctrl Pts',(-9.60853168799772,-10.5232534570122,
-0.362105241912796));
#41408=CARTESIAN_POINT('Ctrl Pts',(-9.59697252030892,-10.5337846211338,
-0.498460177595657));
#41409=CARTESIAN_POINT('Ctrl Pts',(-9.5853634847053,-10.5443612182148,-0.635403368116659));
#41410=CARTESIAN_POINT('Ctrl Pts',(-9.56894645381043,-10.5592890006364,
-0.771590289741169));
#41411=CARTESIAN_POINT('Ctrl Pts',(-9.54768316346852,-10.578480335569,-0.906484242526434));
#41412=CARTESIAN_POINT('Ctrl Pts',(-9.53834928383367,-10.5869046954593,
-0.965698216399696));
#41413=CARTESIAN_POINT('Ctrl Pts',(-9.52808112091929,-10.5961500981613,
-1.02466304565381));
#41414=CARTESIAN_POINT('Ctrl Pts',(-9.51687336999256,-10.6062067328299,
-1.08333333333318));
#41415=CARTESIAN_POINT('',(-9.96888517526507,-11.3978423664701,1.08333333333334));
#41416=CARTESIAN_POINT('Ctrl Pts',(-9.96888517526507,-11.3978423664701,
1.08333333333333));
#41417=CARTESIAN_POINT('Ctrl Pts',(-9.94100828682427,-11.282476771434,1.08333333333333));
#41418=CARTESIAN_POINT('Ctrl Pts',(-9.89967854500783,-11.1697495378475,
1.08333333333333));
#41419=CARTESIAN_POINT('Ctrl Pts',(-9.77419060964618,-10.9091711550573,
1.08333333333333));
#41420=CARTESIAN_POINT('Ctrl Pts',(-9.6512331804331,-10.7366777723579,1.08333333333333));
#41421=CARTESIAN_POINT('Ctrl Pts',(-9.51687336999908,-10.6062067328363,
1.08333333333333));
#41422=CARTESIAN_POINT('Ctrl Pts',(-9.96888517526508,-11.3978423664701,
-1.08333333333333));
#41423=CARTESIAN_POINT('Ctrl Pts',(-9.99706424266063,-11.3731961327199,
-0.956888632103256));
#41424=CARTESIAN_POINT('Ctrl Pts',(-10.020155672713,-11.3528209383891,-0.828820583351071));
#41425=CARTESIAN_POINT('Ctrl Pts',(-10.038197564346,-11.3368457653652,-0.699646919261599));
#41426=CARTESIAN_POINT('Ctrl Pts',(-10.0561445912219,-11.3209545902358,
-0.571152453812953));
#41427=CARTESIAN_POINT('Ctrl Pts',(-10.0690951385517,-11.3094172714603,
-0.441563969171296));
#41428=CARTESIAN_POINT('Ctrl Pts',(-10.0770534136919,-11.3023217413999,
-0.311391073637437));
#41429=CARTESIAN_POINT('Ctrl Pts',(-10.0849478229272,-11.2952831536342,
-0.182262827807044));
#41430=CARTESIAN_POINT('Ctrl Pts',(-10.0879298097314,-11.2926153440655,
-0.0525595133516554));
#41431=CARTESIAN_POINT('Ctrl Pts',(-10.0859696068728,-11.2943658227348,
0.0772214321950453));
#41432=CARTESIAN_POINT('Ctrl Pts',(-10.0846326712896,-11.2955597181575,
0.165737150534751));
#41433=CARTESIAN_POINT('Ctrl Pts',(-10.0809960349672,-11.2988081152181,
0.2542889811304));
#41434=CARTESIAN_POINT('Ctrl Pts',(-10.0750409796764,-11.304115688826,0.342719102199531));
#41435=CARTESIAN_POINT('Ctrl Pts',(-10.0660632343107,-11.3121173012435,
0.476034927301883));
#41436=CARTESIAN_POINT('Ctrl Pts',(-10.0518705086679,-11.3247537742305,
0.608312350206005));
#41437=CARTESIAN_POINT('Ctrl Pts',(-10.0325330571073,-11.3418588735079,
0.739057191238004));
#41438=CARTESIAN_POINT('Ctrl Pts',(-10.0153642561251,-11.3570456753652,
0.855139299994515));
#41439=CARTESIAN_POINT('Ctrl Pts',(-9.99413932000721,-11.3757543553326,
0.970013302477919));
#41440=CARTESIAN_POINT('Ctrl Pts',(-9.96888517526508,-11.3978423664701,
1.08333333333334));
#41441=CARTESIAN_POINT('Origin',(-6.18284328242512,-12.8388063676095,4.97613300162231E-15));
#41442=CARTESIAN_POINT('',(-3.38061559238688,-14.7601124814492,1.08333333333334));
#41443=CARTESIAN_POINT('',(-3.12168342103518,-14.3129832609672,1.08333333333334));
#41444=CARTESIAN_POINT('Origin',(-6.18284328242512,-12.8388063676095,1.08333333333334));
#41445=CARTESIAN_POINT('',(-3.38061559238688,-14.7601124814492,-1.08333333333333));
#41446=CARTESIAN_POINT('Ctrl Pts',(-3.38061559238688,-14.7601124814492,
-1.08333333333333));
#41447=CARTESIAN_POINT('Ctrl Pts',(-3.26177754255684,-14.7873308217382,
-0.727666221822789));
#41448=CARTESIAN_POINT('Ctrl Pts',(-3.20402082808,-14.799450421612,-0.35278297384277));
#41449=CARTESIAN_POINT('Ctrl Pts',(-3.20402082808,-14.799450421612,0.352782973842781));
#41450=CARTESIAN_POINT('Ctrl Pts',(-3.26177754255684,-14.7873308217382,
0.727666221822798));
#41451=CARTESIAN_POINT('Ctrl Pts',(-3.38061559238688,-14.7601124814492,
1.08333333333334));
#41452=CARTESIAN_POINT('',(-2.96777005865995,-13.9375335292483,-1.08333333333333));
#41453=CARTESIAN_POINT('Origin',(-6.18284328242512,-12.8388063676095,-1.08333333333333));
#41454=CARTESIAN_POINT('',(-2.96777005865995,-13.9375335292483,1.08333333333334));
#41455=CARTESIAN_POINT('Ctrl Pts',(-2.96777005865994,-13.9375335292483,
1.08333333333334));
#41456=CARTESIAN_POINT('Ctrl Pts',(-2.85550994597631,-13.9614374861791,
0.725928647976589));
#41457=CARTESIAN_POINT('Ctrl Pts',(-2.80148393014434,-13.9719070920595,
0.352039859176996));
#41458=CARTESIAN_POINT('Ctrl Pts',(-2.80148393014434,-13.9719070920595,
-0.352039859176986));
#41459=CARTESIAN_POINT('Ctrl Pts',(-2.85550994597631,-13.9614374861791,
-0.725928647976579));
#41460=CARTESIAN_POINT('Ctrl Pts',(-2.96777005865994,-13.9375335292483,
-1.08333333333333));
#41461=CARTESIAN_POINT('Origin',(-6.18284328242512,-12.8388063676095,1.08333333333334));
#41462=CARTESIAN_POINT('',(-9.24400314381506,-11.3646294742518,1.08333333333334));
#41463=CARTESIAN_POINT('Origin',(-6.18284328242512,-12.8388063676095,4.97613300162231E-15));
#41464=CARTESIAN_POINT('',(-9.04642813528379,-11.0102060831369,1.08333333333334));
#41465=CARTESIAN_POINT('Origin',(-6.18284328242512,-12.8388063676095,1.08333333333334));
#41466=CARTESIAN_POINT('',(-9.04642813528379,-11.0102060831369,-1.08333333333333));
#41467=CARTESIAN_POINT('Ctrl Pts',(-9.0464281352838,-11.0102060831369,-1.08333333333332));
#41468=CARTESIAN_POINT('Ctrl Pts',(-9.13511003678158,-10.9373414661859,
-0.725928647976569));
#41469=CARTESIAN_POINT('Ctrl Pts',(-9.17698017417422,-10.901629918632,-0.352039859176982));
#41470=CARTESIAN_POINT('Ctrl Pts',(-9.17698017417422,-10.901629918632,4.5383086406711E-15));
#41471=CARTESIAN_POINT('Ctrl Pts',(-9.17698017417422,-10.901629918632,0.352039859176991));
#41472=CARTESIAN_POINT('Ctrl Pts',(-9.13511003678158,-10.9373414661859,
0.725928647976579));
#41473=CARTESIAN_POINT('Ctrl Pts',(-9.0464281352838,-11.0102060831369,1.08333333333333));
#41474=CARTESIAN_POINT('',(-9.43214127690829,-11.8458513067218,-1.08333333333333));
#41475=CARTESIAN_POINT('Origin',(-6.18284328242512,-12.8388063676095,-1.08333333333333));
#41476=CARTESIAN_POINT('',(-9.43214127690829,-11.8458513067218,1.08333333333334));
#41477=CARTESIAN_POINT('Ctrl Pts',(-9.43214127690829,-11.8458513067218,
1.08333333333333));
#41478=CARTESIAN_POINT('Ctrl Pts',(-9.52751574438859,-11.7699103356433,
0.727666221822793));
#41479=CARTESIAN_POINT('Ctrl Pts',(-9.57300195158999,-11.7323107648653,
0.352782973842778));
#41480=CARTESIAN_POINT('Ctrl Pts',(-9.57300195158999,-11.7323107648653,
4.85994849902029E-15));
#41481=CARTESIAN_POINT('Ctrl Pts',(-9.57300195158999,-11.7323107648653,
-0.352782973842768));
#41482=CARTESIAN_POINT('Ctrl Pts',(-9.52751574438859,-11.7699103356433,
-0.727666221822784));
#41483=CARTESIAN_POINT('Ctrl Pts',(-9.43214127690829,-11.8458513067218,
-1.08333333333332));
#41484=CARTESIAN_POINT('Origin',(-6.18284328242512,-12.8388063676095,1.08333333333334));
#41485=CARTESIAN_POINT('',(-5.79568548444331,-12.0348649162504,-3.45272288248773));
#41486=CARTESIAN_POINT('Origin',(-5.79568548444331,-12.0348649162504,4.66453708897012E-15));
#41487=CARTESIAN_POINT('',(-6.57000108040694,-13.6427478189686,-3.45272288248772));
#41488=CARTESIAN_POINT('Origin',(-6.57000108040694,-13.6427478189686,5.28772891427451E-15));
#41489=CARTESIAN_POINT('Origin',(6.1828432824253,-12.8388063676094,4.9761330016223E-15));
#41490=CARTESIAN_POINT('',(6.57000108040713,-13.6427478189685,3.96060240207311));
#41491=CARTESIAN_POINT('Origin',(6.57000108040713,-13.6427478189685,5.28772891427449E-15));
#41492=CARTESIAN_POINT('',(5.79568548444348,-12.0348649162503,3.96060240207311));
#41493=CARTESIAN_POINT('Origin',(6.1828432824253,-12.8388063676094,2.51985201161581));
#41494=CARTESIAN_POINT('Origin',(5.79568548444348,-12.0348649162504,4.66453708897011E-15));
#41495=CARTESIAN_POINT('',(9.51687336999268,-10.6062067328298,-1.08333333333333));
#41496=CARTESIAN_POINT('',(9.96888517526453,-11.3978423664706,-1.08333333333333));
#41497=CARTESIAN_POINT('Ctrl Pts',(9.5168733699927,-10.6062067328298,-1.08333333333333));
#41498=CARTESIAN_POINT('Ctrl Pts',(9.65164439811578,-10.737077088181,-1.08333333333333));
#41499=CARTESIAN_POINT('Ctrl Pts',(9.77420433457484,-10.9091996551649,-1.08333333333333));
#41500=CARTESIAN_POINT('Ctrl Pts',(9.89970565780286,-11.169805838146,-1.08333333333333));
#41501=CARTESIAN_POINT('Ctrl Pts',(9.94099622466366,-11.2824268534395,-1.08333333333333));
#41502=CARTESIAN_POINT('Ctrl Pts',(9.96888517526534,-11.3978423664704,-1.08333333333333));
#41503=CARTESIAN_POINT('',(9.9688851752657,-11.3978423664719,1.08333333333334));
#41504=CARTESIAN_POINT('Ctrl Pts',(9.96888517526519,-11.39784236647,1.08333333333359));
#41505=CARTESIAN_POINT('Ctrl Pts',(9.99728120861575,-11.3730063679711,0.955915065626921));
#41506=CARTESIAN_POINT('Ctrl Pts',(10.0205449777511,-11.3524775820965,0.826701571450959));
#41507=CARTESIAN_POINT('Ctrl Pts',(10.038678205356,-11.3364201641361,0.696211209492648));
#41508=CARTESIAN_POINT('Ctrl Pts',(10.0565256146782,-11.3206158452779,0.567777653525928));
#41509=CARTESIAN_POINT('Ctrl Pts',(10.0694030392049,-11.309143028737,0.438107164856624));
#41510=CARTESIAN_POINT('Ctrl Pts',(10.0772795901119,-11.3021200803759,0.307693975181881));
#41511=CARTESIAN_POINT('Ctrl Pts',(10.0834514220032,-11.2966171061454,0.20550606417946));
#41512=CARTESIAN_POINT('Ctrl Pts',(10.0865521868617,-11.2938455465903,0.102862147741125));
#41513=CARTESIAN_POINT('Ctrl Pts',(10.0865521868617,-11.2938455465903,4.44089209850063E-15));
#41514=CARTESIAN_POINT('Ctrl Pts',(10.0865521868617,-11.2938455465903,-0.130666807305562));
#41515=CARTESIAN_POINT('Ctrl Pts',(10.0815483267233,-11.2983203956244,-0.261069786498721));
#41516=CARTESIAN_POINT('Ctrl Pts',(10.0715807484455,-11.3071987457576,-0.390710450871112));
#41517=CARTESIAN_POINT('Ctrl Pts',(10.0614934865685,-11.3161837008123,-0.521907748246463));
#41518=CARTESIAN_POINT('Ctrl Pts',(10.0463225295865,-11.3296785457857,-0.652324314224642));
#41519=CARTESIAN_POINT('Ctrl Pts',(10.0260740111135,-11.3475689983448,-0.781443489203535));
#41520=CARTESIAN_POINT('Ctrl Pts',(10.0101542943843,-11.3616347650465,-0.88295909849203));
#41521=CARTESIAN_POINT('Ctrl Pts',(9.99109522006272,-11.3784168138781,-0.983672743459888));
#41522=CARTESIAN_POINT('Ctrl Pts',(9.96888517526519,-11.39784236647,-1.08333333333358));
#41523=CARTESIAN_POINT('',(9.51687336999268,-10.6062067328298,1.08333333333334));
#41524=CARTESIAN_POINT('Ctrl Pts',(9.5168733699927,-10.6062067328298,1.08333333333333));
#41525=CARTESIAN_POINT('Ctrl Pts',(9.65123318042911,-10.7366777723523,1.08333333333333));
#41526=CARTESIAN_POINT('Ctrl Pts',(9.77419060964506,-10.9091711550545,1.08333333333333));
#41527=CARTESIAN_POINT('Ctrl Pts',(9.89967854500826,-11.1697495378479,1.08333333333333));
#41528=CARTESIAN_POINT('Ctrl Pts',(9.94100828682489,-11.2824767714351,1.08333333333333));
#41529=CARTESIAN_POINT('Ctrl Pts',(9.96888517526571,-11.3978423664719,1.08333333333333));
#41530=CARTESIAN_POINT('Ctrl Pts',(9.51687336999268,-10.6062067328298,-1.08333333333333));
#41531=CARTESIAN_POINT('Ctrl Pts',(9.54241615713793,-10.5832873727889,-0.949622058007762));
#41532=CARTESIAN_POINT('Ctrl Pts',(9.56308206533645,-10.5645832486408,-0.814376693553466));
#41533=CARTESIAN_POINT('Ctrl Pts',(9.5789232079445,-10.5502004803844,-0.678132403728444));
#41534=CARTESIAN_POINT('Ctrl Pts',(9.59468906287363,-10.5358860686389,-0.542535637671145));
#41535=CARTESIAN_POINT('Ctrl Pts',(9.60567597345963,-10.5258519939611,-0.405949418799242));
#41536=CARTESIAN_POINT('Ctrl Pts',(9.61190127497217,-10.5201641565229,-0.268901316712153));
#41537=CARTESIAN_POINT('Ctrl Pts',(9.61596609683434,-10.5164502727984,-0.179415511019018));
#41538=CARTESIAN_POINT('Ctrl Pts',(9.61800012680612,-10.5145886063487,-0.0897327832367887));
#41539=CARTESIAN_POINT('Ctrl Pts',(9.61800012680612,-10.5145886063487,-9.32587340685131E-15));
#41540=CARTESIAN_POINT('Ctrl Pts',(9.61800012680612,-10.5145886063487,0.137573936980381));
#41541=CARTESIAN_POINT('Ctrl Pts',(9.61322165688595,-10.5189655400926,0.274951212619743));
#41542=CARTESIAN_POINT('Ctrl Pts',(9.6036842477684,-10.5276658794419,0.411612406214774));
#41543=CARTESIAN_POINT('Ctrl Pts',(9.59407304553156,-10.5364335353099,0.54933097877281));
#41544=CARTESIAN_POINT('Ctrl Pts',(9.57962892372621,-10.5495917717182,0.686322345436814));
#41545=CARTESIAN_POINT('Ctrl Pts',(9.5603363503304,-10.5670463644555,0.822054935347047));
#41546=CARTESIAN_POINT('Ctrl Pts',(9.54787585206456,-10.5783197657831,0.909720570537174));
#41547=CARTESIAN_POINT('Ctrl Pts',(9.5333921086825,-10.5913845868635,0.996861109122817));
#41548=CARTESIAN_POINT('Ctrl Pts',(9.51687336999268,-10.6062067328298,1.08333333333334));
#41549=CARTESIAN_POINT('',(2.69569375163578,-14.9004267538186,-1.08333333333333));
#41550=CARTESIAN_POINT('',(2.35859284151893,-14.0534529496468,-1.08333333333333));
#41551=CARTESIAN_POINT('Ctrl Pts',(2.6956937516358,-14.9004267538186,-1.08333333333332));
#41552=CARTESIAN_POINT('Ctrl Pts',(2.62284674626782,-14.8066618988742,-1.08333333333332));
#41553=CARTESIAN_POINT('Ctrl Pts',(2.56054033827465,-14.7041615792632,-1.08333333333332));
#41554=CARTESIAN_POINT('Ctrl Pts',(2.4350390150467,-14.4435553962822,-1.08333333333332));
#41555=CARTESIAN_POINT('Ctrl Pts',(2.37688304383419,-14.2404175142851,-1.08333333333332));
#41556=CARTESIAN_POINT('Ctrl Pts',(2.35859284151955,-14.0534529496467,-1.08333333333332));
#41557=CARTESIAN_POINT('',(2.35859284152043,-14.0534529496557,1.08333333333334));
#41558=CARTESIAN_POINT('Ctrl Pts',(2.35859284151951,-14.0534529496467,1.08333333333319));
#41559=CARTESIAN_POINT('Ctrl Pts',(2.32465906345733,-14.0591480600448,0.949270311030372));
#41560=CARTESIAN_POINT('Ctrl Pts',(2.29705730368849,-14.0636584116899,0.813521288367913));
#41561=CARTESIAN_POINT('Ctrl Pts',(2.27588092254449,-14.0670844892038,0.676607052100994));
#41562=CARTESIAN_POINT('Ctrl Pts',(2.25777746665768,-14.0700134052785,0.55956057377781));
#41563=CARTESIAN_POINT('Ctrl Pts',(2.24436971878542,-14.0721491406499,0.441662516279038));
#41564=CARTESIAN_POINT('Ctrl Pts',(2.23571067141573,-14.073524711092,0.323238258334718));
#41565=CARTESIAN_POINT('Ctrl Pts',(2.2257050924945,-14.0751141906309,0.186398348762649));
#41566=CARTESIAN_POINT('Ctrl Pts',(2.22206972520347,-14.0756851929985,0.0492519096262131));
#41567=CARTESIAN_POINT('Ctrl Pts',(2.22477765061414,-14.0752571701311,-0.087675827066048));
#41568=CARTESIAN_POINT('Ctrl Pts',(2.22749342636756,-14.0748279064149,-0.225000520654297));
#41569=CARTESIAN_POINT('Ctrl Pts',(2.23658933237962,-14.0733937867901,-0.362105241912729));
#41570=CARTESIAN_POINT('Ctrl Pts',(2.25202995120888,-14.0709225390114,-0.498460177595558));
#41571=CARTESIAN_POINT('Ctrl Pts',(2.26753718309241,-14.0684406299137,-0.635403368116538));
#41572=CARTESIAN_POINT('Ctrl Pts',(2.28944404469282,-14.0649125984157,-0.771590289741026));
#41573=CARTESIAN_POINT('Ctrl Pts',(2.31770587921582,-14.0602538902201,-0.906484242526269));
#41574=CARTESIAN_POINT('Ctrl Pts',(2.33011188776182,-14.0582088717468,-0.965698216399587));
#41575=CARTESIAN_POINT('Ctrl Pts',(2.34374232952329,-14.0559453130119,-1.02466304565376));
#41576=CARTESIAN_POINT('Ctrl Pts',(2.35859284151951,-14.0534529496467,-1.08333333333318));
#41577=CARTESIAN_POINT('',(2.69569375163578,-14.9004267538186,1.08333333333334));
#41578=CARTESIAN_POINT('Ctrl Pts',(2.6956937516358,-14.9004267538186,1.08333333333334));
#41579=CARTESIAN_POINT('Ctrl Pts',(2.62284674626782,-14.8066618988742,1.08333333333334));
#41580=CARTESIAN_POINT('Ctrl Pts',(2.56054033827465,-14.7041615792632,1.08333333333334));
#41581=CARTESIAN_POINT('Ctrl Pts',(2.43503901504795,-14.4435553962848,1.08333333333334));
#41582=CARTESIAN_POINT('Ctrl Pts',(2.37688304383586,-14.2404175142916,1.08333333333334));
#41583=CARTESIAN_POINT('Ctrl Pts',(2.35859284152042,-14.0534529496557,1.08333333333334));
#41584=CARTESIAN_POINT('Ctrl Pts',(2.69569375163578,-14.9004267538186,-1.08333333333333));
#41585=CARTESIAN_POINT('Ctrl Pts',(2.65885518901859,-14.9070913604575,-0.956888632103347));
#41586=CARTESIAN_POINT('Ctrl Pts',(2.62852794948137,-14.9124412415715,-0.828820583351256));
#41587=CARTESIAN_POINT('Ctrl Pts',(2.60478912083403,-14.9165866029902,-0.699646919261879));
#41588=CARTESIAN_POINT('Ctrl Pts',(2.58117511159368,-14.9207101679857,-0.571152453813268));
#41589=CARTESIAN_POINT('Ctrl Pts',(2.56408033836306,-14.9236419130061,-0.441563969171648));
#41590=CARTESIAN_POINT('Ctrl Pts',(2.55357092618676,-14.9254399524253,-0.311391073637824));
#41591=CARTESIAN_POINT('Ctrl Pts',(2.54314585302948,-14.9272235624095,-0.182262827807427));
#41592=CARTESIAN_POINT('Ctrl Pts',(2.53920083715778,-14.927891621514,-0.0525595133520343));
#41593=CARTESIAN_POINT('Ctrl Pts',(2.54179158298272,-14.9274504788058,0.077221432194672));
#41594=CARTESIAN_POINT('Ctrl Pts',(2.54355857371286,-14.9271496020974,0.165737150534507));
#41595=CARTESIAN_POINT('Ctrl Pts',(2.54836567846244,-14.9263317077699,0.254288981130285));
#41596=CARTESIAN_POINT('Ctrl Pts',(2.55622822284789,-14.9249850760809,0.342719102199546));
#41597=CARTESIAN_POINT('Ctrl Pts',(2.56808166802554,-14.9229549158531,0.47603492730158));
#41598=CARTESIAN_POINT('Ctrl Pts',(2.58681028013297,-14.9197373081624,0.608312350205393));
#41599=CARTESIAN_POINT('Ctrl Pts',(2.61224028910069,-14.9152835347009,0.739057191237091));
#41600=CARTESIAN_POINT('Ctrl Pts',(2.63481838123332,-14.9113292416576,0.855139299993913));
#41601=CARTESIAN_POINT('Ctrl Pts',(2.66267894744191,-14.9063995895532,0.970013302477622));
#41602=CARTESIAN_POINT('Ctrl Pts',(2.69569375163578,-14.9004267538186,1.08333333333334));
#41603=CARTESIAN_POINT('Origin',(6.1828432824253,-12.8388063676094,4.9761330016223E-15));
#41604=CARTESIAN_POINT('',(9.43214127690845,-11.8458513067217,1.08333333333334));
#41605=CARTESIAN_POINT('',(9.24400314381522,-11.3646294742516,1.08333333333334));
#41606=CARTESIAN_POINT('Origin',(6.1828432824253,-12.8388063676094,1.08333333333334));
#41607=CARTESIAN_POINT('',(9.43214127690845,-11.8458513067217,-1.08333333333333));
#41608=CARTESIAN_POINT('Ctrl Pts',(9.43214127690846,-11.8458513067217,-1.08333333333333));
#41609=CARTESIAN_POINT('Ctrl Pts',(9.52751574438875,-11.7699103356432,-0.727666221822791));
#41610=CARTESIAN_POINT('Ctrl Pts',(9.57300195159016,-11.7323107648652,-0.352782973842771));
#41611=CARTESIAN_POINT('Ctrl Pts',(9.57300195159016,-11.7323107648652,0.35278297384278));
#41612=CARTESIAN_POINT('Ctrl Pts',(9.52751574438876,-11.7699103356432,0.7276662218228));
#41613=CARTESIAN_POINT('Ctrl Pts',(9.43214127690846,-11.8458513067217,1.08333333333334));
#41614=CARTESIAN_POINT('',(9.04642813528394,-11.0102060831368,-1.08333333333333));
#41615=CARTESIAN_POINT('Origin',(6.1828432824253,-12.8388063676094,-1.08333333333333));
#41616=CARTESIAN_POINT('',(9.04642813528394,-11.0102060831368,1.08333333333334));
#41617=CARTESIAN_POINT('Ctrl Pts',(9.04642813528396,-11.0102060831368,1.08333333333334));
#41618=CARTESIAN_POINT('Ctrl Pts',(9.13511003678174,-10.9373414661857,0.725928647976586));
#41619=CARTESIAN_POINT('Ctrl Pts',(9.17698017417438,-10.9016299186319,0.352039859176995));
#41620=CARTESIAN_POINT('Ctrl Pts',(9.17698017417438,-10.9016299186319,-0.352039859176985));
#41621=CARTESIAN_POINT('Ctrl Pts',(9.13511003678174,-10.9373414661857,-0.725928647976577));
#41622=CARTESIAN_POINT('Ctrl Pts',(9.04642813528395,-11.0102060831368,-1.08333333333333));
#41623=CARTESIAN_POINT('Origin',(6.1828432824253,-12.8388063676094,1.08333333333334));
#41624=CARTESIAN_POINT('',(3.12168342103538,-14.3129832609672,1.08333333333334));
#41625=CARTESIAN_POINT('Origin',(6.1828432824253,-12.8388063676094,4.9761330016223E-15));
#41626=CARTESIAN_POINT('',(2.96777005866014,-13.9375335292483,1.08333333333334));
#41627=CARTESIAN_POINT('Origin',(6.1828432824253,-12.8388063676094,1.08333333333334));
#41628=CARTESIAN_POINT('',(2.96777005866014,-13.9375335292483,-1.08333333333333));
#41629=CARTESIAN_POINT('Ctrl Pts',(2.96777005866014,-13.9375335292483,-1.08333333333333));
#41630=CARTESIAN_POINT('Ctrl Pts',(2.85550994597651,-13.9614374861791,-0.725928647976576));
#41631=CARTESIAN_POINT('Ctrl Pts',(2.80148393014454,-13.9719070920595,-0.352039859176985));
#41632=CARTESIAN_POINT('Ctrl Pts',(2.80148393014454,-13.9719070920595,5.10230940761107E-15));
#41633=CARTESIAN_POINT('Ctrl Pts',(2.80148393014454,-13.9719070920595,0.352039859176993));
#41634=CARTESIAN_POINT('Ctrl Pts',(2.85550994597651,-13.9614374861791,0.725928647976584));
#41635=CARTESIAN_POINT('Ctrl Pts',(2.96777005866014,-13.9375335292483,1.08333333333333));
#41636=CARTESIAN_POINT('',(3.38061559238708,-14.7601124814491,-1.08333333333333));
#41637=CARTESIAN_POINT('Origin',(6.1828432824253,-12.8388063676094,-1.08333333333333));
#41638=CARTESIAN_POINT('',(3.38061559238708,-14.7601124814491,1.08333333333334));
#41639=CARTESIAN_POINT('Ctrl Pts',(3.3806155923871,-14.7601124814491,1.08333333333334));
#41640=CARTESIAN_POINT('Ctrl Pts',(3.26177754255705,-14.7873308217381,0.727666221822799));
#41641=CARTESIAN_POINT('Ctrl Pts',(3.20402082808022,-14.7994504216119,0.35278297384278));
#41642=CARTESIAN_POINT('Ctrl Pts',(3.20402082808022,-14.7994504216119,5.42337291349619E-15));
#41643=CARTESIAN_POINT('Ctrl Pts',(3.20402082808022,-14.7994504216119,-0.35278297384277));
#41644=CARTESIAN_POINT('Ctrl Pts',(3.26177754255705,-14.7873308217381,-0.727666221822788));
#41645=CARTESIAN_POINT('Ctrl Pts',(3.3806155923871,-14.7601124814491,-1.08333333333333));
#41646=CARTESIAN_POINT('Origin',(6.1828432824253,-12.8388063676094,1.08333333333334));
#41647=CARTESIAN_POINT('',(5.79568548444348,-12.0348649162504,-3.45272288248773));
#41648=CARTESIAN_POINT('Origin',(5.79568548444348,-12.0348649162504,4.66453708897011E-15));
#41649=CARTESIAN_POINT('',(6.57000108040713,-13.6427478189685,-3.45272288248772));
#41650=CARTESIAN_POINT('Origin',(6.57000108040713,-13.6427478189685,5.28772891427449E-15));
#41651=CARTESIAN_POINT('Origin',(13.892722748591,-3.17092330887735,3.20017169526122E-15));
#41652=CARTESIAN_POINT('',(14.7626584240763,-3.36948044994605,3.96060240207311));
#41653=CARTESIAN_POINT('Origin',(14.7626584240763,-3.36948044994605,3.40056031423575E-15));
#41654=CARTESIAN_POINT('',(13.0227870731057,-2.97236616780864,3.96060240207311));
#41655=CARTESIAN_POINT('Origin',(13.892722748591,-3.17092330887735,2.5198520116158));
#41656=CARTESIAN_POINT('Origin',(13.0227870731057,-2.97236616780865,2.9997830762867E-15));
#41657=CARTESIAN_POINT('',(14.2259398250621,0.827729480997053,-1.08333333333333));
#41658=CARTESIAN_POINT('',(15.1266902369927,0.68754979644376,-1.08333333333333));
#41659=CARTESIAN_POINT('Ctrl Pts',(14.2259398250621,0.827729480997104,-1.08333333333333));
#41660=CARTESIAN_POINT('Ctrl Pts',(14.4122867506183,0.85150138178118,-1.08333333333333));
#41661=CARTESIAN_POINT('Ctrl Pts',(14.6232724628281,0.840005933409976,-1.08333333333333));
#41662=CARTESIAN_POINT('Ctrl Pts',(14.9052713763609,0.775641521611009,-1.08333333333333));
#41663=CARTESIAN_POINT('Ctrl Pts',(15.0190662790554,0.737705732201359,-1.08333333333333));
#41664=CARTESIAN_POINT('Ctrl Pts',(15.1266902369927,0.687549796443767,-1.08333333333333));
#41665=CARTESIAN_POINT('',(15.1266902369927,0.687549796443762,1.08333333333334));
#41666=CARTESIAN_POINT('Ctrl Pts',(15.1266902369927,0.687549796443768,1.08333333333334));
#41667=CARTESIAN_POINT('Ctrl Pts',(15.1249773086751,0.725235701077452,0.955915065626868));
#41668=CARTESIAN_POINT('Ctrl Pts',(15.1234319803901,0.756223536825589,0.826701571451108));
#41669=CARTESIAN_POINT('Ctrl Pts',(15.122183667988,0.780412301388443,0.696211209493001));
#41670=CARTESIAN_POINT('Ctrl Pts',(15.1209550316477,0.804219799510377,0.567777653526322));
#41671=CARTESIAN_POINT('Ctrl Pts',(15.12001416535,0.821440959530357,0.43810716485706));
#41672=CARTESIAN_POINT('Ctrl Pts',(15.1194343523859,0.831977831684773,0.307693975182356));
#41673=CARTESIAN_POINT('Ctrl Pts',(15.1189800281283,0.840234212474528,0.205506064179778));
#41674=CARTESIAN_POINT('Ctrl Pts',(15.1187464308798,0.844386527178536,0.102862147741283));
#41675=CARTESIAN_POINT('Ctrl Pts',(15.1187464308798,0.844386527178536,1.99840144432528E-15));
#41676=CARTESIAN_POINT('Ctrl Pts',(15.1187464308798,0.844386527178536,-0.130666807305585));
#41677=CARTESIAN_POINT('Ctrl Pts',(15.1191251529677,0.837684329050871,-0.261069786498764));
#41678=CARTESIAN_POINT('Ctrl Pts',(15.1198518432089,0.824355801783881,-0.390710450871172));
#41679=CARTESIAN_POINT('Ctrl Pts',(15.1205872590302,0.810867235029882,-0.521907748246314));
#41680=CARTESIAN_POINT('Ctrl Pts',(15.1216790167187,0.790592205023559,-0.652324314224285));
#41681=CARTESIAN_POINT('Ctrl Pts',(15.1230415909943,0.763606761086929,-0.781443489202972));
#41682=CARTESIAN_POINT('Ctrl Pts',(15.1241128691977,0.742390363262186,-0.882959098491574));
#41683=CARTESIAN_POINT('Ctrl Pts',(15.1253504648421,0.717025942630064,-0.983672743459537));
#41684=CARTESIAN_POINT('Ctrl Pts',(15.1266902369927,0.687549796443768,-1.08333333333333));
#41685=CARTESIAN_POINT('',(14.2259398250621,0.827729480997055,1.08333333333334));
#41686=CARTESIAN_POINT('Ctrl Pts',(14.2259398250621,0.827729480997104,1.08333333333333));
#41687=CARTESIAN_POINT('Ctrl Pts',(14.4122867506183,0.85150138178118,1.08333333333333));
#41688=CARTESIAN_POINT('Ctrl Pts',(14.6232724628281,0.840005933409977,1.08333333333333));
#41689=CARTESIAN_POINT('Ctrl Pts',(14.9052713763609,0.775641521611009,1.08333333333333));
#41690=CARTESIAN_POINT('Ctrl Pts',(15.0190662790554,0.73770573220136,1.08333333333333));
#41691=CARTESIAN_POINT('Ctrl Pts',(15.1266902369927,0.687549796443768,1.08333333333333));
#41692=CARTESIAN_POINT('Ctrl Pts',(14.2259398250621,0.8277294809971,-1.08333333333334));
#41693=CARTESIAN_POINT('Ctrl Pts',(14.2239464151202,0.861989623387911,-0.949622058007612));
#41694=CARTESIAN_POINT('Ctrl Pts',(14.2222079250172,0.889808711690379,-0.814376693553152));
#41695=CARTESIAN_POINT('Ctrl Pts',(14.2208398148552,0.911161325030034,-0.678132403727965));
#41696=CARTESIAN_POINT('Ctrl Pts',(14.2194782068654,0.932412456504566,-0.542535637670654));
#41697=CARTESIAN_POINT('Ctrl Pts',(14.2184834780892,0.947258512328438,-0.40594941879874));
#41698=CARTESIAN_POINT('Ctrl Pts',(14.2179179597194,0.955671957676133,-0.268901316711642));
#41699=CARTESIAN_POINT('Ctrl Pts',(14.2175487034788,0.961165532006069,-0.179415511018676));
#41700=CARTESIAN_POINT('Ctrl Pts',(14.2173613909827,0.963916530720146,-0.0897327832366183));
#41701=CARTESIAN_POINT('Ctrl Pts',(14.2173613909827,0.963916530720146,-1.06581410364015E-14));
#41702=CARTESIAN_POINT('Ctrl Pts',(14.2173613909827,0.963916530720146,0.13757393698032));
#41703=CARTESIAN_POINT('Ctrl Pts',(14.2178040883167,0.957451598945758,0.274951212619625));
#41704=CARTESIAN_POINT('Ctrl Pts',(14.2186598102071,0.944570379379524,0.411612406214599));
#41705=CARTESIAN_POINT('Ctrl Pts',(14.2195221530139,0.931589494866494,0.549330978772693));
#41706=CARTESIAN_POINT('Ctrl Pts',(14.2208039138492,0.912092599491427,0.686322345436757));
#41707=CARTESIAN_POINT('Ctrl Pts',(14.222421741201,0.886126297665472,0.822054935347047));
#41708=CARTESIAN_POINT('Ctrl Pts',(14.2234666476786,0.869355437073955,0.909720570537178));
#41709=CARTESIAN_POINT('Ctrl Pts',(14.2246506698206,0.849885807807131,0.996861109122824));
#41710=CARTESIAN_POINT('Ctrl Pts',(14.2259398250621,0.827729480997101,1.08333333333335));
#41711=CARTESIAN_POINT('',(13.3303603014235,-7.18268588222768,-1.08333333333333));
#41712=CARTESIAN_POINT('',(12.4579905368411,-6.91816245718305,-1.08333333333333));
#41713=CARTESIAN_POINT('Ctrl Pts',(13.3303603014235,-7.18268588222769,-1.08333333333333));
#41714=CARTESIAN_POINT('Ctrl Pts',(13.2116326209361,-7.18117853359731,-1.08333333333333));
#41715=CARTESIAN_POINT('Ctrl Pts',(13.0926472341269,-7.16598374096113,-1.08333333333333));
#41716=CARTESIAN_POINT('Ctrl Pts',(12.8106483205942,-7.10161932916216,-1.08333333333333));
#41717=CARTESIAN_POINT('Ctrl Pts',(12.6155690741987,-7.02043310055321,-1.08333333333333));
#41718=CARTESIAN_POINT('Ctrl Pts',(12.4579905368414,-6.91816245718254,-1.08333333333333));
#41719=CARTESIAN_POINT('',(12.4579905368491,-6.91816245718746,1.08333333333334));
#41720=CARTESIAN_POINT('Ctrl Pts',(12.4579905368414,-6.91816245718254,1.08333333333318));
#41721=CARTESIAN_POINT('Ctrl Pts',(12.4412857888865,-6.94824379644432,0.949270311030419));
#41722=CARTESIAN_POINT('Ctrl Pts',(12.4276027080704,-6.97263587945666,0.813521288368017));
#41723=CARTESIAN_POINT('Ctrl Pts',(12.4170780656486,-6.99132836531005,0.676607052101155));
#41724=CARTESIAN_POINT('Ctrl Pts',(12.4080806643215,-7.00730836636693,0.559560573777918));
#41725=CARTESIAN_POINT('Ctrl Pts',(12.4013908554088,-7.019122574986,0.441662516279092));
#41726=CARTESIAN_POINT('Ctrl Pts',(12.397067491958,-7.0267501449702,0.323238258334718));
#41727=CARTESIAN_POINT('Ctrl Pts',(12.3920718206831,-7.03556384585387,0.186398348762654));
#41728=CARTESIAN_POINT('Ctrl Pts',(12.3902516338787,-7.03876210460539,0.0492519096262223));
#41729=CARTESIAN_POINT('Ctrl Pts',(12.3916053560035,-7.03637809537437,-0.0876758270660355));
#41730=CARTESIAN_POINT('Ctrl Pts',(12.3929630026023,-7.03398717484161,-0.225000520654302));
#41731=CARTESIAN_POINT('Ctrl Pts',(12.3975129673672,-7.02598155019911,-0.362105241912753));
#41732=CARTESIAN_POINT('Ctrl Pts',(12.4052079364272,-7.01236879050172,-0.498460177595601));
#41733=CARTESIAN_POINT('Ctrl Pts',(12.4129361026925,-6.99869730339771,-0.635403368116608));
#41734=CARTESIAN_POINT('Ctrl Pts',(12.4238364813948,-6.9793701376568,-0.771590289741124));
#41735=CARTESIAN_POINT('Ctrl Pts',(12.4378151222668,-6.95436948862457,-0.906484242526394));
#41736=CARTESIAN_POINT('Ctrl Pts',(12.4439512822523,-6.94339503240884,-0.96569821639967));
#41737=CARTESIAN_POINT('Ctrl Pts',(12.4506800022041,-6.93132701813272,-1.0246630456538));
#41738=CARTESIAN_POINT('Ctrl Pts',(12.4579905368414,-6.91816245718254,-1.08333333333318));
#41739=CARTESIAN_POINT('',(13.3303603014235,-7.18268588222768,1.08333333333334));
#41740=CARTESIAN_POINT('Ctrl Pts',(13.3303603014235,-7.18268588222769,1.08333333333333));
#41741=CARTESIAN_POINT('Ctrl Pts',(13.2116326209361,-7.18117853359731,1.08333333333333));
#41742=CARTESIAN_POINT('Ctrl Pts',(13.0926472341269,-7.16598374096113,1.08333333333333));
#41743=CARTESIAN_POINT('Ctrl Pts',(12.810648320597,-7.10161932916281,1.08333333333333));
#41744=CARTESIAN_POINT('Ctrl Pts',(12.6155690742049,-7.020433100556,1.08333333333333));
#41745=CARTESIAN_POINT('Ctrl Pts',(12.4579905368491,-6.91816245718749,1.08333333333333));
#41746=CARTESIAN_POINT('Ctrl Pts',(13.3303603014235,-7.18268588222769,-1.08333333333333));
#41747=CARTESIAN_POINT('Ctrl Pts',(13.3126024326051,-7.21564274452345,-0.956888632103319));
#41748=CARTESIAN_POINT('Ctrl Pts',(13.2978764135175,-7.24268913148574,-0.828820583351199));
#41749=CARTESIAN_POINT('Ctrl Pts',(13.2863164700112,-7.26383348564869,-0.699646919261793));
#41750=CARTESIAN_POINT('Ctrl Pts',(13.2748173090023,-7.28486666222208,-0.57115245381317));
#41751=CARTESIAN_POINT('Ctrl Pts',(13.2664510227834,-7.30005980724128,-0.441563969171537));
#41752=CARTESIAN_POINT('Ctrl Pts',(13.2613042752927,-7.30939745578421,-0.311391073637702));
#41753=CARTESIAN_POINT('Ctrl Pts',(13.2561988309336,-7.31866016882124,-0.182262827807302));
#41754=CARTESIAN_POINT('Ctrl Pts',(13.2542614634095,-7.32216103446727,-0.0525595133519065));
#41755=CARTESIAN_POINT('Ctrl Pts',(13.2555318677529,-7.3198604598385,0.0772214321948015));
#41756=CARTESIAN_POINT('Ctrl Pts',(13.2563983335702,-7.31829137729713,0.16573715053459));
#41757=CARTESIAN_POINT('Ctrl Pts',(13.2587560588235,-7.31402308269219,0.254288981130321));
#41758=CARTESIAN_POINT('Ctrl Pts',(13.2626054360147,-7.30703628683439,0.342719102199534));
#41759=CARTESIAN_POINT('Ctrl Pts',(13.2684086950193,-7.29650310602066,0.476034927301568));
#41760=CARTESIAN_POINT('Ctrl Pts',(13.2775701666805,-7.2798543418706,0.608312350205377));
#41761=CARTESIAN_POINT('Ctrl Pts',(13.289943417625,-7.25719547792716,0.739057191237071));
#41762=CARTESIAN_POINT('Ctrl Pts',(13.300929037023,-7.23707775329776,0.8551392999939));
#41763=CARTESIAN_POINT('Ctrl Pts',(13.3144456587152,-7.21222189770271,0.970013302477615));
#41764=CARTESIAN_POINT('Ctrl Pts',(13.3303603014235,-7.18268588222769,1.08333333333334));
#41765=CARTESIAN_POINT('Origin',(13.892722748591,-3.17092330887735,3.20017169526122E-15));
#41766=CARTESIAN_POINT('',(15.1423033840733,-0.0114224867026808,1.08333333333334));
#41767=CARTESIAN_POINT('',(14.6487667980729,0.141522102769127,1.08333333333334));
#41768=CARTESIAN_POINT('Origin',(13.892722748591,-3.17092330887735,1.08333333333334));
#41769=CARTESIAN_POINT('',(15.1423033840733,-0.0114224867026808,-1.08333333333333));
#41770=CARTESIAN_POINT('Ctrl Pts',(15.1423033840733,-0.0114224867026917,
-1.08333333333333));
#41771=CARTESIAN_POINT('Ctrl Pts',(15.1423953499066,0.110492695607724,-0.727666221822789));
#41772=CARTESIAN_POINT('Ctrl Pts',(15.1413590080604,0.169498193350193,-0.352782973842772));
#41773=CARTESIAN_POINT('Ctrl Pts',(15.1413590080604,0.169498193350193,0.352782973842778));
#41774=CARTESIAN_POINT('Ctrl Pts',(15.1423953499066,0.110492695607724,0.727666221822797));
#41775=CARTESIAN_POINT('Ctrl Pts',(15.1423033840733,-0.0114224867026924,
1.08333333333334));
#41776=CARTESIAN_POINT('',(14.2484814298548,0.208031110850763,-1.08333333333333));
#41777=CARTESIAN_POINT('Origin',(13.892722748591,-3.17092330887735,-1.08333333333333));
#41778=CARTESIAN_POINT('',(14.2484814298548,0.208031110850763,1.08333333333334));
#41779=CARTESIAN_POINT('Ctrl Pts',(14.2484814298548,0.208031110850764,1.08333333333334));
#41780=CARTESIAN_POINT('Ctrl Pts',(14.2468058395578,0.322795758952199,0.725928647976585));
#41781=CARTESIAN_POINT('Ctrl Pts',(14.2449910310593,0.377796936249431,0.352039859176993));
#41782=CARTESIAN_POINT('Ctrl Pts',(14.2449910310593,0.37779693624943,-0.352039859176987));
#41783=CARTESIAN_POINT('Ctrl Pts',(14.2468058395578,0.322795758952199,-0.725928647976577));
#41784=CARTESIAN_POINT('Ctrl Pts',(14.2484814298548,0.208031110850765,-1.08333333333333));
#41785=CARTESIAN_POINT('Origin',(13.892722748591,-3.17092330887735,1.08333333333334));
#41786=CARTESIAN_POINT('',(13.1366786991091,-6.48336872052383,1.08333333333334));
#41787=CARTESIAN_POINT('Origin',(13.892722748591,-3.17092330887735,3.20017169526122E-15));
#41788=CARTESIAN_POINT('',(12.7471768669564,-6.36961395396396,1.08333333333334));
#41789=CARTESIAN_POINT('Origin',(13.892722748591,-3.17092330887735,1.08333333333334));
#41790=CARTESIAN_POINT('',(12.7471768669564,-6.36961395396396,-1.08333333333333));
#41791=CARTESIAN_POINT('Ctrl Pts',(12.7471768669564,-6.36961395396397,-1.08333333333334));
#41792=CARTESIAN_POINT('Ctrl Pts',(12.6958726976266,-6.47228631765585,-0.725928647976583));
#41793=CARTESIAN_POINT('Ctrl Pts',(12.6703734952067,-6.52105325020152,-0.352039859176989));
#41794=CARTESIAN_POINT('Ctrl Pts',(12.6703734952067,-6.52105325020152,3.73360976135914E-15));
#41795=CARTESIAN_POINT('Ctrl Pts',(12.6703734952067,-6.52105325020152,0.352039859176996));
#41796=CARTESIAN_POINT('Ctrl Pts',(12.6958726976266,-6.47228631765585,0.725928647976591));
#41797=CARTESIAN_POINT('Ctrl Pts',(12.7471768669564,-6.36961395396397,1.08333333333335));
#41798=CARTESIAN_POINT('',(13.6476999686242,-6.55970790622078,-1.08333333333333));
#41799=CARTESIAN_POINT('Origin',(13.892722748591,-3.17092330887735,-1.08333333333333));
#41800=CARTESIAN_POINT('',(13.6476999686242,-6.55970790622078,1.08333333333334));
#41801=CARTESIAN_POINT('Ctrl Pts',(13.6476999686242,-6.55970790622078,1.08333333333334));
#41802=CARTESIAN_POINT('Ctrl Pts',(13.5948858118209,-6.66958959248674,0.727666221822799));
#41803=CARTESIAN_POINT('Ctrl Pts',(13.5683505740919,-6.72230205711255,0.35278297384278));
#41804=CARTESIAN_POINT('Ctrl Pts',(13.5683505740919,-6.72230205711255,3.93962482987281E-15));
#41805=CARTESIAN_POINT('Ctrl Pts',(13.5683505740919,-6.72230205711255,-0.352782973842771));
#41806=CARTESIAN_POINT('Ctrl Pts',(13.5948858118209,-6.66958959248674,-0.72766622182279));
#41807=CARTESIAN_POINT('Ctrl Pts',(13.6476999686242,-6.55970790622078,-1.08333333333333));
#41808=CARTESIAN_POINT('Origin',(13.892722748591,-3.17092330887735,1.08333333333334));
#41809=CARTESIAN_POINT('',(13.0227870731057,-2.97236616780865,-3.45272288248773));
#41810=CARTESIAN_POINT('Origin',(13.0227870731057,-2.97236616780865,2.9997830762867E-15));
#41811=CARTESIAN_POINT('',(14.7626584240763,-3.36948044994605,-3.45272288248773));
#41812=CARTESIAN_POINT('Origin',(14.7626584240763,-3.36948044994605,3.40056031423575E-15));
#41813=CARTESIAN_POINT('Origin',(11.1410986251693,8.88472967648709,9.85584169237555E-16));
#41814=CARTESIAN_POINT('',(11.8387328710639,9.44107442276104,3.96060240207311));
#41815=CARTESIAN_POINT('Origin',(11.8387328710639,9.44107442276104,1.0472995612114E-15));
#41816=CARTESIAN_POINT('',(10.4434643792748,8.32838493021314,3.96060240207311));
#41817=CARTESIAN_POINT('Origin',(11.1410986251693,8.88472967648709,2.5198520116158));
#41818=CARTESIAN_POINT('Origin',(10.4434643792748,8.32838493021314,9.23868777263706E-16));
#41819=CARTESIAN_POINT('',(8.89378902201275,12.2552029391784,-1.08333333331655));
#41820=CARTESIAN_POINT('',(8.89378902201677,12.2552029391754,1.08333333333333));
#41821=CARTESIAN_POINT('Ctrl Pts',(8.89378902201274,12.2552029391784,-1.08333333331655));
#41822=CARTESIAN_POINT('Ctrl Pts',(8.86335293025879,12.2772908784853,-0.956315399884826));
#41823=CARTESIAN_POINT('Ctrl Pts',(8.83824313040494,12.2953456493747,-0.827586922367285));
#41824=CARTESIAN_POINT('Ctrl Pts',(8.81859777764014,12.3094197866805,-0.69766772380084));
#41825=CARTESIAN_POINT('Ctrl Pts',(8.7991879276401,12.3233252073292,-0.569305958731489));
#41826=CARTESIAN_POINT('Ctrl Pts',(8.78511225071473,12.3333449381983,-0.439781849534452));
#41827=CARTESIAN_POINT('Ctrl Pts',(8.77647376760361,12.3394890678296,-0.309596747993595));
#41828=CARTESIAN_POINT('Ctrl Pts',(8.76964787761092,12.344343988818,-0.206728088024587));
#41829=CARTESIAN_POINT('Ctrl Pts',(8.76621624622163,12.3467783236357,-0.103446722778746));
#41830=CARTESIAN_POINT('Ctrl Pts',(8.76621624622163,12.3467783236357,-7.54951656745106E-15));
#41831=CARTESIAN_POINT('Ctrl Pts',(8.76621624622163,12.3467783236357,0.130951008152141));
#41832=CARTESIAN_POINT('Ctrl Pts',(8.77171477448527,12.3428797767713,0.261548325668487));
#41833=CARTESIAN_POINT('Ctrl Pts',(8.78261416841303,12.3351194002049,0.391301356121213));
#41834=CARTESIAN_POINT('Ctrl Pts',(8.79368558213778,12.3272365454154,0.523102215114213));
#41835=CARTESIAN_POINT('Ctrl Pts',(8.81032969837903,12.3153689336875,0.654031926803563));
#41836=CARTESIAN_POINT('Ctrl Pts',(8.83241243050519,12.2995110840219,0.783576297698762));
#41837=CARTESIAN_POINT('Ctrl Pts',(8.84960195907419,12.2871670969504,0.88441557119687));
#41838=CARTESIAN_POINT('Ctrl Pts',(8.87008627043973,12.2724043900869,0.984415425401903));
#41839=CARTESIAN_POINT('Ctrl Pts',(8.89378902201675,12.2552029391755,1.08333333333333));
#41840=CARTESIAN_POINT('',(8.22258343557123,11.6383685130292,1.08333333333333));
#41841=CARTESIAN_POINT('Ctrl Pts',(8.89378902201675,12.2552029391755,1.08333333333333));
#41842=CARTESIAN_POINT('Ctrl Pts',(8.78751907456219,12.2023537225759,1.08333333333333));
#41843=CARTESIAN_POINT('Ctrl Pts',(8.68681488082489,12.1369760343758,1.08333333333333));
#41844=CARTESIAN_POINT('Ctrl Pts',(8.46069343470621,11.9566501984405,1.08333333333333));
#41845=CARTESIAN_POINT('Ctrl Pts',(8.31988542322917,11.7983921800676,1.08333333333333));
#41846=CARTESIAN_POINT('Ctrl Pts',(8.22258343557176,11.6383685130289,1.08333333333333));
#41847=CARTESIAN_POINT('',(8.22258343557175,11.6383685130288,-1.08333333333333));
#41848=CARTESIAN_POINT('Ctrl Pts',(8.2225834355717,11.6383685130289,1.08333333333318));
#41849=CARTESIAN_POINT('Ctrl Pts',(8.19448780675769,11.6582182584498,0.949301954017324));
#41850=CARTESIAN_POINT('Ctrl Pts',(8.17159767874311,11.6742430454627,0.81366496302888));
#41851=CARTESIAN_POINT('Ctrl Pts',(8.15402161030241,11.6865063889394,0.67695567866062));
#41852=CARTESIAN_POINT('Ctrl Pts',(8.13658119548769,11.6986750828637,0.541301528447691));
#41853=CARTESIAN_POINT('Ctrl Pts',(8.12437307855494,11.7071402381473,0.40459157308691));
#41854=CARTESIAN_POINT('Ctrl Pts',(8.1174733585697,11.7119223986889,0.26734687734235));
#41855=CARTESIAN_POINT('Ctrl Pts',(8.11300215046573,11.7150213700985,0.178408544025479));
#41856=CARTESIAN_POINT('Ctrl Pts',(8.11075954642938,11.7165728598428,0.0892456520429063));
#41857=CARTESIAN_POINT('Ctrl Pts',(8.11075954642938,11.7165728598428,-1.33226762955019E-15));
#41858=CARTESIAN_POINT('Ctrl Pts',(8.11075954642938,11.7165728598428,-0.137335411050026));
#41859=CARTESIAN_POINT('Ctrl Pts',(8.11607262981309,11.7129002012938,-0.274553571737022));
#41860=CARTESIAN_POINT('Ctrl Pts',(8.12665801674411,11.7055512249056,-0.411127959090392));
#41861=CARTESIAN_POINT('Ctrl Pts',(8.13729388250879,11.698167203246,-0.548353632582512));
#41862=CARTESIAN_POINT('Ctrl Pts',(8.15325248641432,11.6870716767896,-0.684929378140945));
#41863=CARTESIAN_POINT('Ctrl Pts',(8.17446212457132,11.6722178258439,-0.820321104282498));
#41864=CARTESIAN_POINT('Ctrl Pts',(8.18828255682692,11.6625388940673,-0.908543834215877));
#41865=CARTESIAN_POINT('Ctrl Pts',(8.20433194575505,11.6512633098961,-0.9962638332735));
#41866=CARTESIAN_POINT('Ctrl Pts',(8.22258343557176,11.6383685130288,-1.08333333333334));
#41867=CARTESIAN_POINT('Ctrl Pts',(8.89378902201473,12.2552029391744,-1.08333333333333));
#41868=CARTESIAN_POINT('Ctrl Pts',(8.7875190745609,12.202353722575,-1.08333333333333));
#41869=CARTESIAN_POINT('Ctrl Pts',(8.68681488082435,12.1369760343753,-1.08333333333333));
#41870=CARTESIAN_POINT('Ctrl Pts',(8.46069343470619,11.9566501984405,-1.08333333333333));
#41871=CARTESIAN_POINT('Ctrl Pts',(8.31988542322913,11.7983921800676,-1.08333333333333));
#41872=CARTESIAN_POINT('Ctrl Pts',(8.22258343557172,11.6383685130288,-1.08333333333333));
#41873=CARTESIAN_POINT('',(13.9269936544443,5.94376395877129,-1.08333333333333));
#41874=CARTESIAN_POINT('',(13.1762672612271,5.42664547033562,-1.08333333333333));
#41875=CARTESIAN_POINT('Ctrl Pts',(13.9269936544443,5.94376395877129,-1.08333333333333));
#41876=CARTESIAN_POINT('Ctrl Pts',(13.8517896638478,5.85187873682469,-1.08333333333333));
#41877=CARTESIAN_POINT('Ctrl Pts',(13.7657237213495,5.76832601371371,-1.08333333333333));
#41878=CARTESIAN_POINT('Ctrl Pts',(13.5395781511316,5.5879809394513,-1.08333333333333));
#41879=CARTESIAN_POINT('Ctrl Pts',(13.3544742809805,5.48608062863226,-1.08333333333333));
#41880=CARTESIAN_POINT('Ctrl Pts',(13.1762672612269,5.42664547033621,-1.08333333333333));
#41881=CARTESIAN_POINT('',(13.1762672612355,5.42664547033908,1.08333333333333));
#41882=CARTESIAN_POINT('Ctrl Pts',(13.1762672612269,5.42664547033617,1.08333333333318));
#41883=CARTESIAN_POINT('Ctrl Pts',(13.1893705593041,5.39482976422236,0.949270311030452));
#41884=CARTESIAN_POINT('Ctrl Pts',(13.1999097963792,5.36892368585892,0.813521288368082));
#41885=CARTESIAN_POINT('Ctrl Pts',(13.2079621630868,5.34904061477083,0.676607052101254));
#41886=CARTESIAN_POINT('Ctrl Pts',(13.2148460430323,5.33204279546023,0.559560573777983));
#41887=CARTESIAN_POINT('Ctrl Pts',(13.2199117356377,5.31944645364959,0.441662516279123));
#41888=CARTESIAN_POINT('Ctrl Pts',(13.2231796369647,5.31131059989547,0.323238258334714));
#41889=CARTESIAN_POINT('Ctrl Pts',(13.2269557156993,5.30190957419912,0.186398348762647));
#41890=CARTESIAN_POINT('Ctrl Pts',(13.2283213471703,5.2984924131362,0.0492519096262126));
#41891=CARTESIAN_POINT('Ctrl Pts',(13.2273014856384,5.30103720115497,-0.087675827066048));
#41892=CARTESIAN_POINT('Ctrl Pts',(13.2262786675026,5.30358936657715,-0.225000520654307));
#41893=CARTESIAN_POINT('Ctrl Pts',(13.22285647475,5.31213809759657,-0.362105241912749));
#41894=CARTESIAN_POINT('Ctrl Pts',(13.2170113253899,5.32664168351083,-0.498460177595588));
#41895=CARTESIAN_POINT('Ctrl Pts',(13.2111409592133,5.34120783998435,-0.635403368116607));
#41896=CARTESIAN_POINT('Ctrl Pts',(13.2028266475275,5.36178038996296,-0.771590289741134));
#41897=CARTESIAN_POINT('Ctrl Pts',(13.1919958930594,5.38829698119018,-0.906484242526414));
#41898=CARTESIAN_POINT('Ctrl Pts',(13.1872415508606,5.3999368857798,-0.965698216399684));
#41899=CARTESIAN_POINT('Ctrl Pts',(13.1820016856381,5.41272189470467,-1.02466304565381));
#41900=CARTESIAN_POINT('Ctrl Pts',(13.1762672612269,5.42664547033617,-1.08333333333318));
#41901=CARTESIAN_POINT('',(13.9269936544443,5.94376395877129,1.08333333333333));
#41902=CARTESIAN_POINT('Ctrl Pts',(13.9269936544443,5.94376395877129,1.08333333333333));
#41903=CARTESIAN_POINT('Ctrl Pts',(13.8517896638478,5.85187873682469,1.08333333333333));
#41904=CARTESIAN_POINT('Ctrl Pts',(13.7657237213495,5.76832601371371,1.08333333333333));
#41905=CARTESIAN_POINT('Ctrl Pts',(13.5395781511339,5.5879809394531,1.08333333333333));
#41906=CARTESIAN_POINT('Ctrl Pts',(13.3544742809865,5.48608062863536,1.08333333333333));
#41907=CARTESIAN_POINT('Ctrl Pts',(13.1762672612355,5.42664547033908,1.08333333333333));
#41908=CARTESIAN_POINT('Ctrl Pts',(13.9269936544443,5.9437639587713,-1.08333333333333));
#41909=CARTESIAN_POINT('Ctrl Pts',(13.9416885168395,5.90933203032488,-0.95688863210334));
#41910=CARTESIAN_POINT('Ctrl Pts',(13.9536527109305,5.88095561854266,-0.828820583351241));
#41911=CARTESIAN_POINT('Ctrl Pts',(13.9629765258053,5.85873440158633,-0.699646919261855));
#41912=CARTESIAN_POINT('Ctrl Pts',(13.9722513158077,5.83663002439342,-0.571152453813261));
#41913=CARTESIAN_POINT('Ctrl Pts',(13.9789135007645,5.82061622745854,-0.441563969171658));
#41914=CARTESIAN_POINT('Ctrl Pts',(13.9830050237944,5.81077040959811,-0.31139107363785));
#41915=CARTESIAN_POINT('Ctrl Pts',(13.987063711968,5.80100360535004,-0.182262827807452));
#41916=CARTESIAN_POINT('Ctrl Pts',(13.9885928700522,5.79730615639857,-0.0525595133520559));
#41917=CARTESIAN_POINT('Ctrl Pts',(13.9875862925321,5.79973378332923,0.077221432194654));
#41918=CARTESIAN_POINT('Ctrl Pts',(13.9868997670033,5.80138952054645,0.165737150534494));
#41919=CARTESIAN_POINT('Ctrl Pts',(13.9850326975557,5.80589410253397,0.254288981130278));
#41920=CARTESIAN_POINT('Ctrl Pts',(13.9819702480148,5.81325986277498,0.342719102199545));
#41921=CARTESIAN_POINT('Ctrl Pts',(13.977353348451,5.82436436418423,0.476034927301432));
#41922=CARTESIAN_POINT('Ctrl Pts',(13.9700489046451,5.84190742581571,0.608312350205104));
#41923=CARTESIAN_POINT('Ctrl Pts',(13.9600480872369,5.86570879353505,0.739057191236667));
#41924=CARTESIAN_POINT('Ctrl Pts',(13.9511688384277,5.88684089277784,0.855139299993628));
#41925=CARTESIAN_POINT('Ctrl Pts',(13.9401632237805,5.91290598563348,0.970013302477476));
#41926=CARTESIAN_POINT('Ctrl Pts',(13.9269936544443,5.9437639587713,1.08333333333333));
#41927=CARTESIAN_POINT('Origin',(11.1410986251693,8.88472967648709,9.85584169237555E-16));
#41928=CARTESIAN_POINT('',(8.72113759169208,11.2696166353064,1.08333333333333));
#41929=CARTESIAN_POINT('',(9.02271027299523,11.54110464988,1.08333333333333));
#41930=CARTESIAN_POINT('Origin',(11.1410986251693,8.88472967648709,1.08333333333333));
#41931=CARTESIAN_POINT('',(13.2594869773434,6.22835470309422,1.08333333333333));
#41932=CARTESIAN_POINT('Origin',(11.1410986251693,8.88472967648709,9.85584169237555E-16));
#41933=CARTESIAN_POINT('',(12.9276994994135,5.9947548451011,1.08333333333333));
#41934=CARTESIAN_POINT('Origin',(11.1410986251693,8.88472967648709,1.08333333333333));
#41935=CARTESIAN_POINT('',(12.9276994994135,5.9947548451011,-1.08333333333333));
#41936=CARTESIAN_POINT('Ctrl Pts',(12.9276994994135,5.9947548451011,-1.08333333333333));
#41937=CARTESIAN_POINT('Ctrl Pts',(12.9759843593573,5.89062845864264,-0.725928647976581));
#41938=CARTESIAN_POINT('Ctrl Pts',(12.9982133898606,5.84028669430273,-0.352039859176989));
#41939=CARTESIAN_POINT('Ctrl Pts',(12.9982133898606,5.84028669430273,9.85141416048961E-16));
#41940=CARTESIAN_POINT('Ctrl Pts',(12.9982133898606,5.84028669430273,0.35203985917699));
#41941=CARTESIAN_POINT('Ctrl Pts',(12.9759843593573,5.89062845864264,0.72592864797658));
#41942=CARTESIAN_POINT('Ctrl Pts',(12.9276994994135,5.9947548451011,1.08333333333333));
#41943=CARTESIAN_POINT('',(13.6377879061428,6.58029051604763,-1.08333333333333));
#41944=CARTESIAN_POINT('Origin',(11.1410986251693,8.88472967648709,-1.08333333333333));
#41945=CARTESIAN_POINT('',(13.6377879061428,6.58029051604763,1.08333333333333));
#41946=CARTESIAN_POINT('Ctrl Pts',(13.6377879061428,6.58029051604764,1.08333333333332));
#41947=CARTESIAN_POINT('Ctrl Pts',(13.6907677796515,6.47048863474093,0.727666221822788));
#41948=CARTESIAN_POINT('Ctrl Pts',(13.7154355939006,6.41687686636464,0.352782973842773));
#41949=CARTESIAN_POINT('Ctrl Pts',(13.7154355939006,6.41687686636464,9.86054494281319E-16));
#41950=CARTESIAN_POINT('Ctrl Pts',(13.7154355939006,6.41687686636464,-0.352782973842772));
#41951=CARTESIAN_POINT('Ctrl Pts',(13.6907677796515,6.47048863474094,-0.727666221822788));
#41952=CARTESIAN_POINT('Ctrl Pts',(13.6377879061428,6.58029051604764,-1.08333333333332));
#41953=CARTESIAN_POINT('Origin',(11.1410986251693,8.88472967648709,1.08333333333333));
#41954=CARTESIAN_POINT('',(9.4500021963329,11.8316076987797,1.08333333333333));
#41955=CARTESIAN_POINT('Origin',(11.1410986251693,8.88472967648709,1.08333333333333));
#41956=CARTESIAN_POINT('',(9.4500021963329,11.8316076987797,-1.08333333333333));
#41957=CARTESIAN_POINT('Ctrl Pts',(9.4500021963329,11.8316076987798,1.08333333333334));
#41958=CARTESIAN_POINT('Ctrl Pts',(9.35474240837097,11.9076924734258,0.7276662218228));
#41959=CARTESIAN_POINT('Ctrl Pts',(9.30796390402485,11.9436715548399,0.352782973842779));
#41960=CARTESIAN_POINT('Ctrl Pts',(9.30796390402485,11.9436715548399,-0.352782973842777));
#41961=CARTESIAN_POINT('Ctrl Pts',(9.35474240837097,11.9076924734258,-0.7276662218228));
#41962=CARTESIAN_POINT('Ctrl Pts',(9.4500021963329,11.8316076987798,-1.08333333333334));
#41963=CARTESIAN_POINT('',(8.72113759169208,11.2696166353064,-1.08333333333333));
#41964=CARTESIAN_POINT('Origin',(11.1410986251693,8.88472967648709,-1.08333333333333));
#41965=CARTESIAN_POINT('Ctrl Pts',(8.72113759169207,11.2696166353064,-1.08333333333334));
#41966=CARTESIAN_POINT('Ctrl Pts',(8.63036626326973,11.3398611937657,-0.725928647976583));
#41967=CARTESIAN_POINT('Ctrl Pts',(8.5862330966948,11.3727349924819,-0.35203985917699));
#41968=CARTESIAN_POINT('Ctrl Pts',(8.5862330966948,11.3727349924819,0.352039859176991));
#41969=CARTESIAN_POINT('Ctrl Pts',(8.63036626326973,11.3398611937657,0.725928647976584));
#41970=CARTESIAN_POINT('Ctrl Pts',(8.72113759169207,11.2696166353064,1.08333333333334));
#41971=CARTESIAN_POINT('',(10.4434643792748,8.32838493021314,-3.45272288248773));
#41972=CARTESIAN_POINT('Origin',(10.4434643792748,8.32838493021314,9.23868777263706E-16));
#41973=CARTESIAN_POINT('',(11.8387328710639,9.44107442276105,-3.45272288248773));
#41974=CARTESIAN_POINT('Origin',(11.8387328710639,9.44107442276104,1.0472995612114E-15));
#41975=CARTESIAN_POINT('Origin',(0.,14.25,0.));
#41976=CARTESIAN_POINT('',(-3.35834339016074,14.7651959662676,1.08333333333333));
#41977=CARTESIAN_POINT('',(-3.39763111739558,14.25,1.08333333333333));
#41978=CARTESIAN_POINT('Origin',(1.55588456152529E-16,14.25,1.08333333333333));
#41979=CARTESIAN_POINT('',(-3.35834339016074,14.7651959662676,-1.08333333333333));
#41980=CARTESIAN_POINT('Ctrl Pts',(-3.35834339016074,14.7651959662676,-1.08333333333333));
#41981=CARTESIAN_POINT('Ctrl Pts',(-3.47722236863702,14.7381569460943,-0.727666221822795));
#41982=CARTESIAN_POINT('Ctrl Pts',(-3.53451786760282,14.7240166290356,-0.352782973842776));
#41983=CARTESIAN_POINT('Ctrl Pts',(-3.53451786760282,14.7240166290356,0.352782973842775));
#41984=CARTESIAN_POINT('Ctrl Pts',(-3.47722236863702,14.7381569460943,0.727666221822794));
#41985=CARTESIAN_POINT('Ctrl Pts',(-3.35834339016074,14.7651959662676,1.08333333333333));
#41986=CARTESIAN_POINT('',(-3.37340073180097,13.8449509750914,-1.08333333333333));
#41987=CARTESIAN_POINT('Origin',(-1.5558845615253E-16,14.25,-1.08333333333333));
#41988=CARTESIAN_POINT('',(-3.37340073180097,13.8449509750914,1.08333333333333));
#41989=CARTESIAN_POINT('Ctrl Pts',(-3.37340073180098,13.8449509750914,1.08333333333333));
#41990=CARTESIAN_POINT('Ctrl Pts',(-3.48491513664897,13.8177798586608,0.725928647976578));
#41991=CARTESIAN_POINT('Ctrl Pts',(-3.53813348671686,13.8037716378594,0.352039859176988));
#41992=CARTESIAN_POINT('Ctrl Pts',(-3.53813348671686,13.8037716378594,-0.352039859176988));
#41993=CARTESIAN_POINT('Ctrl Pts',(-3.48491513664897,13.8177798586608,-0.725928647976578));
#41994=CARTESIAN_POINT('Ctrl Pts',(-3.37340073180098,13.8449509750914,-1.08333333333333));
#41995=CARTESIAN_POINT('Origin',(1.55588456152529E-16,14.25,1.08333333333333));
#41996=CARTESIAN_POINT('',(3.39763111739558,14.25,1.08333333333333));
#41997=CARTESIAN_POINT('Origin',(0.,14.25,0.));
#41998=CARTESIAN_POINT('',(3.37340073180097,13.8449509750914,1.08333333333333));
#41999=CARTESIAN_POINT('Origin',(0.,14.25,1.08333333333333));
#42000=CARTESIAN_POINT('',(3.37340073180097,13.8449509750914,-1.08333333333333));
#42001=CARTESIAN_POINT('Ctrl Pts',(3.37340073180098,13.8449509750914,-1.08333333333333));
#42002=CARTESIAN_POINT('Ctrl Pts',(3.48491513664897,13.8177798586608,-0.725928647976578));
#42003=CARTESIAN_POINT('Ctrl Pts',(3.53813348671686,13.8037716378594,-0.352039859176988));
#42004=CARTESIAN_POINT('Ctrl Pts',(3.53813348671686,13.8037716378594,0.));
#42005=CARTESIAN_POINT('Ctrl Pts',(3.53813348671686,13.8037716378594,0.352039859176988));
#42006=CARTESIAN_POINT('Ctrl Pts',(3.48491513664897,13.8177798586608,0.725928647976578));
#42007=CARTESIAN_POINT('Ctrl Pts',(3.37340073180098,13.8449509750914,1.08333333333333));
#42008=CARTESIAN_POINT('',(3.35834339016074,14.7651959662676,-1.08333333333333));
#42009=CARTESIAN_POINT('Origin',(0.,14.25,-1.08333333333333));
#42010=CARTESIAN_POINT('',(3.35834339016074,14.7651959662676,1.08333333333333));
#42011=CARTESIAN_POINT('Ctrl Pts',(3.35834339016074,14.7651959662676,1.08333333333333));
#42012=CARTESIAN_POINT('Ctrl Pts',(3.47722236863702,14.7381569460943,0.727666221822794));
#42013=CARTESIAN_POINT('Ctrl Pts',(3.53451786760282,14.7240166290356,0.352782973842775));
#42014=CARTESIAN_POINT('Ctrl Pts',(3.53451786760282,14.7240166290356,0.));
#42015=CARTESIAN_POINT('Ctrl Pts',(3.53451786760282,14.7240166290356,-0.352782973842775));
#42016=CARTESIAN_POINT('Ctrl Pts',(3.47722236863702,14.7381569460943,-0.727666221822793));
#42017=CARTESIAN_POINT('Ctrl Pts',(3.35834339016074,14.7651959662676,-1.08333333333333));
#42018=CARTESIAN_POINT('Origin',(0.,14.25,1.08333333333333));
#42019=CARTESIAN_POINT('',(0.,13.3576923076923,-3.45272288248773));
#42020=CARTESIAN_POINT('Origin',(0.,13.3576923076923,0.));
#42021=CARTESIAN_POINT('',(0.,15.1423076923077,-3.45272288248773));
#42022=CARTESIAN_POINT('Origin',(0.,15.1423076923077,0.));
#42023=CARTESIAN_POINT('Origin',(0.,14.25,0.));
#42024=CARTESIAN_POINT('',(-4.85033905439415E-16,15.1423076923077,3.96060240207311));
#42025=CARTESIAN_POINT('Origin',(0.,15.1423076923077,0.));
#42026=CARTESIAN_POINT('',(-4.85033905439415E-16,13.3576923076923,3.96060240207311));
#42027=CARTESIAN_POINT('Origin',(3.08592870035031E-16,14.25,2.5198520116158));
#42028=CARTESIAN_POINT('Origin',(0.,13.3576923076923,0.));
#42029=CARTESIAN_POINT('',(-3.97254599103887,13.6850786752975,-1.08333333333333));
#42030=CARTESIAN_POINT('',(-4.03631672677061,14.5944383081266,-1.08333333333333));
#42031=CARTESIAN_POINT('Ctrl Pts',(-3.97254599103889,13.6850786752975,-1.08333333333333));
#42032=CARTESIAN_POINT('Ctrl Pts',(-4.03699073486477,13.8609255570095,-1.08333333333333));
#42033=CARTESIAN_POINT('Ctrl Pts',(-4.07292947680577,14.0696859538838,-1.08333333333333));
#42034=CARTESIAN_POINT('Ctrl Pts',(-4.07292947680577,14.358906139038,-1.08333333333333));
#42035=CARTESIAN_POINT('Ctrl Pts',(-4.06125577389194,14.4784021699804,-1.08333333333333));
#42036=CARTESIAN_POINT('Ctrl Pts',(-4.03631672677123,14.5944383081267,-1.08333333333333));
#42037=CARTESIAN_POINT('',(-4.03631672677098,14.5944383081279,1.08333333333333));
#42038=CARTESIAN_POINT('Ctrl Pts',(-4.03631672677125,14.5944383081264,1.08333333333353));
#42039=CARTESIAN_POINT('Ctrl Pts',(-4.07239878927587,14.5844592579328,0.956888632103535));
#42040=CARTESIAN_POINT('Ctrl Pts',(-4.10204391436992,14.576120838176,0.828820583351431));
#42041=CARTESIAN_POINT('Ctrl Pts',(-4.12523046485396,14.5695557880246,0.699646919262042));
#42042=CARTESIAN_POINT('Ctrl Pts',(-4.14829509982461,14.5630252570856,0.571152453813459));
#42043=CARTESIAN_POINT('Ctrl Pts',(-4.16496899480084,14.5582495239489,0.441563969171867));
#42044=CARTESIAN_POINT('Ctrl Pts',(-4.17521778805797,14.555309638438,0.311391073638072));
#42045=CARTESIAN_POINT('Ctrl Pts',(-4.18538433378736,14.5523933457842,0.182262827807668));
#42046=CARTESIAN_POINT('Ctrl Pts',(-4.18922853025337,14.5512835680019,0.0525595133522669));
#42047=CARTESIAN_POINT('Ctrl Pts',(-4.18670294427272,14.5520101946411,-0.0772214321944475));
#42048=CARTESIAN_POINT('Ctrl Pts',(-4.18498039512374,14.5525057826387,-0.165737150534356));
#42049=CARTESIAN_POINT('Ctrl Pts',(-4.1802944723506,14.5538546098955,-0.254288981130209));
#42050=CARTESIAN_POINT('Ctrl Pts',(-4.17262628304436,14.5560527668241,-0.342719102199544));
#42051=CARTESIAN_POINT('Ctrl Pts',(-4.16106584445129,14.5593666727772,-0.476034927301542));
#42052=CARTESIAN_POINT('Ctrl Pts',(-4.14279588034764,14.5645937486684,-0.608312350205319));
#42053=CARTESIAN_POINT('Ctrl Pts',(-4.11795181407459,14.5716147048116,-0.739057191236983));
#42054=CARTESIAN_POINT('Ctrl Pts',(-4.09589395251526,14.5778482769217,-0.855139299993905));
#42055=CARTESIAN_POINT('Ctrl Pts',(-4.06865355383155,14.5854950604866,-0.970013302477714));
#42056=CARTESIAN_POINT('Ctrl Pts',(-4.03631672677125,14.5944383081264,-1.08333333333353));
#42057=CARTESIAN_POINT('',(-3.97254599103887,13.6850786752975,1.08333333333333));
#42058=CARTESIAN_POINT('Ctrl Pts',(-3.97254599103889,13.6850786752975,1.08333333333333));
#42059=CARTESIAN_POINT('Ctrl Pts',(-4.03718797255354,13.8614637488071,1.08333333333333));
#42060=CARTESIAN_POINT('Ctrl Pts',(-4.07292947680577,14.0697175866198,1.08333333333333));
#42061=CARTESIAN_POINT('Ctrl Pts',(-4.07292947680577,14.3589686276554,1.08333333333333));
#42062=CARTESIAN_POINT('Ctrl Pts',(-4.06126656486658,14.4783519618466,1.08333333333333));
#42063=CARTESIAN_POINT('Ctrl Pts',(-4.03631672677098,14.5944383081279,1.08333333333333));
#42064=CARTESIAN_POINT('Ctrl Pts',(-3.97254599103885,13.6850786752975,-1.08333333333333));
#42065=CARTESIAN_POINT('Ctrl Pts',(-4.0055902844374,13.6754864779574,-0.949270311030653));
#42066=CARTESIAN_POINT('Ctrl Pts',(-4.03241557892495,13.6675742096383,-0.813521288368336));
#42067=CARTESIAN_POINT('Ctrl Pts',(-4.05298135839275,13.6614729113855,-0.67660705210156));
#42068=CARTESIAN_POINT('Ctrl Pts',(-4.07056281760631,13.6562569784544,-0.559560573778188));
#42069=CARTESIAN_POINT('Ctrl Pts',(-4.08356944187665,13.6523638057542,-0.441662516279225));
#42070=CARTESIAN_POINT('Ctrl Pts',(-4.09196781162929,13.6498461320482,-0.32323825833471));
#42071=CARTESIAN_POINT('Ctrl Pts',(-4.10167217606822,13.6469369456345,-0.186398348762652));
#42072=CARTESIAN_POINT('Ctrl Pts',(-4.10519527746315,13.6458740742379,-0.0492519096262281));
#42073=CARTESIAN_POINT('Ctrl Pts',(-4.1025698088094,13.6466633637621,0.0876758270660229));
#42074=CARTESIAN_POINT('Ctrl Pts',(-4.09993672885708,13.6474549414561,0.225000520654293));
#42075=CARTESIAN_POINT('Ctrl Pts',(-4.0911193595297,13.6501094100325,0.362105241912746));
#42076=CARTESIAN_POINT('Ctrl Pts',(-4.07613560843688,13.6545823261509,0.498460177595596));
#42077=CARTESIAN_POINT('Ctrl Pts',(-4.06108721528303,13.659074539074,0.635403368116582));
#42078=CARTESIAN_POINT('Ctrl Pts',(-4.03981905948952,13.6654009235528,0.771590289741077));
#42079=CARTESIAN_POINT('Ctrl Pts',(-4.01233468870309,13.673465922941,0.906484242526326));
#42080=CARTESIAN_POINT('Ctrl Pts',(-4.00026996096645,13.6770061903378,0.965698216399675));
#42081=CARTESIAN_POINT('Ctrl Pts',(-3.98700723595603,13.6808808214243,1.02466304565388));
#42082=CARTESIAN_POINT('Ctrl Pts',(-3.97254599103885,13.6850786752975,1.08333333333333));
#42083=CARTESIAN_POINT('',(4.0363167267713,14.5944383081264,-1.08333333333333));
#42084=CARTESIAN_POINT('',(3.97254599103947,13.6850786752973,-1.08333333333333));
#42085=CARTESIAN_POINT('Ctrl Pts',(4.0363167267713,14.5944383081264,-1.08333333333333));
#42086=CARTESIAN_POINT('Ctrl Pts',(4.06125577389196,14.4784021699801,-1.08333333333333));
#42087=CARTESIAN_POINT('Ctrl Pts',(4.07292947680577,14.3589061390379,-1.08333333333333));
#42088=CARTESIAN_POINT('Ctrl Pts',(4.07292947680577,14.0696859538838,-1.08333333333333));
#42089=CARTESIAN_POINT('Ctrl Pts',(4.03699073486477,13.8609255570095,-1.08333333333333));
#42090=CARTESIAN_POINT('Ctrl Pts',(3.97254599103889,13.6850786752975,-1.08333333333333));
#42091=CARTESIAN_POINT('',(3.972545991042,13.685078675306,1.08333333333333));
#42092=CARTESIAN_POINT('Ctrl Pts',(3.97254599103891,13.6850786752974,1.08333333333318));
#42093=CARTESIAN_POINT('Ctrl Pts',(4.00550358468898,13.6755116454224,0.949622058007565));
#42094=CARTESIAN_POINT('Ctrl Pts',(4.03223833992508,13.667626413385,0.814376693553222));
#42095=CARTESIAN_POINT('Ctrl Pts',(4.05275116551691,13.6615412011384,0.678132403728152));
#42096=CARTESIAN_POINT('Ctrl Pts',(4.07316650047532,13.6554849098804,0.542535637670838));
#42097=CARTESIAN_POINT('Ctrl Pts',(4.0874189867075,13.6512115628239,0.40594941879892));
#42098=CARTESIAN_POINT('Ctrl Pts',(4.09549564973878,13.6487880554638,0.268901316711817));
#42099=CARTESIAN_POINT('Ctrl Pts',(4.10076932144717,13.6472056219574,0.179415511018788));
#42100=CARTESIAN_POINT('Ctrl Pts',(4.10340966592831,13.6464108509735,0.0897327832366672));
#42101=CARTESIAN_POINT('Ctrl Pts',(4.10340966592831,13.6464108509735,-4.66293670342566E-15));
#42102=CARTESIAN_POINT('Ctrl Pts',(4.10340966592831,13.6464108509735,-0.137573936980382));
#42103=CARTESIAN_POINT('Ctrl Pts',(4.09720533291532,13.6482810316174,-0.274951212619736));
#42104=CARTESIAN_POINT('Ctrl Pts',(4.08483748845152,13.6519816397819,-0.41161240621476));
#42105=CARTESIAN_POINT('Ctrl Pts',(4.07237395114171,13.6557108803995,-0.549330978772818));
#42106=CARTESIAN_POINT('Ctrl Pts',(4.05365110225785,13.6612989721827,-0.686322345436846));
#42107=CARTESIAN_POINT('Ctrl Pts',(4.02869583028489,13.6686542829587,-0.822054935347102));
#42108=CARTESIAN_POINT('Ctrl Pts',(4.01257796374822,13.6734048590114,-0.909720570537157));
#42109=CARTESIAN_POINT('Ctrl Pts',(3.99385994844905,13.6788915953345,-0.996861109122728));
#42110=CARTESIAN_POINT('Ctrl Pts',(3.97254599103891,13.6850786752974,-1.08333333333318));
#42111=CARTESIAN_POINT('',(4.0363167267713,14.5944383081264,1.08333333333333));
#42112=CARTESIAN_POINT('Ctrl Pts',(4.0363167267713,14.5944383081264,1.08333333333333));
#42113=CARTESIAN_POINT('Ctrl Pts',(4.06125577389196,14.4784021699801,1.08333333333333));
#42114=CARTESIAN_POINT('Ctrl Pts',(4.07292947680577,14.3589061390379,1.08333333333333));
#42115=CARTESIAN_POINT('Ctrl Pts',(4.07292947680577,14.0696859538867,1.08333333333333));
#42116=CARTESIAN_POINT('Ctrl Pts',(4.03699073486612,13.8609255570161,1.08333333333333));
#42117=CARTESIAN_POINT('Ctrl Pts',(3.97254599104201,13.685078675306,1.08333333333333));
#42118=CARTESIAN_POINT('Ctrl Pts',(4.0363167267713,14.5944383081264,-1.08333333333333));
#42119=CARTESIAN_POINT('Ctrl Pts',(4.07267660468553,14.5843824238018,-0.955915065626592));
#42120=CARTESIAN_POINT('Ctrl Pts',(4.10254364280131,14.5759803979714,-0.826701571450557));
#42121=CARTESIAN_POINT('Ctrl Pts',(4.12584816889326,14.5693808768856,-0.696211209492171));
#42122=CARTESIAN_POINT('Ctrl Pts',(4.14878536602558,14.5628853783063,-0.567777653525462));
#42123=CARTESIAN_POINT('Ctrl Pts',(4.16536539316191,14.5581360328796,-0.438107164856169));
#42124=CARTESIAN_POINT('Ctrl Pts',(4.17550906341001,14.5552260824043,-0.307693975181436));
#42125=CARTESIAN_POINT('Ctrl Pts',(4.18345734283739,14.55294593144,-0.205506064179161));
#42126=CARTESIAN_POINT('Ctrl Pts',(4.18745357006455,14.5517942140162,-0.102862147740973));
#42127=CARTESIAN_POINT('Ctrl Pts',(4.18745357006455,14.5517942140162,4.44089209850063E-16));
#42128=CARTESIAN_POINT('Ctrl Pts',(4.18745357006455,14.5517942140162,0.13066680730557));
#42129=CARTESIAN_POINT('Ctrl Pts',(4.18100368362964,14.5536548201376,0.261069786498731));
#42130=CARTESIAN_POINT('Ctrl Pts',(4.16817103415993,14.5573291670729,0.390710450871123));
#42131=CARTESIAN_POINT('Ctrl Pts',(4.15518429935153,14.561047632956,0.521907748246283));
#42132=CARTESIAN_POINT('Ctrl Pts',(4.13566054561854,14.5666236366129,0.652324314224272));
#42133=CARTESIAN_POINT('Ctrl Pts',(4.10965488440249,14.5739568744946,0.781443489202978));
#42134=CARTESIAN_POINT('Ctrl Pts',(4.08920880779353,14.5797223861759,0.882959098491578));
#42135=CARTESIAN_POINT('Ctrl Pts',(4.06475571708163,14.586573067282,0.983672743459539));
#42136=CARTESIAN_POINT('Ctrl Pts',(4.0363167267713,14.5944383081264,1.08333333333333));
#42137=CARTESIAN_POINT('Origin',(0.,0.,-1.08333333333333));
#42138=CARTESIAN_POINT('Origin',(0.,0.,1.08333333333333));
#42139=CARTESIAN_POINT('Origin',(0.,0.,-1.08333333333333));
#42140=CARTESIAN_POINT('Origin',(0.,0.,-1.08333333333333));
#42141=CARTESIAN_POINT('Origin',(0.,0.,-1.08333333333333));
#42142=CARTESIAN_POINT('Origin',(0.,0.,1.08333333333333));
#42143=CARTESIAN_POINT('Origin',(0.,0.,-1.08333333333333));
#42144=CARTESIAN_POINT('Origin',(0.,0.,1.08333333333333));
#42145=CARTESIAN_POINT('Origin',(0.,15.1423076923077,-3.45272288248773));
#42146=CARTESIAN_POINT('Origin',(0.,13.3576923076923,-3.45272288248773));
#42147=CARTESIAN_POINT('Origin',(0.,0.,-1.08333333333333));
#42148=CARTESIAN_POINT('Origin',(0.,0.,-1.08333333333333));
#42149=CARTESIAN_POINT('Origin',(0.,0.,-1.08333333333333));
#42150=CARTESIAN_POINT('Origin',(0.,0.,1.08333333333333));
#42151=CARTESIAN_POINT('Origin',(0.,0.,1.08333333333333));
#42152=CARTESIAN_POINT('Origin',(0.,0.,1.08333333333333));
#42153=CARTESIAN_POINT('Origin',(0.,0.,-1.08333333333333));
#42154=CARTESIAN_POINT('Origin',(0.,0.,-1.08333333333333));
#42155=CARTESIAN_POINT('Origin',(10.4434643792748,8.32838493021314,-3.45272288248773));
#42156=CARTESIAN_POINT('Origin',(11.8387328710639,9.44107442276104,-3.45272288248773));
#42157=CARTESIAN_POINT('Origin',(-1.55588456152528E-16,7.49274514625042E-17,
1.08333333333333));
#42158=CARTESIAN_POINT('Origin',(-1.55588456152528E-16,7.49274514625042E-17,
1.08333333333333));
#42159=CARTESIAN_POINT('Origin',(-1.55588456152528E-16,7.49274514625042E-17,
1.08333333333333));
#42160=CARTESIAN_POINT('Origin',(1.55588456152528E-16,-7.49274514625042E-17,
-1.08333333333333));
#42161=CARTESIAN_POINT('Origin',(1.55588456152528E-16,-7.49274514625042E-17,
-1.08333333333333));
#42162=CARTESIAN_POINT('Origin',(1.55588456152528E-16,-7.49274514625042E-17,
-1.08333333333333));
#42163=CARTESIAN_POINT('Origin',(1.55588456152528E-16,-7.49274514625042E-17,
-1.08333333333333));
#42164=CARTESIAN_POINT('Origin',(1.55588456152528E-16,-7.49274514625042E-17,
-1.08333333333333));
#42165=CARTESIAN_POINT('Origin',(1.94015631396094E-16,-2.43287906657286E-16,
-1.08333333333333));
#42166=CARTESIAN_POINT('Origin',(-1.94015631396094E-16,2.43287906657286E-16,
1.08333333333333));
#42167=CARTESIAN_POINT('Origin',(1.94015631396094E-16,-2.43287906657286E-16,
-1.08333333333333));
#42168=CARTESIAN_POINT('Origin',(1.94015631396094E-16,-2.43287906657286E-16,
-1.08333333333333));
#42169=CARTESIAN_POINT('Origin',(1.94015631396094E-16,-2.43287906657286E-16,
-1.08333333333333));
#42170=CARTESIAN_POINT('Origin',(-1.94015631396094E-16,2.43287906657286E-16,
1.08333333333333));
#42171=CARTESIAN_POINT('Origin',(-1.94015631396094E-16,2.43287906657286E-16,
1.08333333333333));
#42172=CARTESIAN_POINT('Origin',(1.94015631396094E-16,-2.43287906657286E-16,
-1.08333333333333));
#42173=CARTESIAN_POINT('Origin',(13.0227870731057,-2.97236616780865,-3.45272288248773));
#42174=CARTESIAN_POINT('Origin',(14.7626584240763,-3.36948044994605,-3.45272288248773));
#42175=CARTESIAN_POINT('Origin',(-1.94015631396094E-16,2.43287906657286E-16,
1.08333333333333));
#42176=CARTESIAN_POINT('Origin',(-1.94015631396094E-16,2.43287906657286E-16,
1.08333333333333));
#42177=CARTESIAN_POINT('Origin',(-1.94015631396094E-16,2.43287906657286E-16,
1.08333333333333));
#42178=CARTESIAN_POINT('Origin',(1.94015631396094E-16,-2.43287906657286E-16,
-1.08333333333333));
#42179=CARTESIAN_POINT('Origin',(1.94015631396094E-16,-2.43287906657286E-16,
-1.08333333333333));
#42180=CARTESIAN_POINT('Origin',(1.94015631396094E-16,-2.43287906657286E-16,
-1.08333333333333));
#42181=CARTESIAN_POINT('Origin',(1.94015631396094E-16,-2.43287906657286E-16,
-1.08333333333333));
#42182=CARTESIAN_POINT('Origin',(1.94015631396094E-16,-2.43287906657286E-16,
-1.08333333333333));
#42183=CARTESIAN_POINT('Origin',(8.63450790007668E-17,-3.78302508895262E-16,
-1.08333333333333));
#42184=CARTESIAN_POINT('Origin',(-8.63450790007668E-17,3.78302508895262E-16,
1.08333333333333));
#42185=CARTESIAN_POINT('Origin',(8.63450790007668E-17,-3.78302508895262E-16,
-1.08333333333333));
#42186=CARTESIAN_POINT('Origin',(8.63450790007668E-17,-3.78302508895262E-16,
-1.08333333333333));
#42187=CARTESIAN_POINT('Origin',(8.63450790007668E-17,-3.78302508895262E-16,
-1.08333333333333));
#42188=CARTESIAN_POINT('Origin',(-8.63450790007668E-17,3.78302508895262E-16,
1.08333333333333));
#42189=CARTESIAN_POINT('Origin',(-8.63450790007668E-17,3.78302508895262E-16,
1.08333333333333));
#42190=CARTESIAN_POINT('Origin',(8.63450790007668E-17,-3.78302508895262E-16,
-1.08333333333333));
#42191=CARTESIAN_POINT('Origin',(5.79568548444348,-12.0348649162504,-3.45272288248773));
#42192=CARTESIAN_POINT('Origin',(6.57000108040713,-13.6427478189685,-3.45272288248772));
#42193=CARTESIAN_POINT('Origin',(-8.63450790007668E-17,3.78302508895262E-16,
1.08333333333333));
#42194=CARTESIAN_POINT('Origin',(-8.63450790007668E-17,3.78302508895262E-16,
1.08333333333333));
#42195=CARTESIAN_POINT('Origin',(-8.63450790007668E-17,3.78302508895262E-16,
1.08333333333333));
#42196=CARTESIAN_POINT('Origin',(8.63450790007668E-17,-3.78302508895262E-16,
-1.08333333333333));
#42197=CARTESIAN_POINT('Origin',(8.63450790007668E-17,-3.78302508895262E-16,
-1.08333333333333));
#42198=CARTESIAN_POINT('Origin',(8.63450790007668E-17,-3.78302508895262E-16,
-1.08333333333333));
#42199=CARTESIAN_POINT('Origin',(8.63450790007668E-17,-3.78302508895262E-16,
-1.08333333333333));
#42200=CARTESIAN_POINT('Origin',(8.63450790007668E-17,-3.78302508895262E-16,
-1.08333333333333));
#42201=CARTESIAN_POINT('Origin',(-8.63450790007644E-17,-3.78302508895264E-16,
-1.08333333333333));
#42202=CARTESIAN_POINT('Origin',(8.63450790007644E-17,3.78302508895264E-16,
1.08333333333333));
#42203=CARTESIAN_POINT('Origin',(-8.63450790007644E-17,-3.78302508895264E-16,
-1.08333333333333));
#42204=CARTESIAN_POINT('Origin',(-8.63450790007644E-17,-3.78302508895264E-16,
-1.08333333333333));
#42205=CARTESIAN_POINT('Origin',(-8.63450790007644E-17,-3.78302508895264E-16,
-1.08333333333333));
#42206=CARTESIAN_POINT('Origin',(8.63450790007644E-17,3.78302508895264E-16,
1.08333333333333));
#42207=CARTESIAN_POINT('Origin',(8.63450790007644E-17,3.78302508895264E-16,
1.08333333333333));
#42208=CARTESIAN_POINT('Origin',(-8.63450790007644E-17,-3.78302508895264E-16,
-1.08333333333333));
#42209=CARTESIAN_POINT('Origin',(-5.79568548444331,-12.0348649162504,-3.45272288248773));
#42210=CARTESIAN_POINT('Origin',(-6.57000108040694,-13.6427478189686,-3.45272288248772));
#42211=CARTESIAN_POINT('Origin',(8.63450790007644E-17,3.78302508895264E-16,
1.08333333333333));
#42212=CARTESIAN_POINT('Origin',(8.63450790007644E-17,3.78302508895264E-16,
1.08333333333333));
#42213=CARTESIAN_POINT('Origin',(8.63450790007644E-17,3.78302508895264E-16,
1.08333333333333));
#42214=CARTESIAN_POINT('Origin',(-8.63450790007644E-17,-3.78302508895264E-16,
-1.08333333333333));
#42215=CARTESIAN_POINT('Origin',(-8.63450790007644E-17,-3.78302508895264E-16,
-1.08333333333333));
#42216=CARTESIAN_POINT('Origin',(-8.63450790007644E-17,-3.78302508895264E-16,
-1.08333333333333));
#42217=CARTESIAN_POINT('Origin',(-8.63450790007644E-17,-3.78302508895264E-16,
-1.08333333333333));
#42218=CARTESIAN_POINT('Origin',(-8.63450790007644E-17,-3.78302508895264E-16,
-1.08333333333333));
#42219=CARTESIAN_POINT('Origin',(-1.94015631396093E-16,-2.43287906657289E-16,
-1.08333333333333));
#42220=CARTESIAN_POINT('Origin',(1.94015631396093E-16,2.43287906657289E-16,
1.08333333333333));
#42221=CARTESIAN_POINT('Origin',(-1.94015631396093E-16,-2.43287906657289E-16,
-1.08333333333333));
#42222=CARTESIAN_POINT('Origin',(-1.94015631396093E-16,-2.43287906657289E-16,
-1.08333333333333));
#42223=CARTESIAN_POINT('Origin',(-1.94015631396093E-16,-2.43287906657289E-16,
-1.08333333333333));
#42224=CARTESIAN_POINT('Origin',(1.94015631396093E-16,2.43287906657289E-16,
1.08333333333333));
#42225=CARTESIAN_POINT('Origin',(1.94015631396093E-16,2.43287906657289E-16,
1.08333333333333));
#42226=CARTESIAN_POINT('Origin',(-1.94015631396093E-16,-2.43287906657289E-16,
-1.08333333333333));
#42227=CARTESIAN_POINT('Origin',(-13.0227870731057,-2.97236616780882,-3.45272288248773));
#42228=CARTESIAN_POINT('Origin',(-14.7626584240763,-3.36948044994625,-3.45272288248773));
#42229=CARTESIAN_POINT('Origin',(1.94015631396093E-16,2.43287906657289E-16,
1.08333333333333));
#42230=CARTESIAN_POINT('Origin',(1.94015631396093E-16,2.43287906657289E-16,
1.08333333333333));
#42231=CARTESIAN_POINT('Origin',(1.94015631396093E-16,2.43287906657289E-16,
1.08333333333333));
#42232=CARTESIAN_POINT('Origin',(-1.94015631396093E-16,-2.43287906657289E-16,
-1.08333333333333));
#42233=CARTESIAN_POINT('Origin',(-1.94015631396093E-16,-2.43287906657289E-16,
-1.08333333333333));
#42234=CARTESIAN_POINT('Origin',(-1.94015631396093E-16,-2.43287906657289E-16,
-1.08333333333333));
#42235=CARTESIAN_POINT('Origin',(-1.94015631396093E-16,-2.43287906657289E-16,
-1.08333333333333));
#42236=CARTESIAN_POINT('Origin',(-1.94015631396093E-16,-2.43287906657289E-16,
-1.08333333333333));
#42237=CARTESIAN_POINT('Origin',(-1.55588456152529E-16,-7.49274514625064E-17,
-1.08333333333333));
#42238=CARTESIAN_POINT('Origin',(1.55588456152529E-16,7.49274514625064E-17,
1.08333333333333));
#42239=CARTESIAN_POINT('Origin',(-1.55588456152529E-16,-7.49274514625064E-17,
-1.08333333333333));
#42240=CARTESIAN_POINT('Origin',(-1.55588456152529E-16,-7.49274514625064E-17,
-1.08333333333333));
#42241=CARTESIAN_POINT('Origin',(-1.55588456152529E-16,-7.49274514625064E-17,
-1.08333333333333));
#42242=CARTESIAN_POINT('Origin',(1.55588456152529E-16,7.49274514625064E-17,
1.08333333333333));
#42243=CARTESIAN_POINT('Origin',(1.55588456152529E-16,7.49274514625064E-17,
1.08333333333333));
#42244=CARTESIAN_POINT('Origin',(-1.55588456152529E-16,-7.49274514625064E-17,
-1.08333333333333));
#42245=CARTESIAN_POINT('Origin',(-10.4434643792749,8.32838493021299,-3.45272288248773));
#42246=CARTESIAN_POINT('Origin',(-11.838732871064,9.44107442276088,-3.45272288248773));
#42247=CARTESIAN_POINT('Origin',(1.55588456152529E-16,7.49274514625064E-17,
1.08333333333333));
#42248=CARTESIAN_POINT('Origin',(1.55588456152529E-16,7.49274514625064E-17,
1.08333333333333));
#42249=CARTESIAN_POINT('Origin',(1.55588456152529E-16,7.49274514625064E-17,
1.08333333333333));
#42250=CARTESIAN_POINT('Origin',(-1.55588456152529E-16,-7.49274514625064E-17,
-1.08333333333333));
#42251=CARTESIAN_POINT('Origin',(-1.55588456152529E-16,-7.49274514625064E-17,
-1.08333333333333));
#42252=CARTESIAN_POINT('Origin',(-1.55588456152529E-16,-7.49274514625064E-17,
-1.08333333333333));
#42253=CARTESIAN_POINT('Origin',(-1.55588456152529E-16,-7.49274514625064E-17,
-1.08333333333333));
#42254=CARTESIAN_POINT('Origin',(-1.55588456152529E-16,-7.49274514625064E-17,
-1.08333333333333));
#42255=CARTESIAN_POINT('Origin',(0.,0.,-1.08333333333333));
#42256=CARTESIAN_POINT('Origin',(0.,0.,-1.08333333333333));
#42257=CARTESIAN_POINT('Origin',(0.,0.,-1.08333333333333));
#42258=CARTESIAN_POINT('Origin',(0.,0.,1.08333333333333));
#42259=CARTESIAN_POINT('Origin',(0.,0.,1.08333333333333));
#42260=CARTESIAN_POINT('Origin',(0.,0.,1.08333333333333));
#42261=CARTESIAN_POINT('Origin',(0.,0.,-1.08333333333333));
#42262=CARTESIAN_POINT('Origin',(0.,0.,-1.08333333333333));
#42263=CARTESIAN_POINT('',(0.,0.,0.));
#42264=CARTESIAN_POINT('Origin',(0.,1.73472347597681E-15,6.67403582113016E-15));
#42265=CARTESIAN_POINT('',(1.52656933693714E-15,12.4653846153846,-3.0875));
#42266=CARTESIAN_POINT('Origin',(0.,6.26866080313552E-16,-3.0875));
#42267=CARTESIAN_POINT('',(-1.52656933693714E-15,12.4653846153846,3.0875));
#42268=CARTESIAN_POINT('Origin',(1.74512168878498E-15,14.25,4.05635328795269E-15));
#42269=CARTESIAN_POINT('Origin',(0.,1.76119517802379E-15,3.0875));
#42270=CARTESIAN_POINT('Origin',(0.,1.56496838953657E-16,-5.64807088834312));
#42271=CARTESIAN_POINT('',(9.67029207191279E-16,7.64278544417155,-5.99278544417156));
#42272=CARTESIAN_POINT('',(9.35971273077467E-16,-7.64278544417155,-5.99278544417156));
#42273=CARTESIAN_POINT('Origin',(0.,9.31738023414375E-17,-5.99278544417156));
#42274=CARTESIAN_POINT('',(9.18485099360515E-16,-7.5,-5.64807088834312));
#42275=CARTESIAN_POINT('Origin',(9.78186630818948E-16,-7.9875,-5.64807088834312));
#42276=CARTESIAN_POINT('',(9.18485099360515E-16,7.5,-5.64807088834312));
#42277=CARTESIAN_POINT('Origin',(0.,1.56496838953657E-16,-5.64807088834312));
#42278=CARTESIAN_POINT('Origin',(0.,1.56496838953657E-16,-5.64807088834312));
#42279=CARTESIAN_POINT('Origin',(0.,9.31738023414375E-17,-5.99278544417156));
#42280=CARTESIAN_POINT('Origin',(0.,2.23156441938368E-15,5.64807088834312));
#42281=CARTESIAN_POINT('',(9.18485099360515E-16,7.5,5.64807088834312));
#42282=CARTESIAN_POINT('',(9.18485099360515E-16,-7.5,5.64807088834312));
#42283=CARTESIAN_POINT('Origin',(0.,2.23156441938368E-15,5.64807088834312));
#42284=CARTESIAN_POINT('',(-9.35971273077467E-16,-7.64278544417155,5.99278544417156));
#42285=CARTESIAN_POINT('Origin',(9.78186630818948E-16,-7.9875,5.64807088834312));
#42286=CARTESIAN_POINT('Origin',(0.,2.2948874559959E-15,5.99278544417156));
#42287=CARTESIAN_POINT('Origin',(0.,2.23156441938368E-15,5.64807088834312));
#42288=CARTESIAN_POINT('Origin',(0.,-9.99635681210842E-31,-6.5));
#42289=CARTESIAN_POINT('',(-9.98087141305092E-16,8.14999999999999,-6.50000000000001));
#42290=CARTESIAN_POINT('',(9.98087141305092E-16,8.14999999999999,-6.5));
#42291=CARTESIAN_POINT('Origin',(0.,-9.99635681210842E-31,-6.5));
#42292=CARTESIAN_POINT('Origin',(0.,0.,-6.5));
#42293=CARTESIAN_POINT('',(-9.18485099360515E-16,7.5,-6.5));
#42294=CARTESIAN_POINT('Origin',(0.,2.26865819542047E-15,5.85));
#42295=CARTESIAN_POINT('',(-9.98087141305091E-16,-8.14999999999998,6.50000000000001));
#42296=CARTESIAN_POINT('',(9.18485099360515E-16,-7.5,5.85));
#42297=CARTESIAN_POINT('Origin',(0.,2.38806125833734E-15,6.50000000000001));
#42298=CARTESIAN_POINT('Origin',(0.,0.,-6.5));
#42299=CARTESIAN_POINT('',(-1.52656933693714E-15,12.4653846153846,6.50000000000001));
#42300=CARTESIAN_POINT('Origin',(0.,2.38806125833734E-15,6.50000000000001));
#42301=CARTESIAN_POINT('',(-1.52656933693714E-15,12.4653846153846,-6.5));
#42302=CARTESIAN_POINT('Origin',(0.,0.,-6.5));
#42303=CARTESIAN_POINT('',(-1.52656933693714E-15,12.4653846153846,-6.50000000000001));
#42304=CARTESIAN_POINT('',(-1.52656933693714E-15,12.4653846153846,-6.5));
#42305=CARTESIAN_POINT('Origin',(0.,-1.17267830746035E-30,-6.50000000000001));
#42306=CARTESIAN_POINT('Origin',(0.,8.14999999999999,-6.50000000000001));
#42307=CARTESIAN_POINT('Origin',(0.,8.14999999999999,6.50000000000001));
#42308=CARTESIAN_POINT('Origin',(0.,14.25,4.07195060716495E-15));
#42309=CARTESIAN_POINT('',(-3.56616156686793,14.25,4.07195060716495E-15));
#42310=CARTESIAN_POINT('',(3.56616156686793,14.25,4.07195060716495E-15));
#42311=CARTESIAN_POINT('Origin',(0.,14.25,4.07195060716495E-15));
#42312=CARTESIAN_POINT('Origin',(11.1410986251694,8.88472967648693,5.05753477640253E-15));
#42313=CARTESIAN_POINT('',(8.91763325644669,11.6728670610318,4.54536224786764E-15));
#42314=CARTESIAN_POINT('',(13.3645639938921,6.09659229194206,5.56970730493742E-15));
#42315=CARTESIAN_POINT('Origin',(11.1410986251694,8.88472967648693,5.05753477640253E-15));
#42316=CARTESIAN_POINT('Origin',(13.892722748591,-3.17092330887753,7.27212230242621E-15));
#42317=CARTESIAN_POINT('',(14.6862683510896,0.305827142012077,6.6334536057588E-15));
#42318=CARTESIAN_POINT('',(13.0991771460924,-6.64767375976714,7.91079099909362E-15));
#42319=CARTESIAN_POINT('Origin',(13.892722748591,-3.17092330887753,7.27212230242621E-15));
#42320=CARTESIAN_POINT('Origin',(6.18284328242512,-12.8388063676095,9.04808360878726E-15));
#42321=CARTESIAN_POINT('',(9.39584383208325,-11.2915068526795,8.76384929904507E-15));
#42322=CARTESIAN_POINT('',(2.96984273276699,-14.3861058825395,9.33231791852945E-15));
#42323=CARTESIAN_POINT('Origin',(6.18284328242512,-12.8388063676095,9.04808360878726E-15));
#42324=CARTESIAN_POINT('Origin',(-6.1828432824253,-12.8388063676094,9.04808360878725E-15));
#42325=CARTESIAN_POINT('',(-2.9698427327672,-14.3861058825394,9.33231791852944E-15));
#42326=CARTESIAN_POINT('',(-9.39584383208341,-11.2915068526794,8.76384929904506E-15));
#42327=CARTESIAN_POINT('Origin',(-6.1828432824253,-12.8388063676094,9.04808360878725E-15));
#42328=CARTESIAN_POINT('Origin',(-13.892722748591,-3.17092330887735,7.27212230242617E-15));
#42329=CARTESIAN_POINT('',(-13.0991771460925,-6.64767375976697,7.91079099909359E-15));
#42330=CARTESIAN_POINT('',(-14.6862683510895,0.30582714201227,6.63345360575876E-15));
#42331=CARTESIAN_POINT('Origin',(-13.892722748591,-3.17092330887735,7.27212230242617E-15));
#42332=CARTESIAN_POINT('Origin',(-11.1410986251693,8.88472967648709,5.0575347764025E-15));
#42333=CARTESIAN_POINT('',(-13.3645639938921,6.09659229194225,5.56970730493739E-15));
#42334=CARTESIAN_POINT('',(-8.91763325644655,11.6728670610319,4.54536224786761E-15));
#42335=CARTESIAN_POINT('Origin',(-11.1410986251693,8.88472967648709,5.0575347764025E-15));
#42336=CARTESIAN_POINT('Origin',(0.,1.07462756625201E-17,-6.44149999999999));
#42337=CARTESIAN_POINT('',(-1.99949495950787E-15,-16.3271153846154,-6.49999999999999));
#42338=CARTESIAN_POINT('Origin',(0.,2.01169401222323E-30,-6.49999999999999));
#42339=CARTESIAN_POINT('',(1.99233077573286E-15,-16.2686153846154,-6.44149999999999));
#42340=CARTESIAN_POINT('Origin',(1.99949495950788E-15,-16.3271153846154,
-6.44149999999999));
#42341=CARTESIAN_POINT('',(1.99233077573286E-15,16.2686153846154,-6.44149999999999));
#42342=CARTESIAN_POINT('Origin',(0.,1.07462756625199E-17,-6.44149999999999));
#42343=CARTESIAN_POINT('Origin',(0.,1.07462756625199E-17,-6.44149999999999));
#42344=CARTESIAN_POINT('Origin',(0.,1.30149338579385E-16,-5.7915));
#42345=CARTESIAN_POINT('',(-1.96367404063281E-15,16.0346153846154,-5.7915));
#42346=CARTESIAN_POINT('Origin',(0.,1.30149338579385E-16,-5.7915));
#42347=CARTESIAN_POINT('',(-1.97083822440782E-15,16.0931153846154,-5.85));
#42348=CARTESIAN_POINT('Origin',(1.97083822440783E-15,16.0931153846154,
-5.7915));
#42349=CARTESIAN_POINT('Origin',(0.,1.19403062916867E-16,-5.85));
#42350=CARTESIAN_POINT('Origin',(0.,2.37731498267482E-15,6.44150000000001));
#42351=CARTESIAN_POINT('',(-1.99949495950787E-15,16.3271153846154,6.5));
#42352=CARTESIAN_POINT('Origin',(0.,2.38806125833734E-15,6.50000000000001));
#42353=CARTESIAN_POINT('',(-1.99233077573286E-15,16.2686153846154,6.4415));
#42354=CARTESIAN_POINT('Origin',(1.99949495950788E-15,16.3271153846154,
6.44150000000001));
#42355=CARTESIAN_POINT('Origin',(0.,2.37731498267482E-15,6.44150000000001));
#42356=CARTESIAN_POINT('Origin',(0.,2.25791191975795E-15,5.7915));
#42357=CARTESIAN_POINT('',(1.96367404063281E-15,16.0346153846154,5.7915));
#42358=CARTESIAN_POINT('',(1.96367404063282E-15,-16.0346153846154,5.7915));
#42359=CARTESIAN_POINT('Origin',(0.,2.25791191975795E-15,5.7915));
#42360=CARTESIAN_POINT('',(-1.97083822440782E-15,-16.0931153846154,5.85000000000001));
#42361=CARTESIAN_POINT('Origin',(1.97083822440783E-15,-16.0931153846154,
5.7915));
#42362=CARTESIAN_POINT('Origin',(0.,2.26865819542047E-15,5.85));
#42363=CARTESIAN_POINT('Origin',(0.,2.25791191975795E-15,5.7915));
#42364=CARTESIAN_POINT('Origin',(0.,0.,-6.5));
#42365=CARTESIAN_POINT('',(-2.16636878649169E-15,17.6897435897436,-6.084));
#42366=CARTESIAN_POINT('Origin',(0.,7.6417960266795E-17,-6.084));
#42367=CARTESIAN_POINT('',(-2.16636878649169E-15,17.6897435897436,-5.85));
#42368=CARTESIAN_POINT('',(-2.16636878649169E-15,17.6897435897436,-6.5));
#42369=CARTESIAN_POINT('Origin',(0.,1.19403062916867E-16,-5.85));
#42370=CARTESIAN_POINT('Origin',(0.,0.,-6.5));
#42371=CARTESIAN_POINT('',(-1.99233077573286E-15,16.2686153846154,-6.084));
#42372=CARTESIAN_POINT('',(-1.99233077573286E-15,16.2686153846154,-6.5));
#42373=CARTESIAN_POINT('Origin',(0.,7.6417960266795E-17,-6.084));
#42374=CARTESIAN_POINT('Origin',(0.,0.,-6.5));
#42375=CARTESIAN_POINT('',(-1.96367404063281E-15,16.0346153846154,3.0875));
#42376=CARTESIAN_POINT('Origin',(0.,1.76119517802379E-15,3.08750000000001));
#42377=CARTESIAN_POINT('',(-1.96367404063282E-15,16.0346153846154,-6.5));
#42378=CARTESIAN_POINT('Origin',(0.,1.73472347597681E-15,6.67403582113016E-15));
#42379=CARTESIAN_POINT('',(-1.96367404063281E-15,16.0346153846154,-3.0875));
#42380=CARTESIAN_POINT('Origin',(1.74512168878498E-15,14.25,4.05635328795269E-15));
#42381=CARTESIAN_POINT('Origin',(0.,6.26866080313552E-16,-3.08749999999999));
#42382=CARTESIAN_POINT('Origin',(0.,0.,-6.5));
#42383=CARTESIAN_POINT('',(-1.96367404063282E-15,16.0346153846154,-6.5));
#42384=CARTESIAN_POINT('Origin',(0.,0.,-6.5));
#42385=CARTESIAN_POINT('',(-1.99233077573286E-15,16.2686153846154,6.084));
#42386=CARTESIAN_POINT('Origin',(0.,2.31164329807054E-15,6.084));
#42387=CARTESIAN_POINT('',(-1.99233077573286E-15,16.2686153846154,-6.5));
#42388=CARTESIAN_POINT('Origin',(0.,0.,-6.5));
#42389=CARTESIAN_POINT('',(-2.16636878649169E-15,17.6897435897436,5.85));
#42390=CARTESIAN_POINT('Origin',(0.,2.26865819542047E-15,5.85));
#42391=CARTESIAN_POINT('',(-2.16636878649169E-15,17.6897435897436,6.084));
#42392=CARTESIAN_POINT('',(-2.16636878649169E-15,17.6897435897436,-6.5));
#42393=CARTESIAN_POINT('Origin',(0.,2.31164329807054E-15,6.084));
#42394=CARTESIAN_POINT('Origin',(0.,2.38806125833734E-15,6.50000000000001));
#42395=CARTESIAN_POINT('',(-2.57175827820944E-15,21.,5.85));
#42396=CARTESIAN_POINT('Origin',(0.,2.26865819542047E-15,5.85000000000001));
#42397=CARTESIAN_POINT('',(-2.49215623626487E-15,20.35,6.5));
#42398=CARTESIAN_POINT('',(2.49215623626486E-15,20.35,6.50000000000001));
#42399=CARTESIAN_POINT('Origin',(0.,2.38806125833734E-15,6.50000000000001));
#42400=CARTESIAN_POINT('Origin',(0.,1.19403062916869E-16,-5.84999999999999));
#42401=CARTESIAN_POINT('',(2.57175827820944E-15,21.,-5.84999999999999));
#42402=CARTESIAN_POINT('',(2.57175827820944E-15,-21.,-5.84999999999999));
#42403=CARTESIAN_POINT('Origin',(0.,1.19403062916869E-16,-5.84999999999999));
#42404=CARTESIAN_POINT('Origin',(0.,1.19403062916869E-16,-5.84999999999999));
#42405=CARTESIAN_POINT('',(-2.49215623626487E-15,-20.35,-6.49999999999999));
#42406=CARTESIAN_POINT('',(2.57175827820944E-15,-21.,-5.84999999999999));
#42407=CARTESIAN_POINT('Origin',(0.,1.96135664184276E-30,-6.49999999999999));
#42408=CARTESIAN_POINT('Origin',(0.,0.,-6.5));
#42409=CARTESIAN_POINT('',(-2.57175827820944E-15,21.,-6.5));
#42410=CARTESIAN_POINT('Origin',(0.,20.35,-6.49999999999999));
#42411=CARTESIAN_POINT('Origin',(0.,20.35,6.5));
#42412=CARTESIAN_POINT('Origin',(0.,16.0346153846154,5.85));
#42413=CARTESIAN_POINT('Origin',(0.,16.2686153846154,6.084));
#42414=CARTESIAN_POINT('Origin',(0.,16.2686153846154,-6.084));
#42415=CARTESIAN_POINT('Origin',(0.,16.0346153846154,-5.85));
#42416=CARTESIAN_POINT('Origin',(-11.1410986251694,8.88472967648693,9.85584169237584E-16));
#42417=CARTESIAN_POINT('',(-11.838732871064,9.44107442276088,3.96060240207311));
#42418=CARTESIAN_POINT('Origin',(-11.838732871064,9.44107442276088,1.04729956121144E-15));
#42419=CARTESIAN_POINT('',(-10.4434643792749,8.32838493021299,3.96060240207311));
#42420=CARTESIAN_POINT('Origin',(-11.1410986251694,8.88472967648693,2.5198520116158));
#42421=CARTESIAN_POINT('Origin',(-10.4434643792749,8.32838493021299,9.23868777263733E-16));
#42422=CARTESIAN_POINT('',(-13.176267261227,5.42664547033602,-1.08333333333333));
#42423=CARTESIAN_POINT('',(-13.9269936544441,5.94376395877182,-1.08333333333333));
#42424=CARTESIAN_POINT('Ctrl Pts',(-13.176267261227,5.42664547033603,-1.08333333333333));
#42425=CARTESIAN_POINT('Ctrl Pts',(-13.3544742809805,5.48608062863209,-1.08333333333333));
#42426=CARTESIAN_POINT('Ctrl Pts',(-13.5395781511317,5.58798093945111,-1.08333333333333));
#42427=CARTESIAN_POINT('Ctrl Pts',(-13.7657237213497,5.76832601371359,-1.08333333333333));
#42428=CARTESIAN_POINT('Ctrl Pts',(-13.851789663848,5.85187873682469,-1.08333333333333));
#42429=CARTESIAN_POINT('Ctrl Pts',(-13.9269936544446,5.9437639587714,-1.08333333333333));
#42430=CARTESIAN_POINT('',(-13.9269936544455,5.94376395877242,1.08333333333333));
#42431=CARTESIAN_POINT('Ctrl Pts',(-13.9269936544444,5.94376395877114,1.08333333333355));
#42432=CARTESIAN_POINT('Ctrl Pts',(-13.9416885168396,5.90933203032471,0.95688863210348));
#42433=CARTESIAN_POINT('Ctrl Pts',(-13.9536527109306,5.88095561854246,0.828820583351296));
#42434=CARTESIAN_POINT('Ctrl Pts',(-13.9629765258054,5.85873440158612,0.699646919261824));
#42435=CARTESIAN_POINT('Ctrl Pts',(-13.9722513158078,5.83663002439321,0.571152453813156));
#42436=CARTESIAN_POINT('Ctrl Pts',(-13.9789135007646,5.82061622745832,0.441563969171476));
#42437=CARTESIAN_POINT('Ctrl Pts',(-13.9830050237945,5.81077040959789,0.311391073637591));
#42438=CARTESIAN_POINT('Ctrl Pts',(-13.9870637119681,5.80100360534983,0.182262827807202));
#42439=CARTESIAN_POINT('Ctrl Pts',(-13.9885928700523,5.79730615639837,0.0525595133518154));
#42440=CARTESIAN_POINT('Ctrl Pts',(-13.9875862925321,5.79973378332902,-0.0772214321948836));
#42441=CARTESIAN_POINT('Ctrl Pts',(-13.9868997670034,5.80138952054624,-0.16573715053464));
#42442=CARTESIAN_POINT('Ctrl Pts',(-13.9850326975558,5.80589410253377,-0.25428898113034));
#42443=CARTESIAN_POINT('Ctrl Pts',(-13.9819702480149,5.81325986277477,-0.342719102199523));
#42444=CARTESIAN_POINT('Ctrl Pts',(-13.9773533484511,5.82436436418404,-0.476034927301742));
#42445=CARTESIAN_POINT('Ctrl Pts',(-13.9700489046451,5.84190742581559,-0.608312350205735));
#42446=CARTESIAN_POINT('Ctrl Pts',(-13.9600480872369,5.86570879353503,-0.739057191237609));
#42447=CARTESIAN_POINT('Ctrl Pts',(-13.9511688384278,5.8868408927778,-0.855139299994326));
#42448=CARTESIAN_POINT('Ctrl Pts',(-13.9401632237806,5.9129059856334,-0.970013302477931));
#42449=CARTESIAN_POINT('Ctrl Pts',(-13.9269936544444,5.94376395877114,-1.08333333333355));
#42450=CARTESIAN_POINT('',(-13.176267261227,5.42664547033602,1.08333333333333));
#42451=CARTESIAN_POINT('Ctrl Pts',(-13.176267261227,5.42664547033603,1.08333333333333));
#42452=CARTESIAN_POINT('Ctrl Pts',(-13.3544742809805,5.48608062863209,1.08333333333333));
#42453=CARTESIAN_POINT('Ctrl Pts',(-13.5395781511317,5.58798093945111,1.08333333333333));
#42454=CARTESIAN_POINT('Ctrl Pts',(-13.76572372135,5.76832601371385,1.08333333333333));
#42455=CARTESIAN_POINT('Ctrl Pts',(-13.8517896638487,5.85187873682532,1.08333333333333));
#42456=CARTESIAN_POINT('Ctrl Pts',(-13.9269936544455,5.94376395877245,1.08333333333333));
#42457=CARTESIAN_POINT('Ctrl Pts',(-13.176267261227,5.426645470336,-1.08333333333333));
#42458=CARTESIAN_POINT('Ctrl Pts',(-13.1893705593041,5.39482976422217,-0.949270311030458));
#42459=CARTESIAN_POINT('Ctrl Pts',(-13.1999097963793,5.36892368585873,-0.813521288367943));
#42460=CARTESIAN_POINT('Ctrl Pts',(-13.2079621630869,5.34904061477063,-0.676607052100963));
#42461=CARTESIAN_POINT('Ctrl Pts',(-13.2148460430323,5.33204279546006,-0.559560573777783));
#42462=CARTESIAN_POINT('Ctrl Pts',(-13.2199117356377,5.31944645364942,-0.441662516279014));
#42463=CARTESIAN_POINT('Ctrl Pts',(-13.2231796369648,5.31131059989529,-0.323238258334693));
#42464=CARTESIAN_POINT('Ctrl Pts',(-13.2269557156994,5.30190957419894,-0.186398348762648));
#42465=CARTESIAN_POINT('Ctrl Pts',(-13.2283213471704,5.29849241313602,-0.0492519096262365));
#42466=CARTESIAN_POINT('Ctrl Pts',(-13.2273014856384,5.30103720115478,0.0876758270660023));
#42467=CARTESIAN_POINT('Ctrl Pts',(-13.2262786675027,5.30358936657696,0.225000520654269));
#42468=CARTESIAN_POINT('Ctrl Pts',(-13.2228564747501,5.31213809759637,0.362105241912721));
#42469=CARTESIAN_POINT('Ctrl Pts',(-13.21701132539,5.32664168351063,0.498460177595569));
#42470=CARTESIAN_POINT('Ctrl Pts',(-13.2111409592134,5.34120783998416,0.635403368116636));
#42471=CARTESIAN_POINT('Ctrl Pts',(-13.2028266475275,5.36178038996277,0.771590289741212));
#42472=CARTESIAN_POINT('Ctrl Pts',(-13.1919958930595,5.38829698119001,0.90648424252654));
#42473=CARTESIAN_POINT('Ctrl Pts',(-13.1872415508606,5.39993688577963,0.965698216399817));
#42474=CARTESIAN_POINT('Ctrl Pts',(-13.1820016856382,5.4127218947045,1.02466304565395));
#42475=CARTESIAN_POINT('Ctrl Pts',(-13.176267261227,5.426645470336,1.08333333333333));
#42476=CARTESIAN_POINT('',(-8.89378902201695,12.2552029391753,-1.08333333333333));
#42477=CARTESIAN_POINT('',(-8.22258343557141,11.6383685130291,-1.08333333333333));
#42478=CARTESIAN_POINT('Ctrl Pts',(-8.89378902201693,12.2552029391753,-1.08333333333333));
#42479=CARTESIAN_POINT('Ctrl Pts',(-8.78747309219938,12.2023308550396,-1.08333333333333));
#42480=CARTESIAN_POINT('Ctrl Pts',(-8.68686373639314,12.1370149953911,-1.08333333333333));
#42481=CARTESIAN_POINT('Ctrl Pts',(-8.46071816617524,11.9566699211287,-1.08333333333333));
#42482=CARTESIAN_POINT('Ctrl Pts',(-8.32018322283281,11.7988819437994,-1.08333333333333));
#42483=CARTESIAN_POINT('Ctrl Pts',(-8.22258343557192,11.6383685130288,-1.08333333333333));
#42484=CARTESIAN_POINT('',(-8.22258343557665,11.6383685130365,1.08333333333333));
#42485=CARTESIAN_POINT('Ctrl Pts',(-8.22258343557191,11.6383685130287,1.08333333333318));
#42486=CARTESIAN_POINT('Ctrl Pts',(-8.19455490688727,11.6581708517696,0.949622058007629));
#42487=CARTESIAN_POINT('Ctrl Pts',(-8.17172113698899,11.6741565633286,0.814376693553349));
#42488=CARTESIAN_POINT('Ctrl Pts',(-8.15417398891324,11.6864000683928,0.678132403728345));
#42489=CARTESIAN_POINT('Ctrl Pts',(-8.13671023659264,11.698585384152,0.542535637671064));
#42490=CARTESIAN_POINT('Ctrl Pts',(-8.12448291951145,11.7070640382822,0.405949418799179));
#42491=CARTESIAN_POINT('Ctrl Pts',(-8.11755242812626,11.7118675955896,0.268901316712111));
#42492=CARTESIAN_POINT('Ctrl Pts',(-8.11302715126356,11.7150040870061,0.179415511018989));
#42493=CARTESIAN_POINT('Ctrl Pts',(-8.11075954642953,11.7165728598427,0.0897327832367744));
#42494=CARTESIAN_POINT('Ctrl Pts',(-8.11075954642953,11.7165728598427,9.99200722162641E-15));
#42495=CARTESIAN_POINT('Ctrl Pts',(-8.11075954642954,11.7165728598427,-0.137573936980354));
#42496=CARTESIAN_POINT('Ctrl Pts',(-8.11609005089583,11.7128881555246,-0.274951212619692));
#42497=CARTESIAN_POINT('Ctrl Pts',(-8.12669452775723,11.7055258768037,-0.4116124062147));
#42498=CARTESIAN_POINT('Ctrl Pts',(-8.13738105388554,11.6981066344457,-0.549330978772881));
#42499=CARTESIAN_POINT('Ctrl Pts',(-8.15342350530942,11.6869526399855,-0.686322345437031));
#42500=CARTESIAN_POINT('Ctrl Pts',(-8.17473347641523,11.6720277839618,-0.822054935347404));
#42501=CARTESIAN_POINT('Ctrl Pts',(-8.18849695174643,11.662388264195,-0.909720570537357));
#42502=CARTESIAN_POINT('Ctrl Pts',(-8.20445714658991,11.6511748546878,-0.996861109122827));
#42503=CARTESIAN_POINT('Ctrl Pts',(-8.22258343557191,11.6383685130287,-1.08333333333318));
#42504=CARTESIAN_POINT('',(-8.89378902201695,12.2552029391753,1.08333333333333));
#42505=CARTESIAN_POINT('Ctrl Pts',(-8.89378902201693,12.2552029391753,1.08333333333333));
#42506=CARTESIAN_POINT('Ctrl Pts',(-8.78747309219938,12.2023308550396,1.08333333333333));
#42507=CARTESIAN_POINT('Ctrl Pts',(-8.68686373639314,12.1370149953911,1.08333333333333));
#42508=CARTESIAN_POINT('Ctrl Pts',(-8.46071816617751,11.9566699211305,1.08333333333333));
#42509=CARTESIAN_POINT('Ctrl Pts',(-8.32018322283717,11.7988819438045,1.08333333333333));
#42510=CARTESIAN_POINT('Ctrl Pts',(-8.22258343557662,11.6383685130365,1.08333333333333));
#42511=CARTESIAN_POINT('Ctrl Pts',(-8.89378902201696,12.2552029391753,-1.08333333333333));
#42512=CARTESIAN_POINT('Ctrl Pts',(-8.86325700199161,12.2773604951023,-0.955915065626613));
#42513=CARTESIAN_POINT('Ctrl Pts',(-8.83806624000395,12.2954729083691,-0.8267015714506));
#42514=CARTESIAN_POINT('Ctrl Pts',(-8.81837639229442,12.3095783864577,-0.696211209492237));
#42515=CARTESIAN_POINT('Ctrl Pts',(-8.79899689851553,12.3234615321731,-0.567777653525536));
#42516=CARTESIAN_POINT('Ctrl Pts',(-8.7849462329058,12.3334631509294,-0.438107164856251));
#42517=CARTESIAN_POINT('Ctrl Pts',(-8.77634666705863,12.3395794672318,-0.307693975181527));
#42518=CARTESIAN_POINT('Ctrl Pts',(-8.76960830208466,12.3443720314467,-0.205506064179221));
#42519=CARTESIAN_POINT('Ctrl Pts',(-8.76621624622179,12.3467783236356,-0.102862147741002));
#42520=CARTESIAN_POINT('Ctrl Pts',(-8.76621624622179,12.3467783236356,2.44249065417534E-15));
#42521=CARTESIAN_POINT('Ctrl Pts',(-8.76621624622179,12.3467783236356,0.130666807305558));
#42522=CARTESIAN_POINT('Ctrl Pts',(-8.77169236507929,12.3428956683044,0.261069786498707));
#42523=CARTESIAN_POINT('Ctrl Pts',(-8.78256611126601,12.3351536167882,0.390710450871087));
#42524=CARTESIAN_POINT('Ctrl Pts',(-8.79357042167237,12.3273186042172,0.521907748246256));
#42525=CARTESIAN_POINT('Ctrl Pts',(-8.8101027782242,12.315530900308,0.652324314224256));
#42526=CARTESIAN_POINT('Ctrl Pts',(-8.83205039902736,12.2997710546807,0.781443489202971));
#42527=CARTESIAN_POINT('Ctrl Pts',(-8.84930597782606,12.2873804060307,0.882959098491573));
#42528=CARTESIAN_POINT('Ctrl Pts',(-8.86990830867396,12.2725335396739,0.983672743459536));
#42529=CARTESIAN_POINT('Ctrl Pts',(-8.89378902201696,12.2552029391753,1.08333333333333));
#42530=CARTESIAN_POINT('Origin',(-11.1410986251694,8.88472967648693,9.85584169237584E-16));
#42531=CARTESIAN_POINT('',(-13.6377879061429,6.58029051604744,1.08333333333333));
#42532=CARTESIAN_POINT('',(-13.2594869773434,6.22835470309403,1.08333333333333));
#42533=CARTESIAN_POINT('Origin',(-11.1410986251694,8.88472967648693,1.08333333333333));
#42534=CARTESIAN_POINT('',(-13.6377879061429,6.58029051604744,-1.08333333333333));
#42535=CARTESIAN_POINT('Ctrl Pts',(-13.6377879061429,6.58029051604746,-1.08333333333332));
#42536=CARTESIAN_POINT('Ctrl Pts',(-13.6907677796516,6.47048863474076,-0.727666221822785));
#42537=CARTESIAN_POINT('Ctrl Pts',(-13.7154355939007,6.41687686636447,-0.35278297384277));
#42538=CARTESIAN_POINT('Ctrl Pts',(-13.7154355939007,6.41687686636447,0.352782973842772));
#42539=CARTESIAN_POINT('Ctrl Pts',(-13.6907677796516,6.47048863474076,0.727666221822785));
#42540=CARTESIAN_POINT('Ctrl Pts',(-13.6377879061429,6.58029051604746,1.08333333333332));
#42541=CARTESIAN_POINT('',(-12.9276994994136,5.99475484510091,-1.08333333333333));
#42542=CARTESIAN_POINT('Origin',(-11.1410986251694,8.88472967648693,-1.08333333333333));
#42543=CARTESIAN_POINT('',(-12.9276994994136,5.99475484510091,1.08333333333333));
#42544=CARTESIAN_POINT('Ctrl Pts',(-12.9276994994136,5.99475484510092,1.08333333333333));
#42545=CARTESIAN_POINT('Ctrl Pts',(-12.9759843593574,5.89062845864246,0.725928647976576));
#42546=CARTESIAN_POINT('Ctrl Pts',(-12.9982133898606,5.84028669430256,0.352039859176989));
#42547=CARTESIAN_POINT('Ctrl Pts',(-12.9982133898606,5.84028669430256,-0.352039859176986));
#42548=CARTESIAN_POINT('Ctrl Pts',(-12.9759843593574,5.89062845864246,-0.725928647976575));
#42549=CARTESIAN_POINT('Ctrl Pts',(-12.9276994994136,5.99475484510092,-1.08333333333332));
#42550=CARTESIAN_POINT('Origin',(-11.1410986251694,8.88472967648693,1.08333333333333));
#42551=CARTESIAN_POINT('',(-9.02271027299537,11.5411046498798,1.08333333333333));
#42552=CARTESIAN_POINT('Origin',(-11.1410986251694,8.88472967648693,9.85584169237584E-16));
#42553=CARTESIAN_POINT('',(-8.72113759169224,11.2696166353063,1.08333333333333));
#42554=CARTESIAN_POINT('Origin',(-11.1410986251694,8.88472967648693,1.08333333333333));
#42555=CARTESIAN_POINT('',(-8.72113759169224,11.2696166353063,-1.08333333333333));
#42556=CARTESIAN_POINT('Ctrl Pts',(-8.72113759169222,11.2696166353063,-1.08333333333334));
#42557=CARTESIAN_POINT('Ctrl Pts',(-8.63036626326988,11.3398611937656,-0.725928647976585));
#42558=CARTESIAN_POINT('Ctrl Pts',(-8.58623309669495,11.3727349924818,-0.352039859176991));
#42559=CARTESIAN_POINT('Ctrl Pts',(-8.58623309669495,11.3727349924818,4.46574186955748E-16));
#42560=CARTESIAN_POINT('Ctrl Pts',(-8.58623309669495,11.3727349924818,0.352039859176991));
#42561=CARTESIAN_POINT('Ctrl Pts',(-8.63036626326988,11.3398611937656,0.725928647976585));
#42562=CARTESIAN_POINT('Ctrl Pts',(-8.72113759169222,11.2696166353063,1.08333333333334));
#42563=CARTESIAN_POINT('',(-9.45000219633307,11.8316076987796,-1.08333333333333));
#42564=CARTESIAN_POINT('Origin',(-11.1410986251694,8.88472967648693,-1.08333333333333));
#42565=CARTESIAN_POINT('',(-9.45000219633307,11.8316076987796,1.08333333333333));
#42566=CARTESIAN_POINT('Ctrl Pts',(-9.45000219633306,11.8316076987796,1.08333333333334));
#42567=CARTESIAN_POINT('Ctrl Pts',(-9.35474240837113,11.9076924734257,0.727666221822798));
#42568=CARTESIAN_POINT('Ctrl Pts',(-9.30796390402501,11.9436715548398,0.352782973842778));
#42569=CARTESIAN_POINT('Ctrl Pts',(-9.30796390402501,11.9436715548398,5.10741104345864E-16));
#42570=CARTESIAN_POINT('Ctrl Pts',(-9.30796390402501,11.9436715548398,-0.352782973842777));
#42571=CARTESIAN_POINT('Ctrl Pts',(-9.35474240837113,11.9076924734257,-0.727666221822798));
#42572=CARTESIAN_POINT('Ctrl Pts',(-9.45000219633306,11.8316076987796,-1.08333333333334));
#42573=CARTESIAN_POINT('Origin',(-11.1410986251694,8.88472967648693,1.08333333333333));
#42574=CARTESIAN_POINT('',(-10.4434643792749,8.32838493021299,-3.45272288248773));
#42575=CARTESIAN_POINT('Origin',(-10.4434643792749,8.32838493021299,9.23868777263733E-16));
#42576=CARTESIAN_POINT('',(-11.838732871064,9.44107442276088,-3.45272288248773));
#42577=CARTESIAN_POINT('Origin',(-11.838732871064,9.44107442276088,1.04729956121144E-15));
#42578=CARTESIAN_POINT('Origin',(-13.892722748591,-3.17092330887753,3.20017169526126E-15));
#42579=CARTESIAN_POINT('',(-14.7626584240763,-3.36948044994625,3.96060240207311));
#42580=CARTESIAN_POINT('Origin',(-14.7626584240763,-3.36948044994625,3.40056031423578E-15));
#42581=CARTESIAN_POINT('',(-13.0227870731057,-2.97236616780882,3.96060240207311));
#42582=CARTESIAN_POINT('Origin',(-13.892722748591,-3.17092330887753,2.5198520116158));
#42583=CARTESIAN_POINT('Origin',(-13.0227870731057,-2.97236616780882,2.99978307628674E-15));
#42584=CARTESIAN_POINT('',(-12.4579905368413,-6.91816245718267,-1.08333333333333));
#42585=CARTESIAN_POINT('',(-13.3303603014234,-7.18268588222789,-1.08333333333333));
#42586=CARTESIAN_POINT('Ctrl Pts',(-12.4579905368413,-6.91816245718265,
-1.08333333333333));
#42587=CARTESIAN_POINT('Ctrl Pts',(-12.6155690741986,-7.02043310055334,
-1.08333333333333));
#42588=CARTESIAN_POINT('Ctrl Pts',(-12.8106483205941,-7.10161932916232,
-1.08333333333333));
#42589=CARTESIAN_POINT('Ctrl Pts',(-13.0926472341269,-7.16598374096129,
-1.08333333333333));
#42590=CARTESIAN_POINT('Ctrl Pts',(-13.211632620936,-7.18117853359748,-1.08333333333333));
#42591=CARTESIAN_POINT('Ctrl Pts',(-13.3303603014234,-7.18268588222786,
-1.08333333333333));
#42592=CARTESIAN_POINT('',(-13.3303603014234,-7.18268588222787,1.08333333333334));
#42593=CARTESIAN_POINT('Ctrl Pts',(-13.3303603014234,-7.18268588222788,
1.08333333333333));
#42594=CARTESIAN_POINT('Ctrl Pts',(-13.312602432605,-7.21564274452362,0.9568886321034));
#42595=CARTESIAN_POINT('Ctrl Pts',(-13.2978764135175,-7.24268913148589,
0.828820583351364));
#42596=CARTESIAN_POINT('Ctrl Pts',(-13.2863164700111,-7.26383348564883,
0.699646919262042));
#42597=CARTESIAN_POINT('Ctrl Pts',(-13.2748173090022,-7.28486666222222,
0.571152453813466));
#42598=CARTESIAN_POINT('Ctrl Pts',(-13.2664510227833,-7.30005980724142,
0.441563969171881));
#42599=CARTESIAN_POINT('Ctrl Pts',(-13.2613042752926,-7.30939745578436,
0.311391073638092));
#42600=CARTESIAN_POINT('Ctrl Pts',(-13.2561988309335,-7.3186601688214,0.182262827807686));
#42601=CARTESIAN_POINT('Ctrl Pts',(-13.2542614634094,-7.32216103446744,
0.0525595133522827));
#42602=CARTESIAN_POINT('Ctrl Pts',(-13.2555318677528,-7.31986045983868,
-0.0772214321944347));
#42603=CARTESIAN_POINT('Ctrl Pts',(-13.2563983335701,-7.31829137729732,
-0.165737150534351));
#42604=CARTESIAN_POINT('Ctrl Pts',(-13.2587560588234,-7.31402308269238,
-0.254288981130211));
#42605=CARTESIAN_POINT('Ctrl Pts',(-13.2626054360146,-7.30703628683457,
-0.342719102199554));
#42606=CARTESIAN_POINT('Ctrl Pts',(-13.2684086950193,-7.29650310602083,
-0.476034927301584));
#42607=CARTESIAN_POINT('Ctrl Pts',(-13.2775701666804,-7.27985434187078,
-0.608312350205395));
#42608=CARTESIAN_POINT('Ctrl Pts',(-13.2899434176249,-7.25719547792734,
-0.739057191237093));
#42609=CARTESIAN_POINT('Ctrl Pts',(-13.3009290370229,-7.23707775329796,
-0.855139299993907));
#42610=CARTESIAN_POINT('Ctrl Pts',(-13.3144456587151,-7.21222189770289,
-0.970013302477609));
#42611=CARTESIAN_POINT('Ctrl Pts',(-13.3303603014234,-7.18268588222788,
-1.08333333333332));
#42612=CARTESIAN_POINT('',(-12.4579905368413,-6.91816245718267,1.08333333333334));
#42613=CARTESIAN_POINT('Ctrl Pts',(-12.4579905368413,-6.91816245718265,
1.08333333333333));
#42614=CARTESIAN_POINT('Ctrl Pts',(-12.6150882655077,-7.02012104908378,
1.08333333333333));
#42615=CARTESIAN_POINT('Ctrl Pts',(-12.8106174809568,-7.10161229021636,
1.08333333333333));
#42616=CARTESIAN_POINT('Ctrl Pts',(-13.0925863122299,-7.16596983593587,
1.08333333333333));
#42617=CARTESIAN_POINT('Ctrl Pts',(-13.2116839714656,-7.18117918553602,
1.08333333333333));
#42618=CARTESIAN_POINT('Ctrl Pts',(-13.3303603014234,-7.18268588222786,
1.08333333333333));
#42619=CARTESIAN_POINT('Ctrl Pts',(-12.4579905368413,-6.91816245718269,
-1.08333333333333));
#42620=CARTESIAN_POINT('Ctrl Pts',(-12.4412857888864,-6.94824379644449,
-0.949270311030495));
#42621=CARTESIAN_POINT('Ctrl Pts',(-12.4276027080703,-6.97263587945683,
-0.813521288368019));
#42622=CARTESIAN_POINT('Ctrl Pts',(-12.4170780656485,-6.99132836531023,
-0.676607052101084));
#42623=CARTESIAN_POINT('Ctrl Pts',(-12.4080806643214,-7.0073083663671,-0.559560573777871));
#42624=CARTESIAN_POINT('Ctrl Pts',(-12.4013908554087,-7.01912257498617,
-0.441662516279072));
#42625=CARTESIAN_POINT('Ctrl Pts',(-12.3970674919579,-7.02675014497037,
-0.323238258334728));
#42626=CARTESIAN_POINT('Ctrl Pts',(-12.392071820683,-7.03556384585404,-0.186398348762656));
#42627=CARTESIAN_POINT('Ctrl Pts',(-12.3902516338786,-7.03876210460556,
-0.0492519096262199));
#42628=CARTESIAN_POINT('Ctrl Pts',(-12.3916053560034,-7.03637809537454,
0.0876758270660418));
#42629=CARTESIAN_POINT('Ctrl Pts',(-12.3929630026022,-7.03398717484178,
0.22500052065431));
#42630=CARTESIAN_POINT('Ctrl Pts',(-12.3975129673671,-7.02598155019929,
0.36210524191276));
#42631=CARTESIAN_POINT('Ctrl Pts',(-12.4052079364271,-7.0123687905019,0.498460177595606));
#42632=CARTESIAN_POINT('Ctrl Pts',(-12.4129361026924,-6.99869730339788,
0.635403368116707));
#42633=CARTESIAN_POINT('Ctrl Pts',(-12.4238364813948,-6.97937013765694,
0.771590289741313));
#42634=CARTESIAN_POINT('Ctrl Pts',(-12.4378151222667,-6.9543694886247,0.906484242526672));
#42635=CARTESIAN_POINT('Ctrl Pts',(-12.4439512822522,-6.94339503240897,
0.965698216399908));
#42636=CARTESIAN_POINT('Ctrl Pts',(-12.450680002204,-6.93132701813286,1.024663045654));
#42637=CARTESIAN_POINT('Ctrl Pts',(-12.4579905368413,-6.91816245718269,
1.08333333333334));
#42638=CARTESIAN_POINT('',(-15.1266902369927,0.68754979644356,-1.08333333333333));
#42639=CARTESIAN_POINT('',(-14.2259398250621,0.827729480997533,-1.08333333333333));
#42640=CARTESIAN_POINT('Ctrl Pts',(-15.1266902369927,0.687549796443589,
-1.08333333333333));
#42641=CARTESIAN_POINT('Ctrl Pts',(-15.0191128271494,0.737684039417719,
-1.08333333333333));
#42642=CARTESIAN_POINT('Ctrl Pts',(-14.905210454464,0.775655426636244,-1.08333333333333));
#42643=CARTESIAN_POINT('Ctrl Pts',(-14.6232416231909,0.840012972355744,
-1.08333333333333));
#42644=CARTESIAN_POINT('Ctrl Pts',(-14.411718162898,0.851428848194329,-1.08333333333333));
#42645=CARTESIAN_POINT('Ctrl Pts',(-14.2259398250622,0.827729480996923,
-1.08333333333333));
#42646=CARTESIAN_POINT('',(-14.2259398250711,0.827729480998061,1.08333333333334));
#42647=CARTESIAN_POINT('Ctrl Pts',(-14.2259398250621,0.827729480996948,
1.08333333333319));
#42648=CARTESIAN_POINT('Ctrl Pts',(-14.2239464151202,0.86198962338768,0.949622058007746));
#42649=CARTESIAN_POINT('Ctrl Pts',(-14.2222079250172,0.889808711690097,
0.814376693553578));
#42650=CARTESIAN_POINT('Ctrl Pts',(-14.2208398148552,0.911161325029729,
0.678132403728685));
#42651=CARTESIAN_POINT('Ctrl Pts',(-14.2194782068654,0.932412456504284,
0.542535637671376));
#42652=CARTESIAN_POINT('Ctrl Pts',(-14.2184834780892,0.947258512328182,
0.405949418799462));
#42653=CARTESIAN_POINT('Ctrl Pts',(-14.2179179597194,0.955671957675903,
0.268901316712362));
#42654=CARTESIAN_POINT('Ctrl Pts',(-14.2175487034788,0.961165532005871,
0.179415511019154));
#42655=CARTESIAN_POINT('Ctrl Pts',(-14.2173613909827,0.963916530719958,
0.0897327832368514));
#42656=CARTESIAN_POINT('Ctrl Pts',(-14.2173613909827,0.963916530719958,
-1.77635683940025E-15));
#42657=CARTESIAN_POINT('Ctrl Pts',(-14.2173613909827,0.963916530719959,
-0.137573936980362));
#42658=CARTESIAN_POINT('Ctrl Pts',(-14.2178040883167,0.957451598945575,
-0.274951212619699));
#42659=CARTESIAN_POINT('Ctrl Pts',(-14.2186598102071,0.944570379379332,
-0.411612406214706));
#42660=CARTESIAN_POINT('Ctrl Pts',(-14.2195221530139,0.931589494866292,
-0.549330978772852));
#42661=CARTESIAN_POINT('Ctrl Pts',(-14.2208039138492,0.912092599491199,
-0.686322345436968));
#42662=CARTESIAN_POINT('Ctrl Pts',(-14.222421741201,0.886126297665223,-0.82205493534731));
#42663=CARTESIAN_POINT('Ctrl Pts',(-14.2234666476786,0.869355437073727,
-0.909720570537294));
#42664=CARTESIAN_POINT('Ctrl Pts',(-14.2246506698206,0.849885807806941,
-0.996861109122796));
#42665=CARTESIAN_POINT('Ctrl Pts',(-14.2259398250621,0.827729480996951,
-1.08333333333318));
#42666=CARTESIAN_POINT('',(-15.1266902369927,0.687549796443561,1.08333333333334));
#42667=CARTESIAN_POINT('Ctrl Pts',(-15.1266902369927,0.687549796443589,
1.08333333333333));
#42668=CARTESIAN_POINT('Ctrl Pts',(-15.0191128271494,0.73768403941772,1.08333333333333));
#42669=CARTESIAN_POINT('Ctrl Pts',(-14.905210454464,0.775655426636245,1.08333333333333));
#42670=CARTESIAN_POINT('Ctrl Pts',(-14.6232416231937,0.840012972355103,
1.08333333333333));
#42671=CARTESIAN_POINT('Ctrl Pts',(-14.4117181629048,0.851428848194163,
1.08333333333333));
#42672=CARTESIAN_POINT('Ctrl Pts',(-14.2259398250711,0.827729480998062,
1.08333333333333));
#42673=CARTESIAN_POINT('Ctrl Pts',(-15.1266902369927,0.687549796443564,
-1.08333333333333));
#42674=CARTESIAN_POINT('Ctrl Pts',(-15.1249773086751,0.725235701077295,
-0.955915065626697));
#42675=CARTESIAN_POINT('Ctrl Pts',(-15.1234319803901,0.756223536825465,
-0.826701571450772));
#42676=CARTESIAN_POINT('Ctrl Pts',(-15.122183667988,0.780412301388329,-0.696211209492499));
#42677=CARTESIAN_POINT('Ctrl Pts',(-15.1209550316477,0.804219799510246,
-0.567777653525797));
#42678=CARTESIAN_POINT('Ctrl Pts',(-15.12001416535,0.821440959530219,-0.438107164856512));
#42679=CARTESIAN_POINT('Ctrl Pts',(-15.1194343523859,0.83197783168462,-0.307693975181787));
#42680=CARTESIAN_POINT('Ctrl Pts',(-15.1189800281283,0.840234212474348,
-0.205506064179395));
#42681=CARTESIAN_POINT('Ctrl Pts',(-15.1187464308798,0.844386527178334,
-0.102862147741089));
#42682=CARTESIAN_POINT('Ctrl Pts',(-15.1187464308798,0.844386527178334,
1.99840144432528E-15));
#42683=CARTESIAN_POINT('Ctrl Pts',(-15.1187464308798,0.844386527178334,
0.130666807305563));
#42684=CARTESIAN_POINT('Ctrl Pts',(-15.1191251529677,0.837684329050672,
0.261069786498716));
#42685=CARTESIAN_POINT('Ctrl Pts',(-15.1198518432089,0.824355801783686,
0.3907104508711));
#42686=CARTESIAN_POINT('Ctrl Pts',(-15.1205872590302,0.810867235029684,
0.521907748246278));
#42687=CARTESIAN_POINT('Ctrl Pts',(-15.1216790167187,0.790592205023353,
0.652324314224286));
#42688=CARTESIAN_POINT('Ctrl Pts',(-15.1230415909943,0.763606761086714,
0.78144348920301));
#42689=CARTESIAN_POINT('Ctrl Pts',(-15.1241128691977,0.742390363261972,
0.882959098491598));
#42690=CARTESIAN_POINT('Ctrl Pts',(-15.1253504648421,0.717025942629857,
0.983672743459549));
#42691=CARTESIAN_POINT('Ctrl Pts',(-15.1266902369927,0.687549796443564,
1.08333333333333));
#42692=CARTESIAN_POINT('Origin',(-13.892722748591,-3.17092330887753,3.20017169526126E-15));
#42693=CARTESIAN_POINT('',(-13.6476999686241,-6.55970790622096,1.08333333333334));
#42694=CARTESIAN_POINT('',(-13.1366786991091,-6.483368720524,1.08333333333334));
#42695=CARTESIAN_POINT('Origin',(-13.892722748591,-3.17092330887753,1.08333333333334));
#42696=CARTESIAN_POINT('',(-13.6476999686241,-6.55970790622096,-1.08333333333333));
#42697=CARTESIAN_POINT('Ctrl Pts',(-13.6476999686241,-6.55970790622096,
-1.08333333333332));
#42698=CARTESIAN_POINT('Ctrl Pts',(-13.5948858118208,-6.66958959248691,
-0.727666221822786));
#42699=CARTESIAN_POINT('Ctrl Pts',(-13.5683505740919,-6.72230205711272,
-0.35278297384277));
#42700=CARTESIAN_POINT('Ctrl Pts',(-13.5683505740919,-6.72230205711272,
0.352782973842779));
#42701=CARTESIAN_POINT('Ctrl Pts',(-13.5948858118208,-6.66958959248691,
0.727666221822796));
#42702=CARTESIAN_POINT('Ctrl Pts',(-13.6476999686241,-6.55970790622096,
1.08333333333333));
#42703=CARTESIAN_POINT('',(-12.7471768669563,-6.36961395396413,-1.08333333333333));
#42704=CARTESIAN_POINT('Origin',(-13.892722748591,-3.17092330887754,-1.08333333333333));
#42705=CARTESIAN_POINT('',(-12.7471768669563,-6.36961395396413,1.08333333333334));
#42706=CARTESIAN_POINT('Ctrl Pts',(-12.7471768669563,-6.36961395396412,
1.08333333333334));
#42707=CARTESIAN_POINT('Ctrl Pts',(-12.6958726976266,-6.472286317656,0.725928647976585));
#42708=CARTESIAN_POINT('Ctrl Pts',(-12.6703734952066,-6.52105325020167,
0.352039859176994));
#42709=CARTESIAN_POINT('Ctrl Pts',(-12.6703734952066,-6.52105325020167,
-0.352039859176985));
#42710=CARTESIAN_POINT('Ctrl Pts',(-12.6958726976266,-6.472286317656,-0.725928647976576));
#42711=CARTESIAN_POINT('Ctrl Pts',(-12.7471768669563,-6.36961395396413,
-1.08333333333333));
#42712=CARTESIAN_POINT('Origin',(-13.892722748591,-3.17092330887753,1.08333333333334));
#42713=CARTESIAN_POINT('',(-14.6487667980729,0.141522102768936,1.08333333333334));
#42714=CARTESIAN_POINT('Origin',(-13.892722748591,-3.17092330887753,3.20017169526126E-15));
#42715=CARTESIAN_POINT('',(-14.2484814298548,0.208031110850571,1.08333333333334));
#42716=CARTESIAN_POINT('Origin',(-13.892722748591,-3.17092330887753,1.08333333333334));
#42717=CARTESIAN_POINT('',(-14.2484814298548,0.20803111085057,-1.08333333333333));
#42718=CARTESIAN_POINT('Ctrl Pts',(-14.2484814298548,0.208031110850584,
-1.08333333333333));
#42719=CARTESIAN_POINT('Ctrl Pts',(-14.2468058395578,0.322795758952019,
-0.725928647976579));
#42720=CARTESIAN_POINT('Ctrl Pts',(-14.2449910310593,0.37779693624925,-0.352039859176988));
#42721=CARTESIAN_POINT('Ctrl Pts',(-14.2449910310593,0.37779693624925,2.46631154156404E-15));
#42722=CARTESIAN_POINT('Ctrl Pts',(-14.2449910310593,0.37779693624925,0.352039859176994));
#42723=CARTESIAN_POINT('Ctrl Pts',(-14.2468058395578,0.322795758952019,
0.725928647976587));
#42724=CARTESIAN_POINT('Ctrl Pts',(-14.2484814298548,0.208031110850583,
1.08333333333334));
#42725=CARTESIAN_POINT('',(-15.1423033840733,-0.0114224867028862,-1.08333333333333));
#42726=CARTESIAN_POINT('Origin',(-13.892722748591,-3.17092330887754,-1.08333333333333));
#42727=CARTESIAN_POINT('',(-15.1423033840733,-0.0114224867028857,1.08333333333334));
#42728=CARTESIAN_POINT('Ctrl Pts',(-15.1423033840733,-0.0114224867028744,
1.08333333333334));
#42729=CARTESIAN_POINT('Ctrl Pts',(-15.1423953499066,0.110492695607543,
0.727666221822802));
#42730=CARTESIAN_POINT('Ctrl Pts',(-15.1413590080604,0.169498193350012,
0.352782973842781));
#42731=CARTESIAN_POINT('Ctrl Pts',(-15.1413590080604,0.169498193350012,
2.67362166230902E-15));
#42732=CARTESIAN_POINT('Ctrl Pts',(-15.1413590080604,0.169498193350012,
-0.352782973842774));
#42733=CARTESIAN_POINT('Ctrl Pts',(-15.1423953499066,0.110492695607543,
-0.727666221822795));
#42734=CARTESIAN_POINT('Ctrl Pts',(-15.1423033840733,-0.0114224867028733,
-1.08333333333333));
#42735=CARTESIAN_POINT('Origin',(-13.892722748591,-3.17092330887753,1.08333333333334));
#42736=CARTESIAN_POINT('',(-13.0227870731057,-2.97236616780882,-3.45272288248773));
#42737=CARTESIAN_POINT('Origin',(-13.0227870731057,-2.97236616780882,2.99978307628674E-15));
#42738=CARTESIAN_POINT('',(-14.7626584240763,-3.36948044994625,-3.45272288248773));
#42739=CARTESIAN_POINT('Origin',(-14.7626584240763,-3.36948044994625,3.40056031423578E-15));
#42740=CARTESIAN_POINT('Origin',(-6.18284328242512,-12.8388063676095,4.97613300162231E-15));
#42741=CARTESIAN_POINT('',(-6.57000108040694,-13.6427478189686,3.96060240207311));
#42742=CARTESIAN_POINT('Origin',(-6.57000108040694,-13.6427478189686,5.28772891427451E-15));
#42743=CARTESIAN_POINT('',(-5.79568548444331,-12.0348649162504,3.96060240207311));
#42744=CARTESIAN_POINT('Origin',(-6.18284328242512,-12.8388063676095,2.51985201161581));
#42745=CARTESIAN_POINT('Origin',(-5.79568548444331,-12.0348649162504,4.66453708897012E-15));
#42746=CARTESIAN_POINT('',(-2.35859284151935,-14.0534529496467,-1.08333333333333));
#42747=CARTESIAN_POINT('',(-2.69569375163562,-14.9004267538186,-1.08333333333333));
#42748=CARTESIAN_POINT('Ctrl Pts',(-2.35859284151934,-14.0534529496467,
-1.08333333333333));
#42749=CARTESIAN_POINT('Ctrl Pts',(-2.37682723618162,-14.2398470420046,
-1.08333333333333));
#42750=CARTESIAN_POINT('Ctrl Pts',(-2.43502529011671,-14.4435268961719,
-1.08333333333332));
#42751=CARTESIAN_POINT('Ctrl Pts',(-2.56051322547963,-14.7041052789647,
-1.08333333333333));
#42752=CARTESIAN_POINT('Ctrl Pts',(-2.62287825309305,-14.806702452812,-1.08333333333333));
#42753=CARTESIAN_POINT('Ctrl Pts',(-2.69569375163558,-14.9004267538186,
-1.08333333333333));
#42754=CARTESIAN_POINT('',(-2.69569375163563,-14.9004267538187,1.08333333333334));
#42755=CARTESIAN_POINT('Ctrl Pts',(-2.69569375163559,-14.9004267538186,
1.08333333333335));
#42756=CARTESIAN_POINT('Ctrl Pts',(-2.65857154890325,-14.9071426748862,
0.955915065626573));
#42757=CARTESIAN_POINT('Ctrl Pts',(-2.628016775001,-14.9125315333598,0.826701571450498));
#42758=CARTESIAN_POINT('Ctrl Pts',(-2.60415669762586,-14.9166970252376,
0.696211209492072));
#42759=CARTESIAN_POINT('Ctrl Pts',(-2.58067270588166,-14.9207968600927,
0.567777653525379));
#42760=CARTESIAN_POINT('Ctrl Pts',(-2.56367395385075,-14.923711651889,0.438107164856101));
#42761=CARTESIAN_POINT('Ctrl Pts',(-2.55327224255806,-14.9254910506792,
0.307693975181385));
#42762=CARTESIAN_POINT('Ctrl Pts',(-2.54512176981446,-14.9268853348437,
0.205506064179128));
#42763=CARTESIAN_POINT('Ctrl Pts',(-2.54102158203148,-14.9275815713119,
0.102862147740959));
#42764=CARTESIAN_POINT('Ctrl Pts',(-2.54102158203148,-14.9275815713119,
4.44089209850063E-15));
#42765=CARTESIAN_POINT('Ctrl Pts',(-2.54102158203148,-14.9275815713119,
-0.130666807305524));
#42766=CARTESIAN_POINT('Ctrl Pts',(-2.54764001565181,-14.9264594186595,
-0.261069786498646));
#42767=CARTESIAN_POINT('Ctrl Pts',(-2.56079607270382,-14.9242020129234,
-0.390710450870999));
#42768=CARTESIAN_POINT('Ctrl Pts',(-2.57411009834303,-14.9219175018628,
-0.521907748246163));
#42769=CARTESIAN_POINT('Ctrl Pts',(-2.59411972995703,-14.9184702682937,
-0.652324314224157));
#42770=CARTESIAN_POINT('Ctrl Pts',(-2.62073179377387,-14.9137938537994,
-0.781443489202868));
#42771=CARTESIAN_POINT('Ctrl Pts',(-2.64165463403551,-14.9101171801624,
-0.882959098491507));
#42772=CARTESIAN_POINT('Ctrl Pts',(-2.66665850662476,-14.9056796321318,
-0.983672743459509));
#42773=CARTESIAN_POINT('Ctrl Pts',(-2.69569375163559,-14.9004267538186,
-1.08333333333334));
#42774=CARTESIAN_POINT('',(-2.35859284151935,-14.0534529496467,1.08333333333334));
#42775=CARTESIAN_POINT('Ctrl Pts',(-2.35859284151934,-14.0534529496467,
1.08333333333333));
#42776=CARTESIAN_POINT('Ctrl Pts',(-2.37688304383397,-14.2404175142851,
1.08333333333333));
#42777=CARTESIAN_POINT('Ctrl Pts',(-2.43503901504648,-14.4435553962822,
1.08333333333334));
#42778=CARTESIAN_POINT('Ctrl Pts',(-2.56054033827446,-14.7041615792632,
1.08333333333334));
#42779=CARTESIAN_POINT('Ctrl Pts',(-2.62284674626764,-14.8066618988743,
1.08333333333334));
#42780=CARTESIAN_POINT('Ctrl Pts',(-2.69569375163563,-14.9004267538187,
1.08333333333334));
#42781=CARTESIAN_POINT('Ctrl Pts',(-2.35859284151935,-14.0534529496467,
-1.08333333333333));
#42782=CARTESIAN_POINT('Ctrl Pts',(-2.32474809698527,-14.0591331175362,
-0.949622058007895));
#42783=CARTESIAN_POINT('Ctrl Pts',(-2.29723964086638,-14.0636285445206,
-0.814376693553736));
#42784=CARTESIAN_POINT('Ctrl Pts',(-2.27611794897253,-14.0670461391994,
-0.678132403728853));
#42785=CARTESIAN_POINT('Ctrl Pts',(-2.25509664145098,-14.0704474911881,
-0.542535637671543));
#42786=CARTESIAN_POINT('Ctrl Pts',(-2.24040145926613,-14.0727812605466,
-0.405949418799629));
#42787=CARTESIAN_POINT('Ctrl Pts',(-2.23207311688321,-14.0741020886196,
-0.268901316712528));
#42788=CARTESIAN_POINT('Ctrl Pts',(-2.22663511068775,-14.0749645256946,
-0.179415511019263));
#42789=CARTESIAN_POINT('Ctrl Pts',(-2.2239114043034,-14.075394064317,-0.0897327832369026));
#42790=CARTESIAN_POINT('Ctrl Pts',(-2.2239114043034,-14.075394064317,8.43769498715119E-15));
#42791=CARTESIAN_POINT('Ctrl Pts',(-2.2239114043034,-14.075394064317,0.137573936980349));
#42792=CARTESIAN_POINT('Ctrl Pts',(-2.23031275616482,-14.0743870796481,
0.274951212619667));
#42793=CARTESIAN_POINT('Ctrl Pts',(-2.24306143269717,-14.0723550057958,
0.411612406214657));
#42794=CARTESIAN_POINT('Ctrl Pts',(-2.25590874866049,-14.0703072093226,
0.549330978772813));
#42795=CARTESIAN_POINT('Ctrl Pts',(-2.27520203478074,-14.0672183663696,
0.68632234543694));
#42796=CARTESIAN_POINT('Ctrl Pts',(-2.30087730766032,-14.0630175856782,
0.822054935347292));
#42797=CARTESIAN_POINT('Ctrl Pts',(-2.31746020132759,-14.0603044266067,
0.909720570537337));
#42798=CARTESIAN_POINT('Ctrl Pts',(-2.33670515605249,-14.0571263627534,
0.996861109122898));
#42799=CARTESIAN_POINT('Ctrl Pts',(-2.35859284151935,-14.0534529496467,
1.08333333333334));
#42800=CARTESIAN_POINT('',(-9.96888517526507,-11.3978423664701,-1.08333333333333));
#42801=CARTESIAN_POINT('',(-9.516873369993,-10.6062067328295,-1.08333333333333));
#42802=CARTESIAN_POINT('Ctrl Pts',(-9.96888517526507,-11.3978423664701,
-1.08333333333333));
#42803=CARTESIAN_POINT('Ctrl Pts',(-9.94100828682427,-11.282476771434,-1.08333333333333));
#42804=CARTESIAN_POINT('Ctrl Pts',(-9.89967854500783,-11.1697495378475,
-1.08333333333333));
#42805=CARTESIAN_POINT('Ctrl Pts',(-9.77419060964491,-10.9091711550547,
-1.08333333333333));
#42806=CARTESIAN_POINT('Ctrl Pts',(-9.65123318042897,-10.7366777723525,
-1.08333333333333));
#42807=CARTESIAN_POINT('Ctrl Pts',(-9.51687336999256,-10.6062067328299,
-1.08333333333333));
#42808=CARTESIAN_POINT('',(-9.51687336999906,-10.6062067328363,1.08333333333334));
#42809=CARTESIAN_POINT('Ctrl Pts',(-9.51687336999256,-10.6062067328299,
1.08333333333319));
#42810=CARTESIAN_POINT('Ctrl Pts',(-9.54248335115827,-10.5832270800755,
0.949270311030248));
#42811=CARTESIAN_POINT('Ctrl Pts',(-9.56321910180067,-10.5644593135702,
0.813521288367661));
#42812=CARTESIAN_POINT('Ctrl Pts',(-9.57910097474595,-10.5500390764974,
0.676607052100613));
#42813=CARTESIAN_POINT('Ctrl Pts',(-9.59267821366648,-10.5377113740467,
0.559560573777554));
#42814=CARTESIAN_POINT('Ctrl Pts',(-9.6027075928823,-10.5285603838747,0.44166251627891));
#42815=CARTESIAN_POINT('Ctrl Pts',(-9.6091818848891,-10.5226481221753,0.323238258334718));
#42816=CARTESIAN_POINT('Ctrl Pts',(-9.61666296645239,-10.5158164698571,
0.186398348762648));
#42817=CARTESIAN_POINT('Ctrl Pts',(-9.61937600851194,-10.5133302394117,
0.0492519096262118));
#42818=CARTESIAN_POINT('Ctrl Pts',(-9.61735300288125,-10.5151805128572,
-0.08767582706605));
#42819=CARTESIAN_POINT('Ctrl Pts',(-9.61532413250719,-10.5170361502911,
-0.225000520654331));
#42820=CARTESIAN_POINT('Ctrl Pts',(-9.60853168799772,-10.5232534570122,
-0.362105241912796));
#42821=CARTESIAN_POINT('Ctrl Pts',(-9.59697252030892,-10.5337846211338,
-0.498460177595657));
#42822=CARTESIAN_POINT('Ctrl Pts',(-9.5853634847053,-10.5443612182148,-0.635403368116659));
#42823=CARTESIAN_POINT('Ctrl Pts',(-9.56894645381043,-10.5592890006364,
-0.771590289741169));
#42824=CARTESIAN_POINT('Ctrl Pts',(-9.54768316346852,-10.578480335569,-0.906484242526434));
#42825=CARTESIAN_POINT('Ctrl Pts',(-9.53834928383367,-10.5869046954593,
-0.965698216399696));
#42826=CARTESIAN_POINT('Ctrl Pts',(-9.52808112091929,-10.5961500981613,
-1.02466304565381));
#42827=CARTESIAN_POINT('Ctrl Pts',(-9.51687336999256,-10.6062067328299,
-1.08333333333318));
#42828=CARTESIAN_POINT('',(-9.96888517526507,-11.3978423664701,1.08333333333334));
#42829=CARTESIAN_POINT('Ctrl Pts',(-9.96888517526507,-11.3978423664701,
1.08333333333333));
#42830=CARTESIAN_POINT('Ctrl Pts',(-9.94100828682427,-11.282476771434,1.08333333333333));
#42831=CARTESIAN_POINT('Ctrl Pts',(-9.89967854500783,-11.1697495378475,
1.08333333333333));
#42832=CARTESIAN_POINT('Ctrl Pts',(-9.77419060964618,-10.9091711550573,
1.08333333333333));
#42833=CARTESIAN_POINT('Ctrl Pts',(-9.6512331804331,-10.7366777723579,1.08333333333333));
#42834=CARTESIAN_POINT('Ctrl Pts',(-9.51687336999908,-10.6062067328363,
1.08333333333333));
#42835=CARTESIAN_POINT('Ctrl Pts',(-9.96888517526508,-11.3978423664701,
-1.08333333333333));
#42836=CARTESIAN_POINT('Ctrl Pts',(-9.99706424266063,-11.3731961327199,
-0.956888632103256));
#42837=CARTESIAN_POINT('Ctrl Pts',(-10.020155672713,-11.3528209383891,-0.828820583351071));
#42838=CARTESIAN_POINT('Ctrl Pts',(-10.038197564346,-11.3368457653652,-0.699646919261599));
#42839=CARTESIAN_POINT('Ctrl Pts',(-10.0561445912219,-11.3209545902358,
-0.571152453812953));
#42840=CARTESIAN_POINT('Ctrl Pts',(-10.0690951385517,-11.3094172714603,
-0.441563969171296));
#42841=CARTESIAN_POINT('Ctrl Pts',(-10.0770534136919,-11.3023217413999,
-0.311391073637437));
#42842=CARTESIAN_POINT('Ctrl Pts',(-10.0849478229272,-11.2952831536342,
-0.182262827807044));
#42843=CARTESIAN_POINT('Ctrl Pts',(-10.0879298097314,-11.2926153440655,
-0.0525595133516554));
#42844=CARTESIAN_POINT('Ctrl Pts',(-10.0859696068728,-11.2943658227348,
0.0772214321950453));
#42845=CARTESIAN_POINT('Ctrl Pts',(-10.0846326712896,-11.2955597181575,
0.165737150534751));
#42846=CARTESIAN_POINT('Ctrl Pts',(-10.0809960349672,-11.2988081152181,
0.2542889811304));
#42847=CARTESIAN_POINT('Ctrl Pts',(-10.0750409796764,-11.304115688826,0.342719102199531));
#42848=CARTESIAN_POINT('Ctrl Pts',(-10.0660632343107,-11.3121173012435,
0.476034927301883));
#42849=CARTESIAN_POINT('Ctrl Pts',(-10.0518705086679,-11.3247537742305,
0.608312350206005));
#42850=CARTESIAN_POINT('Ctrl Pts',(-10.0325330571073,-11.3418588735079,
0.739057191238004));
#42851=CARTESIAN_POINT('Ctrl Pts',(-10.0153642561251,-11.3570456753652,
0.855139299994515));
#42852=CARTESIAN_POINT('Ctrl Pts',(-9.99413932000721,-11.3757543553326,
0.970013302477919));
#42853=CARTESIAN_POINT('Ctrl Pts',(-9.96888517526508,-11.3978423664701,
1.08333333333334));
#42854=CARTESIAN_POINT('Origin',(-6.18284328242512,-12.8388063676095,4.97613300162231E-15));
#42855=CARTESIAN_POINT('',(-3.38061559238688,-14.7601124814492,1.08333333333334));
#42856=CARTESIAN_POINT('',(-3.12168342103518,-14.3129832609672,1.08333333333334));
#42857=CARTESIAN_POINT('Origin',(-6.18284328242512,-12.8388063676095,1.08333333333334));
#42858=CARTESIAN_POINT('',(-3.38061559238688,-14.7601124814492,-1.08333333333333));
#42859=CARTESIAN_POINT('Ctrl Pts',(-3.38061559238688,-14.7601124814492,
-1.08333333333333));
#42860=CARTESIAN_POINT('Ctrl Pts',(-3.26177754255684,-14.7873308217382,
-0.727666221822789));
#42861=CARTESIAN_POINT('Ctrl Pts',(-3.20402082808,-14.799450421612,-0.35278297384277));
#42862=CARTESIAN_POINT('Ctrl Pts',(-3.20402082808,-14.799450421612,0.352782973842781));
#42863=CARTESIAN_POINT('Ctrl Pts',(-3.26177754255684,-14.7873308217382,
0.727666221822798));
#42864=CARTESIAN_POINT('Ctrl Pts',(-3.38061559238688,-14.7601124814492,
1.08333333333334));
#42865=CARTESIAN_POINT('',(-2.96777005865995,-13.9375335292483,-1.08333333333333));
#42866=CARTESIAN_POINT('Origin',(-6.18284328242512,-12.8388063676095,-1.08333333333333));
#42867=CARTESIAN_POINT('',(-2.96777005865995,-13.9375335292483,1.08333333333334));
#42868=CARTESIAN_POINT('Ctrl Pts',(-2.96777005865994,-13.9375335292483,
1.08333333333334));
#42869=CARTESIAN_POINT('Ctrl Pts',(-2.85550994597631,-13.9614374861791,
0.725928647976589));
#42870=CARTESIAN_POINT('Ctrl Pts',(-2.80148393014434,-13.9719070920595,
0.352039859176996));
#42871=CARTESIAN_POINT('Ctrl Pts',(-2.80148393014434,-13.9719070920595,
-0.352039859176986));
#42872=CARTESIAN_POINT('Ctrl Pts',(-2.85550994597631,-13.9614374861791,
-0.725928647976579));
#42873=CARTESIAN_POINT('Ctrl Pts',(-2.96777005865994,-13.9375335292483,
-1.08333333333333));
#42874=CARTESIAN_POINT('Origin',(-6.18284328242512,-12.8388063676095,1.08333333333334));
#42875=CARTESIAN_POINT('',(-9.24400314381506,-11.3646294742518,1.08333333333334));
#42876=CARTESIAN_POINT('Origin',(-6.18284328242512,-12.8388063676095,4.97613300162231E-15));
#42877=CARTESIAN_POINT('',(-9.04642813528379,-11.0102060831369,1.08333333333334));
#42878=CARTESIAN_POINT('Origin',(-6.18284328242512,-12.8388063676095,1.08333333333334));
#42879=CARTESIAN_POINT('',(-9.04642813528379,-11.0102060831369,-1.08333333333333));
#42880=CARTESIAN_POINT('Ctrl Pts',(-9.0464281352838,-11.0102060831369,-1.08333333333332));
#42881=CARTESIAN_POINT('Ctrl Pts',(-9.13511003678158,-10.9373414661859,
-0.725928647976569));
#42882=CARTESIAN_POINT('Ctrl Pts',(-9.17698017417422,-10.901629918632,-0.352039859176982));
#42883=CARTESIAN_POINT('Ctrl Pts',(-9.17698017417422,-10.901629918632,4.5383086406711E-15));
#42884=CARTESIAN_POINT('Ctrl Pts',(-9.17698017417422,-10.901629918632,0.352039859176991));
#42885=CARTESIAN_POINT('Ctrl Pts',(-9.13511003678158,-10.9373414661859,
0.725928647976579));
#42886=CARTESIAN_POINT('Ctrl Pts',(-9.0464281352838,-11.0102060831369,1.08333333333333));
#42887=CARTESIAN_POINT('',(-9.43214127690829,-11.8458513067218,-1.08333333333333));
#42888=CARTESIAN_POINT('Origin',(-6.18284328242512,-12.8388063676095,-1.08333333333333));
#42889=CARTESIAN_POINT('',(-9.43214127690829,-11.8458513067218,1.08333333333334));
#42890=CARTESIAN_POINT('Ctrl Pts',(-9.43214127690829,-11.8458513067218,
1.08333333333333));
#42891=CARTESIAN_POINT('Ctrl Pts',(-9.52751574438859,-11.7699103356433,
0.727666221822793));
#42892=CARTESIAN_POINT('Ctrl Pts',(-9.57300195158999,-11.7323107648653,
0.352782973842778));
#42893=CARTESIAN_POINT('Ctrl Pts',(-9.57300195158999,-11.7323107648653,
4.85994849902029E-15));
#42894=CARTESIAN_POINT('Ctrl Pts',(-9.57300195158999,-11.7323107648653,
-0.352782973842768));
#42895=CARTESIAN_POINT('Ctrl Pts',(-9.52751574438859,-11.7699103356433,
-0.727666221822784));
#42896=CARTESIAN_POINT('Ctrl Pts',(-9.43214127690829,-11.8458513067218,
-1.08333333333332));
#42897=CARTESIAN_POINT('Origin',(-6.18284328242512,-12.8388063676095,1.08333333333334));
#42898=CARTESIAN_POINT('',(-5.79568548444331,-12.0348649162504,-3.45272288248773));
#42899=CARTESIAN_POINT('Origin',(-5.79568548444331,-12.0348649162504,4.66453708897012E-15));
#42900=CARTESIAN_POINT('',(-6.57000108040694,-13.6427478189686,-3.45272288248772));
#42901=CARTESIAN_POINT('Origin',(-6.57000108040694,-13.6427478189686,5.28772891427451E-15));
#42902=CARTESIAN_POINT('Origin',(6.1828432824253,-12.8388063676094,4.9761330016223E-15));
#42903=CARTESIAN_POINT('',(6.57000108040713,-13.6427478189685,3.96060240207311));
#42904=CARTESIAN_POINT('Origin',(6.57000108040713,-13.6427478189685,5.28772891427449E-15));
#42905=CARTESIAN_POINT('',(5.79568548444348,-12.0348649162503,3.96060240207311));
#42906=CARTESIAN_POINT('Origin',(6.1828432824253,-12.8388063676094,2.51985201161581));
#42907=CARTESIAN_POINT('Origin',(5.79568548444348,-12.0348649162504,4.66453708897011E-15));
#42908=CARTESIAN_POINT('',(9.51687336999268,-10.6062067328298,-1.08333333333333));
#42909=CARTESIAN_POINT('',(9.96888517526453,-11.3978423664706,-1.08333333333333));
#42910=CARTESIAN_POINT('Ctrl Pts',(9.5168733699927,-10.6062067328298,-1.08333333333333));
#42911=CARTESIAN_POINT('Ctrl Pts',(9.65164439811578,-10.737077088181,-1.08333333333333));
#42912=CARTESIAN_POINT('Ctrl Pts',(9.77420433457484,-10.9091996551649,-1.08333333333333));
#42913=CARTESIAN_POINT('Ctrl Pts',(9.89970565780286,-11.169805838146,-1.08333333333333));
#42914=CARTESIAN_POINT('Ctrl Pts',(9.94099622466366,-11.2824268534395,-1.08333333333333));
#42915=CARTESIAN_POINT('Ctrl Pts',(9.96888517526534,-11.3978423664704,-1.08333333333333));
#42916=CARTESIAN_POINT('',(9.9688851752657,-11.3978423664719,1.08333333333334));
#42917=CARTESIAN_POINT('Ctrl Pts',(9.96888517526519,-11.39784236647,1.08333333333359));
#42918=CARTESIAN_POINT('Ctrl Pts',(9.99728120861575,-11.3730063679711,0.955915065626921));
#42919=CARTESIAN_POINT('Ctrl Pts',(10.0205449777511,-11.3524775820965,0.826701571450959));
#42920=CARTESIAN_POINT('Ctrl Pts',(10.038678205356,-11.3364201641361,0.696211209492648));
#42921=CARTESIAN_POINT('Ctrl Pts',(10.0565256146782,-11.3206158452779,0.567777653525928));
#42922=CARTESIAN_POINT('Ctrl Pts',(10.0694030392049,-11.309143028737,0.438107164856624));
#42923=CARTESIAN_POINT('Ctrl Pts',(10.0772795901119,-11.3021200803759,0.307693975181881));
#42924=CARTESIAN_POINT('Ctrl Pts',(10.0834514220032,-11.2966171061454,0.20550606417946));
#42925=CARTESIAN_POINT('Ctrl Pts',(10.0865521868617,-11.2938455465903,0.102862147741125));
#42926=CARTESIAN_POINT('Ctrl Pts',(10.0865521868617,-11.2938455465903,4.44089209850063E-15));
#42927=CARTESIAN_POINT('Ctrl Pts',(10.0865521868617,-11.2938455465903,-0.130666807305562));
#42928=CARTESIAN_POINT('Ctrl Pts',(10.0815483267233,-11.2983203956244,-0.261069786498721));
#42929=CARTESIAN_POINT('Ctrl Pts',(10.0715807484455,-11.3071987457576,-0.390710450871112));
#42930=CARTESIAN_POINT('Ctrl Pts',(10.0614934865685,-11.3161837008123,-0.521907748246463));
#42931=CARTESIAN_POINT('Ctrl Pts',(10.0463225295865,-11.3296785457857,-0.652324314224642));
#42932=CARTESIAN_POINT('Ctrl Pts',(10.0260740111135,-11.3475689983448,-0.781443489203535));
#42933=CARTESIAN_POINT('Ctrl Pts',(10.0101542943843,-11.3616347650465,-0.88295909849203));
#42934=CARTESIAN_POINT('Ctrl Pts',(9.99109522006272,-11.3784168138781,-0.983672743459888));
#42935=CARTESIAN_POINT('Ctrl Pts',(9.96888517526519,-11.39784236647,-1.08333333333358));
#42936=CARTESIAN_POINT('',(9.51687336999268,-10.6062067328298,1.08333333333334));
#42937=CARTESIAN_POINT('Ctrl Pts',(9.5168733699927,-10.6062067328298,1.08333333333333));
#42938=CARTESIAN_POINT('Ctrl Pts',(9.65123318042911,-10.7366777723523,1.08333333333333));
#42939=CARTESIAN_POINT('Ctrl Pts',(9.77419060964506,-10.9091711550545,1.08333333333333));
#42940=CARTESIAN_POINT('Ctrl Pts',(9.89967854500826,-11.1697495378479,1.08333333333333));
#42941=CARTESIAN_POINT('Ctrl Pts',(9.94100828682489,-11.2824767714351,1.08333333333333));
#42942=CARTESIAN_POINT('Ctrl Pts',(9.96888517526571,-11.3978423664719,1.08333333333333));
#42943=CARTESIAN_POINT('Ctrl Pts',(9.51687336999268,-10.6062067328298,-1.08333333333333));
#42944=CARTESIAN_POINT('Ctrl Pts',(9.54241615713793,-10.5832873727889,-0.949622058007762));
#42945=CARTESIAN_POINT('Ctrl Pts',(9.56308206533645,-10.5645832486408,-0.814376693553466));
#42946=CARTESIAN_POINT('Ctrl Pts',(9.5789232079445,-10.5502004803844,-0.678132403728444));
#42947=CARTESIAN_POINT('Ctrl Pts',(9.59468906287363,-10.5358860686389,-0.542535637671145));
#42948=CARTESIAN_POINT('Ctrl Pts',(9.60567597345963,-10.5258519939611,-0.405949418799242));
#42949=CARTESIAN_POINT('Ctrl Pts',(9.61190127497217,-10.5201641565229,-0.268901316712153));
#42950=CARTESIAN_POINT('Ctrl Pts',(9.61596609683434,-10.5164502727984,-0.179415511019018));
#42951=CARTESIAN_POINT('Ctrl Pts',(9.61800012680612,-10.5145886063487,-0.0897327832367887));
#42952=CARTESIAN_POINT('Ctrl Pts',(9.61800012680612,-10.5145886063487,-9.32587340685131E-15));
#42953=CARTESIAN_POINT('Ctrl Pts',(9.61800012680612,-10.5145886063487,0.137573936980381));
#42954=CARTESIAN_POINT('Ctrl Pts',(9.61322165688595,-10.5189655400926,0.274951212619743));
#42955=CARTESIAN_POINT('Ctrl Pts',(9.6036842477684,-10.5276658794419,0.411612406214774));
#42956=CARTESIAN_POINT('Ctrl Pts',(9.59407304553156,-10.5364335353099,0.54933097877281));
#42957=CARTESIAN_POINT('Ctrl Pts',(9.57962892372621,-10.5495917717182,0.686322345436814));
#42958=CARTESIAN_POINT('Ctrl Pts',(9.5603363503304,-10.5670463644555,0.822054935347047));
#42959=CARTESIAN_POINT('Ctrl Pts',(9.54787585206456,-10.5783197657831,0.909720570537174));
#42960=CARTESIAN_POINT('Ctrl Pts',(9.5333921086825,-10.5913845868635,0.996861109122817));
#42961=CARTESIAN_POINT('Ctrl Pts',(9.51687336999268,-10.6062067328298,1.08333333333334));
#42962=CARTESIAN_POINT('',(2.69569375163578,-14.9004267538186,-1.08333333333333));
#42963=CARTESIAN_POINT('',(2.35859284151893,-14.0534529496468,-1.08333333333333));
#42964=CARTESIAN_POINT('Ctrl Pts',(2.6956937516358,-14.9004267538186,-1.08333333333332));
#42965=CARTESIAN_POINT('Ctrl Pts',(2.62284674626782,-14.8066618988742,-1.08333333333332));
#42966=CARTESIAN_POINT('Ctrl Pts',(2.56054033827465,-14.7041615792632,-1.08333333333332));
#42967=CARTESIAN_POINT('Ctrl Pts',(2.4350390150467,-14.4435553962822,-1.08333333333332));
#42968=CARTESIAN_POINT('Ctrl Pts',(2.37688304383419,-14.2404175142851,-1.08333333333332));
#42969=CARTESIAN_POINT('Ctrl Pts',(2.35859284151955,-14.0534529496467,-1.08333333333332));
#42970=CARTESIAN_POINT('',(2.35859284152043,-14.0534529496557,1.08333333333334));
#42971=CARTESIAN_POINT('Ctrl Pts',(2.35859284151951,-14.0534529496467,1.08333333333319));
#42972=CARTESIAN_POINT('Ctrl Pts',(2.32465906345733,-14.0591480600448,0.949270311030372));
#42973=CARTESIAN_POINT('Ctrl Pts',(2.29705730368849,-14.0636584116899,0.813521288367913));
#42974=CARTESIAN_POINT('Ctrl Pts',(2.27588092254449,-14.0670844892038,0.676607052100994));
#42975=CARTESIAN_POINT('Ctrl Pts',(2.25777746665768,-14.0700134052785,0.55956057377781));
#42976=CARTESIAN_POINT('Ctrl Pts',(2.24436971878542,-14.0721491406499,0.441662516279038));
#42977=CARTESIAN_POINT('Ctrl Pts',(2.23571067141573,-14.073524711092,0.323238258334718));
#42978=CARTESIAN_POINT('Ctrl Pts',(2.2257050924945,-14.0751141906309,0.186398348762649));
#42979=CARTESIAN_POINT('Ctrl Pts',(2.22206972520347,-14.0756851929985,0.0492519096262131));
#42980=CARTESIAN_POINT('Ctrl Pts',(2.22477765061414,-14.0752571701311,-0.087675827066048));
#42981=CARTESIAN_POINT('Ctrl Pts',(2.22749342636756,-14.0748279064149,-0.225000520654297));
#42982=CARTESIAN_POINT('Ctrl Pts',(2.23658933237962,-14.0733937867901,-0.362105241912729));
#42983=CARTESIAN_POINT('Ctrl Pts',(2.25202995120888,-14.0709225390114,-0.498460177595558));
#42984=CARTESIAN_POINT('Ctrl Pts',(2.26753718309241,-14.0684406299137,-0.635403368116538));
#42985=CARTESIAN_POINT('Ctrl Pts',(2.28944404469282,-14.0649125984157,-0.771590289741026));
#42986=CARTESIAN_POINT('Ctrl Pts',(2.31770587921582,-14.0602538902201,-0.906484242526269));
#42987=CARTESIAN_POINT('Ctrl Pts',(2.33011188776182,-14.0582088717468,-0.965698216399587));
#42988=CARTESIAN_POINT('Ctrl Pts',(2.34374232952329,-14.0559453130119,-1.02466304565376));
#42989=CARTESIAN_POINT('Ctrl Pts',(2.35859284151951,-14.0534529496467,-1.08333333333318));
#42990=CARTESIAN_POINT('',(2.69569375163578,-14.9004267538186,1.08333333333334));
#42991=CARTESIAN_POINT('Ctrl Pts',(2.6956937516358,-14.9004267538186,1.08333333333334));
#42992=CARTESIAN_POINT('Ctrl Pts',(2.62284674626782,-14.8066618988742,1.08333333333334));
#42993=CARTESIAN_POINT('Ctrl Pts',(2.56054033827465,-14.7041615792632,1.08333333333334));
#42994=CARTESIAN_POINT('Ctrl Pts',(2.43503901504795,-14.4435553962848,1.08333333333334));
#42995=CARTESIAN_POINT('Ctrl Pts',(2.37688304383586,-14.2404175142916,1.08333333333334));
#42996=CARTESIAN_POINT('Ctrl Pts',(2.35859284152042,-14.0534529496557,1.08333333333334));
#42997=CARTESIAN_POINT('Ctrl Pts',(2.69569375163578,-14.9004267538186,-1.08333333333333));
#42998=CARTESIAN_POINT('Ctrl Pts',(2.65885518901859,-14.9070913604575,-0.956888632103347));
#42999=CARTESIAN_POINT('Ctrl Pts',(2.62852794948137,-14.9124412415715,-0.828820583351256));
#43000=CARTESIAN_POINT('Ctrl Pts',(2.60478912083403,-14.9165866029902,-0.699646919261879));
#43001=CARTESIAN_POINT('Ctrl Pts',(2.58117511159368,-14.9207101679857,-0.571152453813268));
#43002=CARTESIAN_POINT('Ctrl Pts',(2.56408033836306,-14.9236419130061,-0.441563969171648));
#43003=CARTESIAN_POINT('Ctrl Pts',(2.55357092618676,-14.9254399524253,-0.311391073637824));
#43004=CARTESIAN_POINT('Ctrl Pts',(2.54314585302948,-14.9272235624095,-0.182262827807427));
#43005=CARTESIAN_POINT('Ctrl Pts',(2.53920083715778,-14.927891621514,-0.0525595133520343));
#43006=CARTESIAN_POINT('Ctrl Pts',(2.54179158298272,-14.9274504788058,0.077221432194672));
#43007=CARTESIAN_POINT('Ctrl Pts',(2.54355857371286,-14.9271496020974,0.165737150534507));
#43008=CARTESIAN_POINT('Ctrl Pts',(2.54836567846244,-14.9263317077699,0.254288981130285));
#43009=CARTESIAN_POINT('Ctrl Pts',(2.55622822284789,-14.9249850760809,0.342719102199546));
#43010=CARTESIAN_POINT('Ctrl Pts',(2.56808166802554,-14.9229549158531,0.47603492730158));
#43011=CARTESIAN_POINT('Ctrl Pts',(2.58681028013297,-14.9197373081624,0.608312350205393));
#43012=CARTESIAN_POINT('Ctrl Pts',(2.61224028910069,-14.9152835347009,0.739057191237091));
#43013=CARTESIAN_POINT('Ctrl Pts',(2.63481838123332,-14.9113292416576,0.855139299993913));
#43014=CARTESIAN_POINT('Ctrl Pts',(2.66267894744191,-14.9063995895532,0.970013302477622));
#43015=CARTESIAN_POINT('Ctrl Pts',(2.69569375163578,-14.9004267538186,1.08333333333334));
#43016=CARTESIAN_POINT('Origin',(6.1828432824253,-12.8388063676094,4.9761330016223E-15));
#43017=CARTESIAN_POINT('',(9.43214127690845,-11.8458513067217,1.08333333333334));
#43018=CARTESIAN_POINT('',(9.24400314381522,-11.3646294742516,1.08333333333334));
#43019=CARTESIAN_POINT('Origin',(6.1828432824253,-12.8388063676094,1.08333333333334));
#43020=CARTESIAN_POINT('',(9.43214127690845,-11.8458513067217,-1.08333333333333));
#43021=CARTESIAN_POINT('Ctrl Pts',(9.43214127690846,-11.8458513067217,-1.08333333333333));
#43022=CARTESIAN_POINT('Ctrl Pts',(9.52751574438875,-11.7699103356432,-0.727666221822791));
#43023=CARTESIAN_POINT('Ctrl Pts',(9.57300195159016,-11.7323107648652,-0.352782973842771));
#43024=CARTESIAN_POINT('Ctrl Pts',(9.57300195159016,-11.7323107648652,0.35278297384278));
#43025=CARTESIAN_POINT('Ctrl Pts',(9.52751574438876,-11.7699103356432,0.7276662218228));
#43026=CARTESIAN_POINT('Ctrl Pts',(9.43214127690846,-11.8458513067217,1.08333333333334));
#43027=CARTESIAN_POINT('',(9.04642813528394,-11.0102060831368,-1.08333333333333));
#43028=CARTESIAN_POINT('Origin',(6.1828432824253,-12.8388063676094,-1.08333333333333));
#43029=CARTESIAN_POINT('',(9.04642813528394,-11.0102060831368,1.08333333333334));
#43030=CARTESIAN_POINT('Ctrl Pts',(9.04642813528396,-11.0102060831368,1.08333333333334));
#43031=CARTESIAN_POINT('Ctrl Pts',(9.13511003678174,-10.9373414661857,0.725928647976586));
#43032=CARTESIAN_POINT('Ctrl Pts',(9.17698017417438,-10.9016299186319,0.352039859176995));
#43033=CARTESIAN_POINT('Ctrl Pts',(9.17698017417438,-10.9016299186319,-0.352039859176985));
#43034=CARTESIAN_POINT('Ctrl Pts',(9.13511003678174,-10.9373414661857,-0.725928647976577));
#43035=CARTESIAN_POINT('Ctrl Pts',(9.04642813528395,-11.0102060831368,-1.08333333333333));
#43036=CARTESIAN_POINT('Origin',(6.1828432824253,-12.8388063676094,1.08333333333334));
#43037=CARTESIAN_POINT('',(3.12168342103538,-14.3129832609672,1.08333333333334));
#43038=CARTESIAN_POINT('Origin',(6.1828432824253,-12.8388063676094,4.9761330016223E-15));
#43039=CARTESIAN_POINT('',(2.96777005866014,-13.9375335292483,1.08333333333334));
#43040=CARTESIAN_POINT('Origin',(6.1828432824253,-12.8388063676094,1.08333333333334));
#43041=CARTESIAN_POINT('',(2.96777005866014,-13.9375335292483,-1.08333333333333));
#43042=CARTESIAN_POINT('Ctrl Pts',(2.96777005866014,-13.9375335292483,-1.08333333333333));
#43043=CARTESIAN_POINT('Ctrl Pts',(2.85550994597651,-13.9614374861791,-0.725928647976576));
#43044=CARTESIAN_POINT('Ctrl Pts',(2.80148393014454,-13.9719070920595,-0.352039859176985));
#43045=CARTESIAN_POINT('Ctrl Pts',(2.80148393014454,-13.9719070920595,5.10230940761107E-15));
#43046=CARTESIAN_POINT('Ctrl Pts',(2.80148393014454,-13.9719070920595,0.352039859176993));
#43047=CARTESIAN_POINT('Ctrl Pts',(2.85550994597651,-13.9614374861791,0.725928647976584));
#43048=CARTESIAN_POINT('Ctrl Pts',(2.96777005866014,-13.9375335292483,1.08333333333333));
#43049=CARTESIAN_POINT('',(3.38061559238708,-14.7601124814491,-1.08333333333333));
#43050=CARTESIAN_POINT('Origin',(6.1828432824253,-12.8388063676094,-1.08333333333333));
#43051=CARTESIAN_POINT('',(3.38061559238708,-14.7601124814491,1.08333333333334));
#43052=CARTESIAN_POINT('Ctrl Pts',(3.3806155923871,-14.7601124814491,1.08333333333334));
#43053=CARTESIAN_POINT('Ctrl Pts',(3.26177754255705,-14.7873308217381,0.727666221822799));
#43054=CARTESIAN_POINT('Ctrl Pts',(3.20402082808022,-14.7994504216119,0.35278297384278));
#43055=CARTESIAN_POINT('Ctrl Pts',(3.20402082808022,-14.7994504216119,5.42337291349619E-15));
#43056=CARTESIAN_POINT('Ctrl Pts',(3.20402082808022,-14.7994504216119,-0.35278297384277));
#43057=CARTESIAN_POINT('Ctrl Pts',(3.26177754255705,-14.7873308217381,-0.727666221822788));
#43058=CARTESIAN_POINT('Ctrl Pts',(3.3806155923871,-14.7601124814491,-1.08333333333333));
#43059=CARTESIAN_POINT('Origin',(6.1828432824253,-12.8388063676094,1.08333333333334));
#43060=CARTESIAN_POINT('',(5.79568548444348,-12.0348649162504,-3.45272288248773));
#43061=CARTESIAN_POINT('Origin',(5.79568548444348,-12.0348649162504,4.66453708897011E-15));
#43062=CARTESIAN_POINT('',(6.57000108040713,-13.6427478189685,-3.45272288248772));
#43063=CARTESIAN_POINT('Origin',(6.57000108040713,-13.6427478189685,5.28772891427449E-15));
#43064=CARTESIAN_POINT('Origin',(13.892722748591,-3.17092330887735,3.20017169526122E-15));
#43065=CARTESIAN_POINT('',(14.7626584240763,-3.36948044994605,3.96060240207311));
#43066=CARTESIAN_POINT('Origin',(14.7626584240763,-3.36948044994605,3.40056031423575E-15));
#43067=CARTESIAN_POINT('',(13.0227870731057,-2.97236616780864,3.96060240207311));
#43068=CARTESIAN_POINT('Origin',(13.892722748591,-3.17092330887735,2.5198520116158));
#43069=CARTESIAN_POINT('Origin',(13.0227870731057,-2.97236616780865,2.9997830762867E-15));
#43070=CARTESIAN_POINT('',(14.2259398250621,0.827729480997053,-1.08333333333333));
#43071=CARTESIAN_POINT('',(15.1266902369927,0.68754979644376,-1.08333333333333));
#43072=CARTESIAN_POINT('Ctrl Pts',(14.2259398250621,0.827729480997104,-1.08333333333333));
#43073=CARTESIAN_POINT('Ctrl Pts',(14.4122867506183,0.85150138178118,-1.08333333333333));
#43074=CARTESIAN_POINT('Ctrl Pts',(14.6232724628281,0.840005933409976,-1.08333333333333));
#43075=CARTESIAN_POINT('Ctrl Pts',(14.9052713763609,0.775641521611009,-1.08333333333333));
#43076=CARTESIAN_POINT('Ctrl Pts',(15.0190662790554,0.737705732201359,-1.08333333333333));
#43077=CARTESIAN_POINT('Ctrl Pts',(15.1266902369927,0.687549796443767,-1.08333333333333));
#43078=CARTESIAN_POINT('',(15.1266902369927,0.687549796443762,1.08333333333334));
#43079=CARTESIAN_POINT('Ctrl Pts',(15.1266902369927,0.687549796443768,1.08333333333334));
#43080=CARTESIAN_POINT('Ctrl Pts',(15.1249773086751,0.725235701077452,0.955915065626868));
#43081=CARTESIAN_POINT('Ctrl Pts',(15.1234319803901,0.756223536825589,0.826701571451108));
#43082=CARTESIAN_POINT('Ctrl Pts',(15.122183667988,0.780412301388443,0.696211209493001));
#43083=CARTESIAN_POINT('Ctrl Pts',(15.1209550316477,0.804219799510377,0.567777653526322));
#43084=CARTESIAN_POINT('Ctrl Pts',(15.12001416535,0.821440959530357,0.43810716485706));
#43085=CARTESIAN_POINT('Ctrl Pts',(15.1194343523859,0.831977831684773,0.307693975182356));
#43086=CARTESIAN_POINT('Ctrl Pts',(15.1189800281283,0.840234212474528,0.205506064179778));
#43087=CARTESIAN_POINT('Ctrl Pts',(15.1187464308798,0.844386527178536,0.102862147741283));
#43088=CARTESIAN_POINT('Ctrl Pts',(15.1187464308798,0.844386527178536,1.99840144432528E-15));
#43089=CARTESIAN_POINT('Ctrl Pts',(15.1187464308798,0.844386527178536,-0.130666807305585));
#43090=CARTESIAN_POINT('Ctrl Pts',(15.1191251529677,0.837684329050871,-0.261069786498764));
#43091=CARTESIAN_POINT('Ctrl Pts',(15.1198518432089,0.824355801783881,-0.390710450871172));
#43092=CARTESIAN_POINT('Ctrl Pts',(15.1205872590302,0.810867235029882,-0.521907748246314));
#43093=CARTESIAN_POINT('Ctrl Pts',(15.1216790167187,0.790592205023559,-0.652324314224285));
#43094=CARTESIAN_POINT('Ctrl Pts',(15.1230415909943,0.763606761086929,-0.781443489202972));
#43095=CARTESIAN_POINT('Ctrl Pts',(15.1241128691977,0.742390363262186,-0.882959098491574));
#43096=CARTESIAN_POINT('Ctrl Pts',(15.1253504648421,0.717025942630064,-0.983672743459537));
#43097=CARTESIAN_POINT('Ctrl Pts',(15.1266902369927,0.687549796443768,-1.08333333333333));
#43098=CARTESIAN_POINT('',(14.2259398250621,0.827729480997055,1.08333333333334));
#43099=CARTESIAN_POINT('Ctrl Pts',(14.2259398250621,0.827729480997104,1.08333333333333));
#43100=CARTESIAN_POINT('Ctrl Pts',(14.4122867506183,0.85150138178118,1.08333333333333));
#43101=CARTESIAN_POINT('Ctrl Pts',(14.6232724628281,0.840005933409977,1.08333333333333));
#43102=CARTESIAN_POINT('Ctrl Pts',(14.9052713763609,0.775641521611009,1.08333333333333));
#43103=CARTESIAN_POINT('Ctrl Pts',(15.0190662790554,0.73770573220136,1.08333333333333));
#43104=CARTESIAN_POINT('Ctrl Pts',(15.1266902369927,0.687549796443768,1.08333333333333));
#43105=CARTESIAN_POINT('Ctrl Pts',(14.2259398250621,0.8277294809971,-1.08333333333334));
#43106=CARTESIAN_POINT('Ctrl Pts',(14.2239464151202,0.861989623387911,-0.949622058007612));
#43107=CARTESIAN_POINT('Ctrl Pts',(14.2222079250172,0.889808711690379,-0.814376693553152));
#43108=CARTESIAN_POINT('Ctrl Pts',(14.2208398148552,0.911161325030034,-0.678132403727965));
#43109=CARTESIAN_POINT('Ctrl Pts',(14.2194782068654,0.932412456504566,-0.542535637670654));
#43110=CARTESIAN_POINT('Ctrl Pts',(14.2184834780892,0.947258512328438,-0.40594941879874));
#43111=CARTESIAN_POINT('Ctrl Pts',(14.2179179597194,0.955671957676133,-0.268901316711642));
#43112=CARTESIAN_POINT('Ctrl Pts',(14.2175487034788,0.961165532006069,-0.179415511018676));
#43113=CARTESIAN_POINT('Ctrl Pts',(14.2173613909827,0.963916530720146,-0.0897327832366183));
#43114=CARTESIAN_POINT('Ctrl Pts',(14.2173613909827,0.963916530720146,-1.06581410364015E-14));
#43115=CARTESIAN_POINT('Ctrl Pts',(14.2173613909827,0.963916530720146,0.13757393698032));
#43116=CARTESIAN_POINT('Ctrl Pts',(14.2178040883167,0.957451598945758,0.274951212619625));
#43117=CARTESIAN_POINT('Ctrl Pts',(14.2186598102071,0.944570379379524,0.411612406214599));
#43118=CARTESIAN_POINT('Ctrl Pts',(14.2195221530139,0.931589494866494,0.549330978772693));
#43119=CARTESIAN_POINT('Ctrl Pts',(14.2208039138492,0.912092599491427,0.686322345436757));
#43120=CARTESIAN_POINT('Ctrl Pts',(14.222421741201,0.886126297665472,0.822054935347047));
#43121=CARTESIAN_POINT('Ctrl Pts',(14.2234666476786,0.869355437073955,0.909720570537178));
#43122=CARTESIAN_POINT('Ctrl Pts',(14.2246506698206,0.849885807807131,0.996861109122824));
#43123=CARTESIAN_POINT('Ctrl Pts',(14.2259398250621,0.827729480997101,1.08333333333335));
#43124=CARTESIAN_POINT('',(13.3303603014235,-7.18268588222768,-1.08333333333333));
#43125=CARTESIAN_POINT('',(12.4579905368411,-6.91816245718305,-1.08333333333333));
#43126=CARTESIAN_POINT('Ctrl Pts',(13.3303603014235,-7.18268588222769,-1.08333333333333));
#43127=CARTESIAN_POINT('Ctrl Pts',(13.2116326209361,-7.18117853359731,-1.08333333333333));
#43128=CARTESIAN_POINT('Ctrl Pts',(13.0926472341269,-7.16598374096113,-1.08333333333333));
#43129=CARTESIAN_POINT('Ctrl Pts',(12.8106483205942,-7.10161932916216,-1.08333333333333));
#43130=CARTESIAN_POINT('Ctrl Pts',(12.6155690741987,-7.02043310055321,-1.08333333333333));
#43131=CARTESIAN_POINT('Ctrl Pts',(12.4579905368414,-6.91816245718254,-1.08333333333333));
#43132=CARTESIAN_POINT('',(12.4579905368491,-6.91816245718746,1.08333333333334));
#43133=CARTESIAN_POINT('Ctrl Pts',(12.4579905368414,-6.91816245718254,1.08333333333318));
#43134=CARTESIAN_POINT('Ctrl Pts',(12.4412857888865,-6.94824379644432,0.949270311030419));
#43135=CARTESIAN_POINT('Ctrl Pts',(12.4276027080704,-6.97263587945666,0.813521288368017));
#43136=CARTESIAN_POINT('Ctrl Pts',(12.4170780656486,-6.99132836531005,0.676607052101155));
#43137=CARTESIAN_POINT('Ctrl Pts',(12.4080806643215,-7.00730836636693,0.559560573777918));
#43138=CARTESIAN_POINT('Ctrl Pts',(12.4013908554088,-7.019122574986,0.441662516279092));
#43139=CARTESIAN_POINT('Ctrl Pts',(12.397067491958,-7.0267501449702,0.323238258334718));
#43140=CARTESIAN_POINT('Ctrl Pts',(12.3920718206831,-7.03556384585387,0.186398348762654));
#43141=CARTESIAN_POINT('Ctrl Pts',(12.3902516338787,-7.03876210460539,0.0492519096262223));
#43142=CARTESIAN_POINT('Ctrl Pts',(12.3916053560035,-7.03637809537437,-0.0876758270660355));
#43143=CARTESIAN_POINT('Ctrl Pts',(12.3929630026023,-7.03398717484161,-0.225000520654302));
#43144=CARTESIAN_POINT('Ctrl Pts',(12.3975129673672,-7.02598155019911,-0.362105241912753));
#43145=CARTESIAN_POINT('Ctrl Pts',(12.4052079364272,-7.01236879050172,-0.498460177595601));
#43146=CARTESIAN_POINT('Ctrl Pts',(12.4129361026925,-6.99869730339771,-0.635403368116608));
#43147=CARTESIAN_POINT('Ctrl Pts',(12.4238364813948,-6.9793701376568,-0.771590289741124));
#43148=CARTESIAN_POINT('Ctrl Pts',(12.4378151222668,-6.95436948862457,-0.906484242526394));
#43149=CARTESIAN_POINT('Ctrl Pts',(12.4439512822523,-6.94339503240884,-0.96569821639967));
#43150=CARTESIAN_POINT('Ctrl Pts',(12.4506800022041,-6.93132701813272,-1.0246630456538));
#43151=CARTESIAN_POINT('Ctrl Pts',(12.4579905368414,-6.91816245718254,-1.08333333333318));
#43152=CARTESIAN_POINT('',(13.3303603014235,-7.18268588222768,1.08333333333334));
#43153=CARTESIAN_POINT('Ctrl Pts',(13.3303603014235,-7.18268588222769,1.08333333333333));
#43154=CARTESIAN_POINT('Ctrl Pts',(13.2116326209361,-7.18117853359731,1.08333333333333));
#43155=CARTESIAN_POINT('Ctrl Pts',(13.0926472341269,-7.16598374096113,1.08333333333333));
#43156=CARTESIAN_POINT('Ctrl Pts',(12.810648320597,-7.10161932916281,1.08333333333333));
#43157=CARTESIAN_POINT('Ctrl Pts',(12.6155690742049,-7.020433100556,1.08333333333333));
#43158=CARTESIAN_POINT('Ctrl Pts',(12.4579905368491,-6.91816245718749,1.08333333333333));
#43159=CARTESIAN_POINT('Ctrl Pts',(13.3303603014235,-7.18268588222769,-1.08333333333333));
#43160=CARTESIAN_POINT('Ctrl Pts',(13.3126024326051,-7.21564274452345,-0.956888632103319));
#43161=CARTESIAN_POINT('Ctrl Pts',(13.2978764135175,-7.24268913148574,-0.828820583351199));
#43162=CARTESIAN_POINT('Ctrl Pts',(13.2863164700112,-7.26383348564869,-0.699646919261793));
#43163=CARTESIAN_POINT('Ctrl Pts',(13.2748173090023,-7.28486666222208,-0.57115245381317));
#43164=CARTESIAN_POINT('Ctrl Pts',(13.2664510227834,-7.30005980724128,-0.441563969171537));
#43165=CARTESIAN_POINT('Ctrl Pts',(13.2613042752927,-7.30939745578421,-0.311391073637702));
#43166=CARTESIAN_POINT('Ctrl Pts',(13.2561988309336,-7.31866016882124,-0.182262827807302));
#43167=CARTESIAN_POINT('Ctrl Pts',(13.2542614634095,-7.32216103446727,-0.0525595133519065));
#43168=CARTESIAN_POINT('Ctrl Pts',(13.2555318677529,-7.3198604598385,0.0772214321948015));
#43169=CARTESIAN_POINT('Ctrl Pts',(13.2563983335702,-7.31829137729713,0.16573715053459));
#43170=CARTESIAN_POINT('Ctrl Pts',(13.2587560588235,-7.31402308269219,0.254288981130321));
#43171=CARTESIAN_POINT('Ctrl Pts',(13.2626054360147,-7.30703628683439,0.342719102199534));
#43172=CARTESIAN_POINT('Ctrl Pts',(13.2684086950193,-7.29650310602066,0.476034927301568));
#43173=CARTESIAN_POINT('Ctrl Pts',(13.2775701666805,-7.2798543418706,0.608312350205377));
#43174=CARTESIAN_POINT('Ctrl Pts',(13.289943417625,-7.25719547792716,0.739057191237071));
#43175=CARTESIAN_POINT('Ctrl Pts',(13.300929037023,-7.23707775329776,0.8551392999939));
#43176=CARTESIAN_POINT('Ctrl Pts',(13.3144456587152,-7.21222189770271,0.970013302477615));
#43177=CARTESIAN_POINT('Ctrl Pts',(13.3303603014235,-7.18268588222769,1.08333333333334));
#43178=CARTESIAN_POINT('Origin',(13.892722748591,-3.17092330887735,3.20017169526122E-15));
#43179=CARTESIAN_POINT('',(15.1423033840733,-0.0114224867026808,1.08333333333334));
#43180=CARTESIAN_POINT('',(14.6487667980729,0.141522102769127,1.08333333333334));
#43181=CARTESIAN_POINT('Origin',(13.892722748591,-3.17092330887735,1.08333333333334));
#43182=CARTESIAN_POINT('',(15.1423033840733,-0.0114224867026808,-1.08333333333333));
#43183=CARTESIAN_POINT('Ctrl Pts',(15.1423033840733,-0.0114224867026917,
-1.08333333333333));
#43184=CARTESIAN_POINT('Ctrl Pts',(15.1423953499066,0.110492695607724,-0.727666221822789));
#43185=CARTESIAN_POINT('Ctrl Pts',(15.1413590080604,0.169498193350193,-0.352782973842772));
#43186=CARTESIAN_POINT('Ctrl Pts',(15.1413590080604,0.169498193350193,0.352782973842778));
#43187=CARTESIAN_POINT('Ctrl Pts',(15.1423953499066,0.110492695607724,0.727666221822797));
#43188=CARTESIAN_POINT('Ctrl Pts',(15.1423033840733,-0.0114224867026924,
1.08333333333334));
#43189=CARTESIAN_POINT('',(14.2484814298548,0.208031110850763,-1.08333333333333));
#43190=CARTESIAN_POINT('Origin',(13.892722748591,-3.17092330887735,-1.08333333333333));
#43191=CARTESIAN_POINT('',(14.2484814298548,0.208031110850763,1.08333333333334));
#43192=CARTESIAN_POINT('Ctrl Pts',(14.2484814298548,0.208031110850764,1.08333333333334));
#43193=CARTESIAN_POINT('Ctrl Pts',(14.2468058395578,0.322795758952199,0.725928647976585));
#43194=CARTESIAN_POINT('Ctrl Pts',(14.2449910310593,0.377796936249431,0.352039859176993));
#43195=CARTESIAN_POINT('Ctrl Pts',(14.2449910310593,0.37779693624943,-0.352039859176987));
#43196=CARTESIAN_POINT('Ctrl Pts',(14.2468058395578,0.322795758952199,-0.725928647976577));
#43197=CARTESIAN_POINT('Ctrl Pts',(14.2484814298548,0.208031110850765,-1.08333333333333));
#43198=CARTESIAN_POINT('Origin',(13.892722748591,-3.17092330887735,1.08333333333334));
#43199=CARTESIAN_POINT('',(13.1366786991091,-6.48336872052383,1.08333333333334));
#43200=CARTESIAN_POINT('Origin',(13.892722748591,-3.17092330887735,3.20017169526122E-15));
#43201=CARTESIAN_POINT('',(12.7471768669564,-6.36961395396396,1.08333333333334));
#43202=CARTESIAN_POINT('Origin',(13.892722748591,-3.17092330887735,1.08333333333334));
#43203=CARTESIAN_POINT('',(12.7471768669564,-6.36961395396396,-1.08333333333333));
#43204=CARTESIAN_POINT('Ctrl Pts',(12.7471768669564,-6.36961395396397,-1.08333333333334));
#43205=CARTESIAN_POINT('Ctrl Pts',(12.6958726976266,-6.47228631765585,-0.725928647976583));
#43206=CARTESIAN_POINT('Ctrl Pts',(12.6703734952067,-6.52105325020152,-0.352039859176989));
#43207=CARTESIAN_POINT('Ctrl Pts',(12.6703734952067,-6.52105325020152,3.73360976135914E-15));
#43208=CARTESIAN_POINT('Ctrl Pts',(12.6703734952067,-6.52105325020152,0.352039859176996));
#43209=CARTESIAN_POINT('Ctrl Pts',(12.6958726976266,-6.47228631765585,0.725928647976591));
#43210=CARTESIAN_POINT('Ctrl Pts',(12.7471768669564,-6.36961395396397,1.08333333333335));
#43211=CARTESIAN_POINT('',(13.6476999686242,-6.55970790622078,-1.08333333333333));
#43212=CARTESIAN_POINT('Origin',(13.892722748591,-3.17092330887735,-1.08333333333333));
#43213=CARTESIAN_POINT('',(13.6476999686242,-6.55970790622078,1.08333333333334));
#43214=CARTESIAN_POINT('Ctrl Pts',(13.6476999686242,-6.55970790622078,1.08333333333334));
#43215=CARTESIAN_POINT('Ctrl Pts',(13.5948858118209,-6.66958959248674,0.727666221822799));
#43216=CARTESIAN_POINT('Ctrl Pts',(13.5683505740919,-6.72230205711255,0.35278297384278));
#43217=CARTESIAN_POINT('Ctrl Pts',(13.5683505740919,-6.72230205711255,3.93962482987281E-15));
#43218=CARTESIAN_POINT('Ctrl Pts',(13.5683505740919,-6.72230205711255,-0.352782973842771));
#43219=CARTESIAN_POINT('Ctrl Pts',(13.5948858118209,-6.66958959248674,-0.72766622182279));
#43220=CARTESIAN_POINT('Ctrl Pts',(13.6476999686242,-6.55970790622078,-1.08333333333333));
#43221=CARTESIAN_POINT('Origin',(13.892722748591,-3.17092330887735,1.08333333333334));
#43222=CARTESIAN_POINT('',(13.0227870731057,-2.97236616780865,-3.45272288248773));
#43223=CARTESIAN_POINT('Origin',(13.0227870731057,-2.97236616780865,2.9997830762867E-15));
#43224=CARTESIAN_POINT('',(14.7626584240763,-3.36948044994605,-3.45272288248773));
#43225=CARTESIAN_POINT('Origin',(14.7626584240763,-3.36948044994605,3.40056031423575E-15));
#43226=CARTESIAN_POINT('Origin',(11.1410986251693,8.88472967648709,9.85584169237555E-16));
#43227=CARTESIAN_POINT('',(11.8387328710639,9.44107442276104,3.96060240207311));
#43228=CARTESIAN_POINT('Origin',(11.8387328710639,9.44107442276104,1.0472995612114E-15));
#43229=CARTESIAN_POINT('',(10.4434643792748,8.32838493021314,3.96060240207311));
#43230=CARTESIAN_POINT('Origin',(11.1410986251693,8.88472967648709,2.5198520116158));
#43231=CARTESIAN_POINT('Origin',(10.4434643792748,8.32838493021314,9.23868777263706E-16));
#43232=CARTESIAN_POINT('',(8.89378902201275,12.2552029391784,-1.08333333331655));
#43233=CARTESIAN_POINT('',(8.89378902201677,12.2552029391754,1.08333333333333));
#43234=CARTESIAN_POINT('Ctrl Pts',(8.89378902201274,12.2552029391784,-1.08333333331655));
#43235=CARTESIAN_POINT('Ctrl Pts',(8.86335293025879,12.2772908784853,-0.956315399884826));
#43236=CARTESIAN_POINT('Ctrl Pts',(8.83824313040494,12.2953456493747,-0.827586922367285));
#43237=CARTESIAN_POINT('Ctrl Pts',(8.81859777764014,12.3094197866805,-0.69766772380084));
#43238=CARTESIAN_POINT('Ctrl Pts',(8.7991879276401,12.3233252073292,-0.569305958731489));
#43239=CARTESIAN_POINT('Ctrl Pts',(8.78511225071473,12.3333449381983,-0.439781849534452));
#43240=CARTESIAN_POINT('Ctrl Pts',(8.77647376760361,12.3394890678296,-0.309596747993595));
#43241=CARTESIAN_POINT('Ctrl Pts',(8.76964787761092,12.344343988818,-0.206728088024587));
#43242=CARTESIAN_POINT('Ctrl Pts',(8.76621624622163,12.3467783236357,-0.103446722778746));
#43243=CARTESIAN_POINT('Ctrl Pts',(8.76621624622163,12.3467783236357,-7.54951656745106E-15));
#43244=CARTESIAN_POINT('Ctrl Pts',(8.76621624622163,12.3467783236357,0.130951008152141));
#43245=CARTESIAN_POINT('Ctrl Pts',(8.77171477448527,12.3428797767713,0.261548325668487));
#43246=CARTESIAN_POINT('Ctrl Pts',(8.78261416841303,12.3351194002049,0.391301356121213));
#43247=CARTESIAN_POINT('Ctrl Pts',(8.79368558213778,12.3272365454154,0.523102215114213));
#43248=CARTESIAN_POINT('Ctrl Pts',(8.81032969837903,12.3153689336875,0.654031926803563));
#43249=CARTESIAN_POINT('Ctrl Pts',(8.83241243050519,12.2995110840219,0.783576297698762));
#43250=CARTESIAN_POINT('Ctrl Pts',(8.84960195907419,12.2871670969504,0.88441557119687));
#43251=CARTESIAN_POINT('Ctrl Pts',(8.87008627043973,12.2724043900869,0.984415425401903));
#43252=CARTESIAN_POINT('Ctrl Pts',(8.89378902201675,12.2552029391755,1.08333333333333));
#43253=CARTESIAN_POINT('',(8.22258343557123,11.6383685130292,1.08333333333333));
#43254=CARTESIAN_POINT('Ctrl Pts',(8.89378902201675,12.2552029391755,1.08333333333333));
#43255=CARTESIAN_POINT('Ctrl Pts',(8.78751907456219,12.2023537225759,1.08333333333333));
#43256=CARTESIAN_POINT('Ctrl Pts',(8.68681488082489,12.1369760343758,1.08333333333333));
#43257=CARTESIAN_POINT('Ctrl Pts',(8.46069343470621,11.9566501984405,1.08333333333333));
#43258=CARTESIAN_POINT('Ctrl Pts',(8.31988542322917,11.7983921800676,1.08333333333333));
#43259=CARTESIAN_POINT('Ctrl Pts',(8.22258343557176,11.6383685130289,1.08333333333333));
#43260=CARTESIAN_POINT('',(8.22258343557175,11.6383685130288,-1.08333333333333));
#43261=CARTESIAN_POINT('Ctrl Pts',(8.2225834355717,11.6383685130289,1.08333333333318));
#43262=CARTESIAN_POINT('Ctrl Pts',(8.19448780675769,11.6582182584498,0.949301954017324));
#43263=CARTESIAN_POINT('Ctrl Pts',(8.17159767874311,11.6742430454627,0.81366496302888));
#43264=CARTESIAN_POINT('Ctrl Pts',(8.15402161030241,11.6865063889394,0.67695567866062));
#43265=CARTESIAN_POINT('Ctrl Pts',(8.13658119548769,11.6986750828637,0.541301528447691));
#43266=CARTESIAN_POINT('Ctrl Pts',(8.12437307855494,11.7071402381473,0.40459157308691));
#43267=CARTESIAN_POINT('Ctrl Pts',(8.1174733585697,11.7119223986889,0.26734687734235));
#43268=CARTESIAN_POINT('Ctrl Pts',(8.11300215046573,11.7150213700985,0.178408544025479));
#43269=CARTESIAN_POINT('Ctrl Pts',(8.11075954642938,11.7165728598428,0.0892456520429063));
#43270=CARTESIAN_POINT('Ctrl Pts',(8.11075954642938,11.7165728598428,-1.33226762955019E-15));
#43271=CARTESIAN_POINT('Ctrl Pts',(8.11075954642938,11.7165728598428,-0.137335411050026));
#43272=CARTESIAN_POINT('Ctrl Pts',(8.11607262981309,11.7129002012938,-0.274553571737022));
#43273=CARTESIAN_POINT('Ctrl Pts',(8.12665801674411,11.7055512249056,-0.411127959090392));
#43274=CARTESIAN_POINT('Ctrl Pts',(8.13729388250879,11.698167203246,-0.548353632582512));
#43275=CARTESIAN_POINT('Ctrl Pts',(8.15325248641432,11.6870716767896,-0.684929378140945));
#43276=CARTESIAN_POINT('Ctrl Pts',(8.17446212457132,11.6722178258439,-0.820321104282498));
#43277=CARTESIAN_POINT('Ctrl Pts',(8.18828255682692,11.6625388940673,-0.908543834215877));
#43278=CARTESIAN_POINT('Ctrl Pts',(8.20433194575505,11.6512633098961,-0.9962638332735));
#43279=CARTESIAN_POINT('Ctrl Pts',(8.22258343557176,11.6383685130288,-1.08333333333334));
#43280=CARTESIAN_POINT('Ctrl Pts',(8.89378902201473,12.2552029391744,-1.08333333333333));
#43281=CARTESIAN_POINT('Ctrl Pts',(8.7875190745609,12.202353722575,-1.08333333333333));
#43282=CARTESIAN_POINT('Ctrl Pts',(8.68681488082435,12.1369760343753,-1.08333333333333));
#43283=CARTESIAN_POINT('Ctrl Pts',(8.46069343470619,11.9566501984405,-1.08333333333333));
#43284=CARTESIAN_POINT('Ctrl Pts',(8.31988542322913,11.7983921800676,-1.08333333333333));
#43285=CARTESIAN_POINT('Ctrl Pts',(8.22258343557172,11.6383685130288,-1.08333333333333));
#43286=CARTESIAN_POINT('',(13.9269936544443,5.94376395877129,-1.08333333333333));
#43287=CARTESIAN_POINT('',(13.1762672612271,5.42664547033562,-1.08333333333333));
#43288=CARTESIAN_POINT('Ctrl Pts',(13.9269936544443,5.94376395877129,-1.08333333333333));
#43289=CARTESIAN_POINT('Ctrl Pts',(13.8517896638478,5.85187873682469,-1.08333333333333));
#43290=CARTESIAN_POINT('Ctrl Pts',(13.7657237213495,5.76832601371371,-1.08333333333333));
#43291=CARTESIAN_POINT('Ctrl Pts',(13.5395781511316,5.5879809394513,-1.08333333333333));
#43292=CARTESIAN_POINT('Ctrl Pts',(13.3544742809805,5.48608062863226,-1.08333333333333));
#43293=CARTESIAN_POINT('Ctrl Pts',(13.1762672612269,5.42664547033621,-1.08333333333333));
#43294=CARTESIAN_POINT('',(13.1762672612355,5.42664547033908,1.08333333333333));
#43295=CARTESIAN_POINT('Ctrl Pts',(13.1762672612269,5.42664547033617,1.08333333333318));
#43296=CARTESIAN_POINT('Ctrl Pts',(13.1893705593041,5.39482976422236,0.949270311030452));
#43297=CARTESIAN_POINT('Ctrl Pts',(13.1999097963792,5.36892368585892,0.813521288368082));
#43298=CARTESIAN_POINT('Ctrl Pts',(13.2079621630868,5.34904061477083,0.676607052101254));
#43299=CARTESIAN_POINT('Ctrl Pts',(13.2148460430323,5.33204279546023,0.559560573777983));
#43300=CARTESIAN_POINT('Ctrl Pts',(13.2199117356377,5.31944645364959,0.441662516279123));
#43301=CARTESIAN_POINT('Ctrl Pts',(13.2231796369647,5.31131059989547,0.323238258334714));
#43302=CARTESIAN_POINT('Ctrl Pts',(13.2269557156993,5.30190957419912,0.186398348762647));
#43303=CARTESIAN_POINT('Ctrl Pts',(13.2283213471703,5.2984924131362,0.0492519096262126));
#43304=CARTESIAN_POINT('Ctrl Pts',(13.2273014856384,5.30103720115497,-0.087675827066048));
#43305=CARTESIAN_POINT('Ctrl Pts',(13.2262786675026,5.30358936657715,-0.225000520654307));
#43306=CARTESIAN_POINT('Ctrl Pts',(13.22285647475,5.31213809759657,-0.362105241912749));
#43307=CARTESIAN_POINT('Ctrl Pts',(13.2170113253899,5.32664168351083,-0.498460177595588));
#43308=CARTESIAN_POINT('Ctrl Pts',(13.2111409592133,5.34120783998435,-0.635403368116607));
#43309=CARTESIAN_POINT('Ctrl Pts',(13.2028266475275,5.36178038996296,-0.771590289741134));
#43310=CARTESIAN_POINT('Ctrl Pts',(13.1919958930594,5.38829698119018,-0.906484242526414));
#43311=CARTESIAN_POINT('Ctrl Pts',(13.1872415508606,5.3999368857798,-0.965698216399684));
#43312=CARTESIAN_POINT('Ctrl Pts',(13.1820016856381,5.41272189470467,-1.02466304565381));
#43313=CARTESIAN_POINT('Ctrl Pts',(13.1762672612269,5.42664547033617,-1.08333333333318));
#43314=CARTESIAN_POINT('',(13.9269936544443,5.94376395877129,1.08333333333333));
#43315=CARTESIAN_POINT('Ctrl Pts',(13.9269936544443,5.94376395877129,1.08333333333333));
#43316=CARTESIAN_POINT('Ctrl Pts',(13.8517896638478,5.85187873682469,1.08333333333333));
#43317=CARTESIAN_POINT('Ctrl Pts',(13.7657237213495,5.76832601371371,1.08333333333333));
#43318=CARTESIAN_POINT('Ctrl Pts',(13.5395781511339,5.5879809394531,1.08333333333333));
#43319=CARTESIAN_POINT('Ctrl Pts',(13.3544742809865,5.48608062863536,1.08333333333333));
#43320=CARTESIAN_POINT('Ctrl Pts',(13.1762672612355,5.42664547033908,1.08333333333333));
#43321=CARTESIAN_POINT('Ctrl Pts',(13.9269936544443,5.9437639587713,-1.08333333333333));
#43322=CARTESIAN_POINT('Ctrl Pts',(13.9416885168395,5.90933203032488,-0.95688863210334));
#43323=CARTESIAN_POINT('Ctrl Pts',(13.9536527109305,5.88095561854266,-0.828820583351241));
#43324=CARTESIAN_POINT('Ctrl Pts',(13.9629765258053,5.85873440158633,-0.699646919261855));
#43325=CARTESIAN_POINT('Ctrl Pts',(13.9722513158077,5.83663002439342,-0.571152453813261));
#43326=CARTESIAN_POINT('Ctrl Pts',(13.9789135007645,5.82061622745854,-0.441563969171658));
#43327=CARTESIAN_POINT('Ctrl Pts',(13.9830050237944,5.81077040959811,-0.31139107363785));
#43328=CARTESIAN_POINT('Ctrl Pts',(13.987063711968,5.80100360535004,-0.182262827807452));
#43329=CARTESIAN_POINT('Ctrl Pts',(13.9885928700522,5.79730615639857,-0.0525595133520559));
#43330=CARTESIAN_POINT('Ctrl Pts',(13.9875862925321,5.79973378332923,0.077221432194654));
#43331=CARTESIAN_POINT('Ctrl Pts',(13.9868997670033,5.80138952054645,0.165737150534494));
#43332=CARTESIAN_POINT('Ctrl Pts',(13.9850326975557,5.80589410253397,0.254288981130278));
#43333=CARTESIAN_POINT('Ctrl Pts',(13.9819702480148,5.81325986277498,0.342719102199545));
#43334=CARTESIAN_POINT('Ctrl Pts',(13.977353348451,5.82436436418423,0.476034927301432));
#43335=CARTESIAN_POINT('Ctrl Pts',(13.9700489046451,5.84190742581571,0.608312350205104));
#43336=CARTESIAN_POINT('Ctrl Pts',(13.9600480872369,5.86570879353505,0.739057191236667));
#43337=CARTESIAN_POINT('Ctrl Pts',(13.9511688384277,5.88684089277784,0.855139299993628));
#43338=CARTESIAN_POINT('Ctrl Pts',(13.9401632237805,5.91290598563348,0.970013302477476));
#43339=CARTESIAN_POINT('Ctrl Pts',(13.9269936544443,5.9437639587713,1.08333333333333));
#43340=CARTESIAN_POINT('Origin',(11.1410986251693,8.88472967648709,9.85584169237555E-16));
#43341=CARTESIAN_POINT('',(8.72113759169208,11.2696166353064,1.08333333333333));
#43342=CARTESIAN_POINT('',(9.02271027299523,11.54110464988,1.08333333333333));
#43343=CARTESIAN_POINT('Origin',(11.1410986251693,8.88472967648709,1.08333333333333));
#43344=CARTESIAN_POINT('',(13.2594869773434,6.22835470309422,1.08333333333333));
#43345=CARTESIAN_POINT('Origin',(11.1410986251693,8.88472967648709,9.85584169237555E-16));
#43346=CARTESIAN_POINT('',(12.9276994994135,5.9947548451011,1.08333333333333));
#43347=CARTESIAN_POINT('Origin',(11.1410986251693,8.88472967648709,1.08333333333333));
#43348=CARTESIAN_POINT('',(12.9276994994135,5.9947548451011,-1.08333333333333));
#43349=CARTESIAN_POINT('Ctrl Pts',(12.9276994994135,5.9947548451011,-1.08333333333333));
#43350=CARTESIAN_POINT('Ctrl Pts',(12.9759843593573,5.89062845864264,-0.725928647976581));
#43351=CARTESIAN_POINT('Ctrl Pts',(12.9982133898606,5.84028669430273,-0.352039859176989));
#43352=CARTESIAN_POINT('Ctrl Pts',(12.9982133898606,5.84028669430273,9.85141416048961E-16));
#43353=CARTESIAN_POINT('Ctrl Pts',(12.9982133898606,5.84028669430273,0.35203985917699));
#43354=CARTESIAN_POINT('Ctrl Pts',(12.9759843593573,5.89062845864264,0.72592864797658));
#43355=CARTESIAN_POINT('Ctrl Pts',(12.9276994994135,5.9947548451011,1.08333333333333));
#43356=CARTESIAN_POINT('',(13.6377879061428,6.58029051604763,-1.08333333333333));
#43357=CARTESIAN_POINT('Origin',(11.1410986251693,8.88472967648709,-1.08333333333333));
#43358=CARTESIAN_POINT('',(13.6377879061428,6.58029051604763,1.08333333333333));
#43359=CARTESIAN_POINT('Ctrl Pts',(13.6377879061428,6.58029051604764,1.08333333333332));
#43360=CARTESIAN_POINT('Ctrl Pts',(13.6907677796515,6.47048863474093,0.727666221822788));
#43361=CARTESIAN_POINT('Ctrl Pts',(13.7154355939006,6.41687686636464,0.352782973842773));
#43362=CARTESIAN_POINT('Ctrl Pts',(13.7154355939006,6.41687686636464,9.86054494281319E-16));
#43363=CARTESIAN_POINT('Ctrl Pts',(13.7154355939006,6.41687686636464,-0.352782973842772));
#43364=CARTESIAN_POINT('Ctrl Pts',(13.6907677796515,6.47048863474094,-0.727666221822788));
#43365=CARTESIAN_POINT('Ctrl Pts',(13.6377879061428,6.58029051604764,-1.08333333333332));
#43366=CARTESIAN_POINT('Origin',(11.1410986251693,8.88472967648709,1.08333333333333));
#43367=CARTESIAN_POINT('',(9.4500021963329,11.8316076987797,1.08333333333333));
#43368=CARTESIAN_POINT('Origin',(11.1410986251693,8.88472967648709,1.08333333333333));
#43369=CARTESIAN_POINT('',(9.4500021963329,11.8316076987797,-1.08333333333333));
#43370=CARTESIAN_POINT('Ctrl Pts',(9.4500021963329,11.8316076987798,1.08333333333334));
#43371=CARTESIAN_POINT('Ctrl Pts',(9.35474240837097,11.9076924734258,0.7276662218228));
#43372=CARTESIAN_POINT('Ctrl Pts',(9.30796390402485,11.9436715548399,0.352782973842779));
#43373=CARTESIAN_POINT('Ctrl Pts',(9.30796390402485,11.9436715548399,-0.352782973842777));
#43374=CARTESIAN_POINT('Ctrl Pts',(9.35474240837097,11.9076924734258,-0.7276662218228));
#43375=CARTESIAN_POINT('Ctrl Pts',(9.4500021963329,11.8316076987798,-1.08333333333334));
#43376=CARTESIAN_POINT('',(8.72113759169208,11.2696166353064,-1.08333333333333));
#43377=CARTESIAN_POINT('Origin',(11.1410986251693,8.88472967648709,-1.08333333333333));
#43378=CARTESIAN_POINT('Ctrl Pts',(8.72113759169207,11.2696166353064,-1.08333333333334));
#43379=CARTESIAN_POINT('Ctrl Pts',(8.63036626326973,11.3398611937657,-0.725928647976583));
#43380=CARTESIAN_POINT('Ctrl Pts',(8.5862330966948,11.3727349924819,-0.35203985917699));
#43381=CARTESIAN_POINT('Ctrl Pts',(8.5862330966948,11.3727349924819,0.352039859176991));
#43382=CARTESIAN_POINT('Ctrl Pts',(8.63036626326973,11.3398611937657,0.725928647976584));
#43383=CARTESIAN_POINT('Ctrl Pts',(8.72113759169207,11.2696166353064,1.08333333333334));
#43384=CARTESIAN_POINT('',(10.4434643792748,8.32838493021314,-3.45272288248773));
#43385=CARTESIAN_POINT('Origin',(10.4434643792748,8.32838493021314,9.23868777263706E-16));
#43386=CARTESIAN_POINT('',(11.8387328710639,9.44107442276105,-3.45272288248773));
#43387=CARTESIAN_POINT('Origin',(11.8387328710639,9.44107442276104,1.0472995612114E-15));
#43388=CARTESIAN_POINT('Origin',(0.,14.25,0.));
#43389=CARTESIAN_POINT('',(-3.35834339016074,14.7651959662676,1.08333333333333));
#43390=CARTESIAN_POINT('',(-3.39763111739558,14.25,1.08333333333333));
#43391=CARTESIAN_POINT('Origin',(1.55588456152529E-16,14.25,1.08333333333333));
#43392=CARTESIAN_POINT('',(-3.35834339016074,14.7651959662676,-1.08333333333333));
#43393=CARTESIAN_POINT('Ctrl Pts',(-3.35834339016074,14.7651959662676,-1.08333333333333));
#43394=CARTESIAN_POINT('Ctrl Pts',(-3.47722236863702,14.7381569460943,-0.727666221822795));
#43395=CARTESIAN_POINT('Ctrl Pts',(-3.53451786760282,14.7240166290356,-0.352782973842776));
#43396=CARTESIAN_POINT('Ctrl Pts',(-3.53451786760282,14.7240166290356,0.352782973842775));
#43397=CARTESIAN_POINT('Ctrl Pts',(-3.47722236863702,14.7381569460943,0.727666221822794));
#43398=CARTESIAN_POINT('Ctrl Pts',(-3.35834339016074,14.7651959662676,1.08333333333333));
#43399=CARTESIAN_POINT('',(-3.37340073180097,13.8449509750914,-1.08333333333333));
#43400=CARTESIAN_POINT('Origin',(-1.5558845615253E-16,14.25,-1.08333333333333));
#43401=CARTESIAN_POINT('',(-3.37340073180097,13.8449509750914,1.08333333333333));
#43402=CARTESIAN_POINT('Ctrl Pts',(-3.37340073180098,13.8449509750914,1.08333333333333));
#43403=CARTESIAN_POINT('Ctrl Pts',(-3.48491513664897,13.8177798586608,0.725928647976578));
#43404=CARTESIAN_POINT('Ctrl Pts',(-3.53813348671686,13.8037716378594,0.352039859176988));
#43405=CARTESIAN_POINT('Ctrl Pts',(-3.53813348671686,13.8037716378594,-0.352039859176988));
#43406=CARTESIAN_POINT('Ctrl Pts',(-3.48491513664897,13.8177798586608,-0.725928647976578));
#43407=CARTESIAN_POINT('Ctrl Pts',(-3.37340073180098,13.8449509750914,-1.08333333333333));
#43408=CARTESIAN_POINT('Origin',(1.55588456152529E-16,14.25,1.08333333333333));
#43409=CARTESIAN_POINT('',(3.39763111739558,14.25,1.08333333333333));
#43410=CARTESIAN_POINT('Origin',(0.,14.25,0.));
#43411=CARTESIAN_POINT('',(3.37340073180097,13.8449509750914,1.08333333333333));
#43412=CARTESIAN_POINT('Origin',(0.,14.25,1.08333333333333));
#43413=CARTESIAN_POINT('',(3.37340073180097,13.8449509750914,-1.08333333333333));
#43414=CARTESIAN_POINT('Ctrl Pts',(3.37340073180098,13.8449509750914,-1.08333333333333));
#43415=CARTESIAN_POINT('Ctrl Pts',(3.48491513664897,13.8177798586608,-0.725928647976578));
#43416=CARTESIAN_POINT('Ctrl Pts',(3.53813348671686,13.8037716378594,-0.352039859176988));
#43417=CARTESIAN_POINT('Ctrl Pts',(3.53813348671686,13.8037716378594,0.));
#43418=CARTESIAN_POINT('Ctrl Pts',(3.53813348671686,13.8037716378594,0.352039859176988));
#43419=CARTESIAN_POINT('Ctrl Pts',(3.48491513664897,13.8177798586608,0.725928647976578));
#43420=CARTESIAN_POINT('Ctrl Pts',(3.37340073180098,13.8449509750914,1.08333333333333));
#43421=CARTESIAN_POINT('',(3.35834339016074,14.7651959662676,-1.08333333333333));
#43422=CARTESIAN_POINT('Origin',(0.,14.25,-1.08333333333333));
#43423=CARTESIAN_POINT('',(3.35834339016074,14.7651959662676,1.08333333333333));
#43424=CARTESIAN_POINT('Ctrl Pts',(3.35834339016074,14.7651959662676,1.08333333333333));
#43425=CARTESIAN_POINT('Ctrl Pts',(3.47722236863702,14.7381569460943,0.727666221822794));
#43426=CARTESIAN_POINT('Ctrl Pts',(3.53451786760282,14.7240166290356,0.352782973842775));
#43427=CARTESIAN_POINT('Ctrl Pts',(3.53451786760282,14.7240166290356,0.));
#43428=CARTESIAN_POINT('Ctrl Pts',(3.53451786760282,14.7240166290356,-0.352782973842775));
#43429=CARTESIAN_POINT('Ctrl Pts',(3.47722236863702,14.7381569460943,-0.727666221822793));
#43430=CARTESIAN_POINT('Ctrl Pts',(3.35834339016074,14.7651959662676,-1.08333333333333));
#43431=CARTESIAN_POINT('Origin',(0.,14.25,1.08333333333333));
#43432=CARTESIAN_POINT('',(0.,13.3576923076923,-3.45272288248773));
#43433=CARTESIAN_POINT('Origin',(0.,13.3576923076923,0.));
#43434=CARTESIAN_POINT('',(0.,15.1423076923077,-3.45272288248773));
#43435=CARTESIAN_POINT('Origin',(0.,15.1423076923077,0.));
#43436=CARTESIAN_POINT('Origin',(0.,14.25,0.));
#43437=CARTESIAN_POINT('',(-4.85033905439415E-16,15.1423076923077,3.96060240207311));
#43438=CARTESIAN_POINT('Origin',(0.,15.1423076923077,0.));
#43439=CARTESIAN_POINT('',(-4.85033905439415E-16,13.3576923076923,3.96060240207311));
#43440=CARTESIAN_POINT('Origin',(3.08592870035031E-16,14.25,2.5198520116158));
#43441=CARTESIAN_POINT('Origin',(0.,13.3576923076923,0.));
#43442=CARTESIAN_POINT('',(-3.97254599103887,13.6850786752975,-1.08333333333333));
#43443=CARTESIAN_POINT('',(-4.03631672677061,14.5944383081266,-1.08333333333333));
#43444=CARTESIAN_POINT('Ctrl Pts',(-3.97254599103889,13.6850786752975,-1.08333333333333));
#43445=CARTESIAN_POINT('Ctrl Pts',(-4.03699073486477,13.8609255570095,-1.08333333333333));
#43446=CARTESIAN_POINT('Ctrl Pts',(-4.07292947680577,14.0696859538838,-1.08333333333333));
#43447=CARTESIAN_POINT('Ctrl Pts',(-4.07292947680577,14.358906139038,-1.08333333333333));
#43448=CARTESIAN_POINT('Ctrl Pts',(-4.06125577389194,14.4784021699804,-1.08333333333333));
#43449=CARTESIAN_POINT('Ctrl Pts',(-4.03631672677123,14.5944383081267,-1.08333333333333));
#43450=CARTESIAN_POINT('',(-4.03631672677098,14.5944383081279,1.08333333333333));
#43451=CARTESIAN_POINT('Ctrl Pts',(-4.03631672677125,14.5944383081264,1.08333333333353));
#43452=CARTESIAN_POINT('Ctrl Pts',(-4.07239878927587,14.5844592579328,0.956888632103535));
#43453=CARTESIAN_POINT('Ctrl Pts',(-4.10204391436992,14.576120838176,0.828820583351431));
#43454=CARTESIAN_POINT('Ctrl Pts',(-4.12523046485396,14.5695557880246,0.699646919262042));
#43455=CARTESIAN_POINT('Ctrl Pts',(-4.14829509982461,14.5630252570856,0.571152453813459));
#43456=CARTESIAN_POINT('Ctrl Pts',(-4.16496899480084,14.5582495239489,0.441563969171867));
#43457=CARTESIAN_POINT('Ctrl Pts',(-4.17521778805797,14.555309638438,0.311391073638072));
#43458=CARTESIAN_POINT('Ctrl Pts',(-4.18538433378736,14.5523933457842,0.182262827807668));
#43459=CARTESIAN_POINT('Ctrl Pts',(-4.18922853025337,14.5512835680019,0.0525595133522669));
#43460=CARTESIAN_POINT('Ctrl Pts',(-4.18670294427272,14.5520101946411,-0.0772214321944475));
#43461=CARTESIAN_POINT('Ctrl Pts',(-4.18498039512374,14.5525057826387,-0.165737150534356));
#43462=CARTESIAN_POINT('Ctrl Pts',(-4.1802944723506,14.5538546098955,-0.254288981130209));
#43463=CARTESIAN_POINT('Ctrl Pts',(-4.17262628304436,14.5560527668241,-0.342719102199544));
#43464=CARTESIAN_POINT('Ctrl Pts',(-4.16106584445129,14.5593666727772,-0.476034927301542));
#43465=CARTESIAN_POINT('Ctrl Pts',(-4.14279588034764,14.5645937486684,-0.608312350205319));
#43466=CARTESIAN_POINT('Ctrl Pts',(-4.11795181407459,14.5716147048116,-0.739057191236983));
#43467=CARTESIAN_POINT('Ctrl Pts',(-4.09589395251526,14.5778482769217,-0.855139299993905));
#43468=CARTESIAN_POINT('Ctrl Pts',(-4.06865355383155,14.5854950604866,-0.970013302477714));
#43469=CARTESIAN_POINT('Ctrl Pts',(-4.03631672677125,14.5944383081264,-1.08333333333353));
#43470=CARTESIAN_POINT('',(-3.97254599103887,13.6850786752975,1.08333333333333));
#43471=CARTESIAN_POINT('Ctrl Pts',(-3.97254599103889,13.6850786752975,1.08333333333333));
#43472=CARTESIAN_POINT('Ctrl Pts',(-4.03718797255354,13.8614637488071,1.08333333333333));
#43473=CARTESIAN_POINT('Ctrl Pts',(-4.07292947680577,14.0697175866198,1.08333333333333));
#43474=CARTESIAN_POINT('Ctrl Pts',(-4.07292947680577,14.3589686276554,1.08333333333333));
#43475=CARTESIAN_POINT('Ctrl Pts',(-4.06126656486658,14.4783519618466,1.08333333333333));
#43476=CARTESIAN_POINT('Ctrl Pts',(-4.03631672677098,14.5944383081279,1.08333333333333));
#43477=CARTESIAN_POINT('Ctrl Pts',(-3.97254599103885,13.6850786752975,-1.08333333333333));
#43478=CARTESIAN_POINT('Ctrl Pts',(-4.0055902844374,13.6754864779574,-0.949270311030653));
#43479=CARTESIAN_POINT('Ctrl Pts',(-4.03241557892495,13.6675742096383,-0.813521288368336));
#43480=CARTESIAN_POINT('Ctrl Pts',(-4.05298135839275,13.6614729113855,-0.67660705210156));
#43481=CARTESIAN_POINT('Ctrl Pts',(-4.07056281760631,13.6562569784544,-0.559560573778188));
#43482=CARTESIAN_POINT('Ctrl Pts',(-4.08356944187665,13.6523638057542,-0.441662516279225));
#43483=CARTESIAN_POINT('Ctrl Pts',(-4.09196781162929,13.6498461320482,-0.32323825833471));
#43484=CARTESIAN_POINT('Ctrl Pts',(-4.10167217606822,13.6469369456345,-0.186398348762652));
#43485=CARTESIAN_POINT('Ctrl Pts',(-4.10519527746315,13.6458740742379,-0.0492519096262281));
#43486=CARTESIAN_POINT('Ctrl Pts',(-4.1025698088094,13.6466633637621,0.0876758270660229));
#43487=CARTESIAN_POINT('Ctrl Pts',(-4.09993672885708,13.6474549414561,0.225000520654293));
#43488=CARTESIAN_POINT('Ctrl Pts',(-4.0911193595297,13.6501094100325,0.362105241912746));
#43489=CARTESIAN_POINT('Ctrl Pts',(-4.07613560843688,13.6545823261509,0.498460177595596));
#43490=CARTESIAN_POINT('Ctrl Pts',(-4.06108721528303,13.659074539074,0.635403368116582));
#43491=CARTESIAN_POINT('Ctrl Pts',(-4.03981905948952,13.6654009235528,0.771590289741077));
#43492=CARTESIAN_POINT('Ctrl Pts',(-4.01233468870309,13.673465922941,0.906484242526326));
#43493=CARTESIAN_POINT('Ctrl Pts',(-4.00026996096645,13.6770061903378,0.965698216399675));
#43494=CARTESIAN_POINT('Ctrl Pts',(-3.98700723595603,13.6808808214243,1.02466304565388));
#43495=CARTESIAN_POINT('Ctrl Pts',(-3.97254599103885,13.6850786752975,1.08333333333333));
#43496=CARTESIAN_POINT('',(4.0363167267713,14.5944383081264,-1.08333333333333));
#43497=CARTESIAN_POINT('',(3.97254599103947,13.6850786752973,-1.08333333333333));
#43498=CARTESIAN_POINT('Ctrl Pts',(4.0363167267713,14.5944383081264,-1.08333333333333));
#43499=CARTESIAN_POINT('Ctrl Pts',(4.06125577389196,14.4784021699801,-1.08333333333333));
#43500=CARTESIAN_POINT('Ctrl Pts',(4.07292947680577,14.3589061390379,-1.08333333333333));
#43501=CARTESIAN_POINT('Ctrl Pts',(4.07292947680577,14.0696859538838,-1.08333333333333));
#43502=CARTESIAN_POINT('Ctrl Pts',(4.03699073486477,13.8609255570095,-1.08333333333333));
#43503=CARTESIAN_POINT('Ctrl Pts',(3.97254599103889,13.6850786752975,-1.08333333333333));
#43504=CARTESIAN_POINT('',(3.972545991042,13.685078675306,1.08333333333333));
#43505=CARTESIAN_POINT('Ctrl Pts',(3.97254599103891,13.6850786752974,1.08333333333318));
#43506=CARTESIAN_POINT('Ctrl Pts',(4.00550358468898,13.6755116454224,0.949622058007565));
#43507=CARTESIAN_POINT('Ctrl Pts',(4.03223833992508,13.667626413385,0.814376693553222));
#43508=CARTESIAN_POINT('Ctrl Pts',(4.05275116551691,13.6615412011384,0.678132403728152));
#43509=CARTESIAN_POINT('Ctrl Pts',(4.07316650047532,13.6554849098804,0.542535637670838));
#43510=CARTESIAN_POINT('Ctrl Pts',(4.0874189867075,13.6512115628239,0.40594941879892));
#43511=CARTESIAN_POINT('Ctrl Pts',(4.09549564973878,13.6487880554638,0.268901316711817));
#43512=CARTESIAN_POINT('Ctrl Pts',(4.10076932144717,13.6472056219574,0.179415511018788));
#43513=CARTESIAN_POINT('Ctrl Pts',(4.10340966592831,13.6464108509735,0.0897327832366672));
#43514=CARTESIAN_POINT('Ctrl Pts',(4.10340966592831,13.6464108509735,-4.66293670342566E-15));
#43515=CARTESIAN_POINT('Ctrl Pts',(4.10340966592831,13.6464108509735,-0.137573936980382));
#43516=CARTESIAN_POINT('Ctrl Pts',(4.09720533291532,13.6482810316174,-0.274951212619736));
#43517=CARTESIAN_POINT('Ctrl Pts',(4.08483748845152,13.6519816397819,-0.41161240621476));
#43518=CARTESIAN_POINT('Ctrl Pts',(4.07237395114171,13.6557108803995,-0.549330978772818));
#43519=CARTESIAN_POINT('Ctrl Pts',(4.05365110225785,13.6612989721827,-0.686322345436846));
#43520=CARTESIAN_POINT('Ctrl Pts',(4.02869583028489,13.6686542829587,-0.822054935347102));
#43521=CARTESIAN_POINT('Ctrl Pts',(4.01257796374822,13.6734048590114,-0.909720570537157));
#43522=CARTESIAN_POINT('Ctrl Pts',(3.99385994844905,13.6788915953345,-0.996861109122728));
#43523=CARTESIAN_POINT('Ctrl Pts',(3.97254599103891,13.6850786752974,-1.08333333333318));
#43524=CARTESIAN_POINT('',(4.0363167267713,14.5944383081264,1.08333333333333));
#43525=CARTESIAN_POINT('Ctrl Pts',(4.0363167267713,14.5944383081264,1.08333333333333));
#43526=CARTESIAN_POINT('Ctrl Pts',(4.06125577389196,14.4784021699801,1.08333333333333));
#43527=CARTESIAN_POINT('Ctrl Pts',(4.07292947680577,14.3589061390379,1.08333333333333));
#43528=CARTESIAN_POINT('Ctrl Pts',(4.07292947680577,14.0696859538867,1.08333333333333));
#43529=CARTESIAN_POINT('Ctrl Pts',(4.03699073486612,13.8609255570161,1.08333333333333));
#43530=CARTESIAN_POINT('Ctrl Pts',(3.97254599104201,13.685078675306,1.08333333333333));
#43531=CARTESIAN_POINT('Ctrl Pts',(4.0363167267713,14.5944383081264,-1.08333333333333));
#43532=CARTESIAN_POINT('Ctrl Pts',(4.07267660468553,14.5843824238018,-0.955915065626592));
#43533=CARTESIAN_POINT('Ctrl Pts',(4.10254364280131,14.5759803979714,-0.826701571450557));
#43534=CARTESIAN_POINT('Ctrl Pts',(4.12584816889326,14.5693808768856,-0.696211209492171));
#43535=CARTESIAN_POINT('Ctrl Pts',(4.14878536602558,14.5628853783063,-0.567777653525462));
#43536=CARTESIAN_POINT('Ctrl Pts',(4.16536539316191,14.5581360328796,-0.438107164856169));
#43537=CARTESIAN_POINT('Ctrl Pts',(4.17550906341001,14.5552260824043,-0.307693975181436));
#43538=CARTESIAN_POINT('Ctrl Pts',(4.18345734283739,14.55294593144,-0.205506064179161));
#43539=CARTESIAN_POINT('Ctrl Pts',(4.18745357006455,14.5517942140162,-0.102862147740973));
#43540=CARTESIAN_POINT('Ctrl Pts',(4.18745357006455,14.5517942140162,4.44089209850063E-16));
#43541=CARTESIAN_POINT('Ctrl Pts',(4.18745357006455,14.5517942140162,0.13066680730557));
#43542=CARTESIAN_POINT('Ctrl Pts',(4.18100368362964,14.5536548201376,0.261069786498731));
#43543=CARTESIAN_POINT('Ctrl Pts',(4.16817103415993,14.5573291670729,0.390710450871123));
#43544=CARTESIAN_POINT('Ctrl Pts',(4.15518429935153,14.561047632956,0.521907748246283));
#43545=CARTESIAN_POINT('Ctrl Pts',(4.13566054561854,14.5666236366129,0.652324314224272));
#43546=CARTESIAN_POINT('Ctrl Pts',(4.10965488440249,14.5739568744946,0.781443489202978));
#43547=CARTESIAN_POINT('Ctrl Pts',(4.08920880779353,14.5797223861759,0.882959098491578));
#43548=CARTESIAN_POINT('Ctrl Pts',(4.06475571708163,14.586573067282,0.983672743459539));
#43549=CARTESIAN_POINT('Ctrl Pts',(4.0363167267713,14.5944383081264,1.08333333333333));
#43550=CARTESIAN_POINT('Origin',(0.,0.,-1.08333333333333));
#43551=CARTESIAN_POINT('Origin',(0.,0.,1.08333333333333));
#43552=CARTESIAN_POINT('Origin',(0.,0.,-1.08333333333333));
#43553=CARTESIAN_POINT('Origin',(0.,0.,-1.08333333333333));
#43554=CARTESIAN_POINT('Origin',(0.,0.,-1.08333333333333));
#43555=CARTESIAN_POINT('Origin',(0.,0.,1.08333333333333));
#43556=CARTESIAN_POINT('Origin',(0.,0.,-1.08333333333333));
#43557=CARTESIAN_POINT('Origin',(0.,0.,1.08333333333333));
#43558=CARTESIAN_POINT('Origin',(0.,15.1423076923077,-3.45272288248773));
#43559=CARTESIAN_POINT('Origin',(0.,13.3576923076923,-3.45272288248773));
#43560=CARTESIAN_POINT('Origin',(0.,0.,-1.08333333333333));
#43561=CARTESIAN_POINT('Origin',(0.,0.,-1.08333333333333));
#43562=CARTESIAN_POINT('Origin',(0.,0.,-1.08333333333333));
#43563=CARTESIAN_POINT('Origin',(0.,0.,1.08333333333333));
#43564=CARTESIAN_POINT('Origin',(0.,0.,1.08333333333333));
#43565=CARTESIAN_POINT('Origin',(0.,0.,1.08333333333333));
#43566=CARTESIAN_POINT('Origin',(0.,0.,-1.08333333333333));
#43567=CARTESIAN_POINT('Origin',(0.,0.,-1.08333333333333));
#43568=CARTESIAN_POINT('Origin',(10.4434643792748,8.32838493021314,-3.45272288248773));
#43569=CARTESIAN_POINT('Origin',(11.8387328710639,9.44107442276104,-3.45272288248773));
#43570=CARTESIAN_POINT('Origin',(-1.55588456152528E-16,7.49274514625042E-17,
1.08333333333333));
#43571=CARTESIAN_POINT('Origin',(-1.55588456152528E-16,7.49274514625042E-17,
1.08333333333333));
#43572=CARTESIAN_POINT('Origin',(-1.55588456152528E-16,7.49274514625042E-17,
1.08333333333333));
#43573=CARTESIAN_POINT('Origin',(1.55588456152528E-16,-7.49274514625042E-17,
-1.08333333333333));
#43574=CARTESIAN_POINT('Origin',(1.55588456152528E-16,-7.49274514625042E-17,
-1.08333333333333));
#43575=CARTESIAN_POINT('Origin',(1.55588456152528E-16,-7.49274514625042E-17,
-1.08333333333333));
#43576=CARTESIAN_POINT('Origin',(1.55588456152528E-16,-7.49274514625042E-17,
-1.08333333333333));
#43577=CARTESIAN_POINT('Origin',(1.55588456152528E-16,-7.49274514625042E-17,
-1.08333333333333));
#43578=CARTESIAN_POINT('Origin',(1.94015631396094E-16,-2.43287906657286E-16,
-1.08333333333333));
#43579=CARTESIAN_POINT('Origin',(-1.94015631396094E-16,2.43287906657286E-16,
1.08333333333333));
#43580=CARTESIAN_POINT('Origin',(1.94015631396094E-16,-2.43287906657286E-16,
-1.08333333333333));
#43581=CARTESIAN_POINT('Origin',(1.94015631396094E-16,-2.43287906657286E-16,
-1.08333333333333));
#43582=CARTESIAN_POINT('Origin',(1.94015631396094E-16,-2.43287906657286E-16,
-1.08333333333333));
#43583=CARTESIAN_POINT('Origin',(-1.94015631396094E-16,2.43287906657286E-16,
1.08333333333333));
#43584=CARTESIAN_POINT('Origin',(-1.94015631396094E-16,2.43287906657286E-16,
1.08333333333333));
#43585=CARTESIAN_POINT('Origin',(1.94015631396094E-16,-2.43287906657286E-16,
-1.08333333333333));
#43586=CARTESIAN_POINT('Origin',(13.0227870731057,-2.97236616780865,-3.45272288248773));
#43587=CARTESIAN_POINT('Origin',(14.7626584240763,-3.36948044994605,-3.45272288248773));
#43588=CARTESIAN_POINT('Origin',(-1.94015631396094E-16,2.43287906657286E-16,
1.08333333333333));
#43589=CARTESIAN_POINT('Origin',(-1.94015631396094E-16,2.43287906657286E-16,
1.08333333333333));
#43590=CARTESIAN_POINT('Origin',(-1.94015631396094E-16,2.43287906657286E-16,
1.08333333333333));
#43591=CARTESIAN_POINT('Origin',(1.94015631396094E-16,-2.43287906657286E-16,
-1.08333333333333));
#43592=CARTESIAN_POINT('Origin',(1.94015631396094E-16,-2.43287906657286E-16,
-1.08333333333333));
#43593=CARTESIAN_POINT('Origin',(1.94015631396094E-16,-2.43287906657286E-16,
-1.08333333333333));
#43594=CARTESIAN_POINT('Origin',(1.94015631396094E-16,-2.43287906657286E-16,
-1.08333333333333));
#43595=CARTESIAN_POINT('Origin',(1.94015631396094E-16,-2.43287906657286E-16,
-1.08333333333333));
#43596=CARTESIAN_POINT('Origin',(8.63450790007668E-17,-3.78302508895262E-16,
-1.08333333333333));
#43597=CARTESIAN_POINT('Origin',(-8.63450790007668E-17,3.78302508895262E-16,
1.08333333333333));
#43598=CARTESIAN_POINT('Origin',(8.63450790007668E-17,-3.78302508895262E-16,
-1.08333333333333));
#43599=CARTESIAN_POINT('Origin',(8.63450790007668E-17,-3.78302508895262E-16,
-1.08333333333333));
#43600=CARTESIAN_POINT('Origin',(8.63450790007668E-17,-3.78302508895262E-16,
-1.08333333333333));
#43601=CARTESIAN_POINT('Origin',(-8.63450790007668E-17,3.78302508895262E-16,
1.08333333333333));
#43602=CARTESIAN_POINT('Origin',(-8.63450790007668E-17,3.78302508895262E-16,
1.08333333333333));
#43603=CARTESIAN_POINT('Origin',(8.63450790007668E-17,-3.78302508895262E-16,
-1.08333333333333));
#43604=CARTESIAN_POINT('Origin',(5.79568548444348,-12.0348649162504,-3.45272288248773));
#43605=CARTESIAN_POINT('Origin',(6.57000108040713,-13.6427478189685,-3.45272288248772));
#43606=CARTESIAN_POINT('Origin',(-8.63450790007668E-17,3.78302508895262E-16,
1.08333333333333));
#43607=CARTESIAN_POINT('Origin',(-8.63450790007668E-17,3.78302508895262E-16,
1.08333333333333));
#43608=CARTESIAN_POINT('Origin',(-8.63450790007668E-17,3.78302508895262E-16,
1.08333333333333));
#43609=CARTESIAN_POINT('Origin',(8.63450790007668E-17,-3.78302508895262E-16,
-1.08333333333333));
#43610=CARTESIAN_POINT('Origin',(8.63450790007668E-17,-3.78302508895262E-16,
-1.08333333333333));
#43611=CARTESIAN_POINT('Origin',(8.63450790007668E-17,-3.78302508895262E-16,
-1.08333333333333));
#43612=CARTESIAN_POINT('Origin',(8.63450790007668E-17,-3.78302508895262E-16,
-1.08333333333333));
#43613=CARTESIAN_POINT('Origin',(8.63450790007668E-17,-3.78302508895262E-16,
-1.08333333333333));
#43614=CARTESIAN_POINT('Origin',(-8.63450790007644E-17,-3.78302508895264E-16,
-1.08333333333333));
#43615=CARTESIAN_POINT('Origin',(8.63450790007644E-17,3.78302508895264E-16,
1.08333333333333));
#43616=CARTESIAN_POINT('Origin',(-8.63450790007644E-17,-3.78302508895264E-16,
-1.08333333333333));
#43617=CARTESIAN_POINT('Origin',(-8.63450790007644E-17,-3.78302508895264E-16,
-1.08333333333333));
#43618=CARTESIAN_POINT('Origin',(-8.63450790007644E-17,-3.78302508895264E-16,
-1.08333333333333));
#43619=CARTESIAN_POINT('Origin',(8.63450790007644E-17,3.78302508895264E-16,
1.08333333333333));
#43620=CARTESIAN_POINT('Origin',(8.63450790007644E-17,3.78302508895264E-16,
1.08333333333333));
#43621=CARTESIAN_POINT('Origin',(-8.63450790007644E-17,-3.78302508895264E-16,
-1.08333333333333));
#43622=CARTESIAN_POINT('Origin',(-5.79568548444331,-12.0348649162504,-3.45272288248773));
#43623=CARTESIAN_POINT('Origin',(-6.57000108040694,-13.6427478189686,-3.45272288248772));
#43624=CARTESIAN_POINT('Origin',(8.63450790007644E-17,3.78302508895264E-16,
1.08333333333333));
#43625=CARTESIAN_POINT('Origin',(8.63450790007644E-17,3.78302508895264E-16,
1.08333333333333));
#43626=CARTESIAN_POINT('Origin',(8.63450790007644E-17,3.78302508895264E-16,
1.08333333333333));
#43627=CARTESIAN_POINT('Origin',(-8.63450790007644E-17,-3.78302508895264E-16,
-1.08333333333333));
#43628=CARTESIAN_POINT('Origin',(-8.63450790007644E-17,-3.78302508895264E-16,
-1.08333333333333));
#43629=CARTESIAN_POINT('Origin',(-8.63450790007644E-17,-3.78302508895264E-16,
-1.08333333333333));
#43630=CARTESIAN_POINT('Origin',(-8.63450790007644E-17,-3.78302508895264E-16,
-1.08333333333333));
#43631=CARTESIAN_POINT('Origin',(-8.63450790007644E-17,-3.78302508895264E-16,
-1.08333333333333));
#43632=CARTESIAN_POINT('Origin',(-1.94015631396093E-16,-2.43287906657289E-16,
-1.08333333333333));
#43633=CARTESIAN_POINT('Origin',(1.94015631396093E-16,2.43287906657289E-16,
1.08333333333333));
#43634=CARTESIAN_POINT('Origin',(-1.94015631396093E-16,-2.43287906657289E-16,
-1.08333333333333));
#43635=CARTESIAN_POINT('Origin',(-1.94015631396093E-16,-2.43287906657289E-16,
-1.08333333333333));
#43636=CARTESIAN_POINT('Origin',(-1.94015631396093E-16,-2.43287906657289E-16,
-1.08333333333333));
#43637=CARTESIAN_POINT('Origin',(1.94015631396093E-16,2.43287906657289E-16,
1.08333333333333));
#43638=CARTESIAN_POINT('Origin',(1.94015631396093E-16,2.43287906657289E-16,
1.08333333333333));
#43639=CARTESIAN_POINT('Origin',(-1.94015631396093E-16,-2.43287906657289E-16,
-1.08333333333333));
#43640=CARTESIAN_POINT('Origin',(-13.0227870731057,-2.97236616780882,-3.45272288248773));
#43641=CARTESIAN_POINT('Origin',(-14.7626584240763,-3.36948044994625,-3.45272288248773));
#43642=CARTESIAN_POINT('Origin',(1.94015631396093E-16,2.43287906657289E-16,
1.08333333333333));
#43643=CARTESIAN_POINT('Origin',(1.94015631396093E-16,2.43287906657289E-16,
1.08333333333333));
#43644=CARTESIAN_POINT('Origin',(1.94015631396093E-16,2.43287906657289E-16,
1.08333333333333));
#43645=CARTESIAN_POINT('Origin',(-1.94015631396093E-16,-2.43287906657289E-16,
-1.08333333333333));
#43646=CARTESIAN_POINT('Origin',(-1.94015631396093E-16,-2.43287906657289E-16,
-1.08333333333333));
#43647=CARTESIAN_POINT('Origin',(-1.94015631396093E-16,-2.43287906657289E-16,
-1.08333333333333));
#43648=CARTESIAN_POINT('Origin',(-1.94015631396093E-16,-2.43287906657289E-16,
-1.08333333333333));
#43649=CARTESIAN_POINT('Origin',(-1.94015631396093E-16,-2.43287906657289E-16,
-1.08333333333333));
#43650=CARTESIAN_POINT('Origin',(-1.55588456152529E-16,-7.49274514625064E-17,
-1.08333333333333));
#43651=CARTESIAN_POINT('Origin',(1.55588456152529E-16,7.49274514625064E-17,
1.08333333333333));
#43652=CARTESIAN_POINT('Origin',(-1.55588456152529E-16,-7.49274514625064E-17,
-1.08333333333333));
#43653=CARTESIAN_POINT('Origin',(-1.55588456152529E-16,-7.49274514625064E-17,
-1.08333333333333));
#43654=CARTESIAN_POINT('Origin',(-1.55588456152529E-16,-7.49274514625064E-17,
-1.08333333333333));
#43655=CARTESIAN_POINT('Origin',(1.55588456152529E-16,7.49274514625064E-17,
1.08333333333333));
#43656=CARTESIAN_POINT('Origin',(1.55588456152529E-16,7.49274514625064E-17,
1.08333333333333));
#43657=CARTESIAN_POINT('Origin',(-1.55588456152529E-16,-7.49274514625064E-17,
-1.08333333333333));
#43658=CARTESIAN_POINT('Origin',(-10.4434643792749,8.32838493021299,-3.45272288248773));
#43659=CARTESIAN_POINT('Origin',(-11.838732871064,9.44107442276088,-3.45272288248773));
#43660=CARTESIAN_POINT('Origin',(1.55588456152529E-16,7.49274514625064E-17,
1.08333333333333));
#43661=CARTESIAN_POINT('Origin',(1.55588456152529E-16,7.49274514625064E-17,
1.08333333333333));
#43662=CARTESIAN_POINT('Origin',(1.55588456152529E-16,7.49274514625064E-17,
1.08333333333333));
#43663=CARTESIAN_POINT('Origin',(-1.55588456152529E-16,-7.49274514625064E-17,
-1.08333333333333));
#43664=CARTESIAN_POINT('Origin',(-1.55588456152529E-16,-7.49274514625064E-17,
-1.08333333333333));
#43665=CARTESIAN_POINT('Origin',(-1.55588456152529E-16,-7.49274514625064E-17,
-1.08333333333333));
#43666=CARTESIAN_POINT('Origin',(-1.55588456152529E-16,-7.49274514625064E-17,
-1.08333333333333));
#43667=CARTESIAN_POINT('Origin',(-1.55588456152529E-16,-7.49274514625064E-17,
-1.08333333333333));
#43668=CARTESIAN_POINT('Origin',(0.,0.,-1.08333333333333));
#43669=CARTESIAN_POINT('Origin',(0.,0.,-1.08333333333333));
#43670=CARTESIAN_POINT('Origin',(0.,0.,-1.08333333333333));
#43671=CARTESIAN_POINT('Origin',(0.,0.,1.08333333333333));
#43672=CARTESIAN_POINT('Origin',(0.,0.,1.08333333333333));
#43673=CARTESIAN_POINT('Origin',(0.,0.,1.08333333333333));
#43674=CARTESIAN_POINT('Origin',(0.,0.,-1.08333333333333));
#43675=CARTESIAN_POINT('Origin',(0.,0.,-1.08333333333333));
#43676=CARTESIAN_POINT('',(0.,0.,0.));
#43677=CARTESIAN_POINT('Origin',(0.,-33.,7.49999756423169));
#43678=CARTESIAN_POINT('',(-2.57175827820944E-15,-45.,-13.5000024357683));
#43679=CARTESIAN_POINT('Origin',(0.,-45.,7.49999756423169));
#43680=CARTESIAN_POINT('',(-2.57175827820944E-15,-30.,-13.5000024357683));
#43681=CARTESIAN_POINT('',(-2.57175827820944E-15,-33.,-13.5000024357683));
#43682=CARTESIAN_POINT('Origin',(0.,-30.,7.49999756423169));
#43683=CARTESIAN_POINT('Origin',(0.,-45.,23.6225292964879));
#43684=CARTESIAN_POINT('',(58.1257387537822,-45.,-51.5400639196098));
#43685=CARTESIAN_POINT('',(-58.1257387537822,-45.,-51.5400639196098));
#43686=CARTESIAN_POINT('',(-58.1257387537822,-45.,-51.5400639196098));
#43687=CARTESIAN_POINT('',(58.1257387537822,-45.,98.7851225125855));
#43688=CARTESIAN_POINT('',(58.1257387537822,-45.,-51.5400639196098));
#43689=CARTESIAN_POINT('',(-58.1257387537822,-45.,98.7851225125855));
#43690=CARTESIAN_POINT('',(58.1257387537822,-45.,98.7851225125855));
#43691=CARTESIAN_POINT('',(-58.1257387537822,-45.,98.7851225125855));
#43692=CARTESIAN_POINT('',(3.70557314396981E-12,-44.9999999999997,46.5000021716098));
#43693=CARTESIAN_POINT('Origin',(3.70814490224802E-12,-44.9999999999994,
67.5000021716098));
#43694=CARTESIAN_POINT('Origin',(3.70814490224802E-12,-33.,67.5000021716096));
#43695=CARTESIAN_POINT('',(3.70557314396981E-12,-30.,46.5000021716096));
#43696=CARTESIAN_POINT('',(3.70557314396981E-12,-33.0000000000003,46.5000021716096));
#43697=CARTESIAN_POINT('Origin',(3.70814490224802E-12,-30.,67.5000021716098));
#43698=CARTESIAN_POINT('Origin',(0.,-30.,23.6225292964879));
#43699=CARTESIAN_POINT('',(58.1257387537822,-30.,-51.5400639196098));
#43700=CARTESIAN_POINT('',(-58.1257387537822,-30.,-51.5400639196098));
#43701=CARTESIAN_POINT('',(29.0628693768911,-30.,-51.5400639196098));
#43702=CARTESIAN_POINT('',(-58.1257387537822,-30.,98.7851225125855));
#43703=CARTESIAN_POINT('',(-58.1257387537822,-30.,-13.958767311561));
#43704=CARTESIAN_POINT('',(58.1257387537822,-30.,98.7851225125855));
#43705=CARTESIAN_POINT('',(-29.0628693768911,-30.,98.7851225125855));
#43706=CARTESIAN_POINT('',(58.1257387537822,-30.,61.2038259045367));
#43707=CARTESIAN_POINT('Origin',(58.1257387537822,5.,98.7851225125855));
#43708=CARTESIAN_POINT('',(58.1257387537822,5.,98.7851225125855));
#43709=CARTESIAN_POINT('',(58.1257387537822,5.,-51.5400639196098));
#43710=CARTESIAN_POINT('Origin',(58.1257387537822,5.,-51.5400639196098));
#43711=CARTESIAN_POINT('',(-58.1257387537822,5.,-51.5400639196098));
#43712=CARTESIAN_POINT('Origin',(-58.1257387537822,5.,98.7851225125855));
#43713=CARTESIAN_POINT('',(-58.1257387537822,5.,98.7851225125855));
#43714=CARTESIAN_POINT('Origin',(-58.1257387537822,5.,-51.5400639196098));
#43715=CARTESIAN_POINT('',(0.,0.,0.));
#43716=CARTESIAN_POINT('Origin',(3.70814490224802E-12,45.,67.5000021716098));
#43717=CARTESIAN_POINT('',(21.0000000000037,45.,67.5000021716098));
#43718=CARTESIAN_POINT('Origin',(3.70814490224802E-12,45.,67.5000021716098));
#43719=CARTESIAN_POINT('',(21.0000000000037,30.,67.5000021716098));
#43720=CARTESIAN_POINT('',(21.0000000000037,45.,67.5000021716098));
#43721=CARTESIAN_POINT('Origin',(3.70814490224802E-12,30.,67.5000021716098));
#43722=CARTESIAN_POINT('Origin',(0.,45.,7.49999756423169));
#43723=CARTESIAN_POINT('',(21.,45.,7.49999756423169));
#43724=CARTESIAN_POINT('Origin',(0.,45.,7.49999756423169));
#43725=CARTESIAN_POINT('',(21.,30.,7.49999756423169));
#43726=CARTESIAN_POINT('',(21.,45.,7.49999756423169));
#43727=CARTESIAN_POINT('Origin',(0.,30.,7.49999756423169));
#43728=CARTESIAN_POINT('Origin',(0.,30.,23.6225292964879));
#43729=CARTESIAN_POINT('',(58.1257387537822,30.,-51.5400639196098));
#43730=CARTESIAN_POINT('',(-58.1257387537822,30.,-51.5400639196098));
#43731=CARTESIAN_POINT('',(29.0628693768911,30.,-51.5400639196098));
#43732=CARTESIAN_POINT('',(58.1257387537822,30.,98.7851225125855));
#43733=CARTESIAN_POINT('',(58.1257387537822,30.,61.2038259045367));
#43734=CARTESIAN_POINT('',(-58.1257387537822,30.,98.7851225125855));
#43735=CARTESIAN_POINT('',(-29.0628693768911,30.,98.7851225125855));
#43736=CARTESIAN_POINT('',(-58.1257387537822,30.,-13.958767311561));
#43737=CARTESIAN_POINT('Origin',(58.1257387537822,-5.,98.7851225125855));
#43738=CARTESIAN_POINT('',(58.1257387537822,45.,-51.5400639196098));
#43739=CARTESIAN_POINT('',(58.1257387537822,-5.,-51.5400639196098));
#43740=CARTESIAN_POINT('',(58.1257387537822,45.,98.7851225125855));
#43741=CARTESIAN_POINT('',(58.1257387537822,45.,-51.5400639196098));
#43742=CARTESIAN_POINT('',(58.1257387537822,-5.,98.7851225125855));
#43743=CARTESIAN_POINT('Origin',(58.1257387537822,-5.,-51.5400639196098));
#43744=CARTESIAN_POINT('',(-58.1257387537822,45.,-51.5400639196098));
#43745=CARTESIAN_POINT('',(-58.1257387537822,-5.,-51.5400639196098));
#43746=CARTESIAN_POINT('',(-58.1257387537822,45.,-51.5400639196098));
#43747=CARTESIAN_POINT('Origin',(-58.1257387537822,-5.,98.7851225125855));
#43748=CARTESIAN_POINT('',(-58.1257387537822,45.,98.7851225125855));
#43749=CARTESIAN_POINT('',(58.1257387537822,45.,98.7851225125855));
#43750=CARTESIAN_POINT('',(-58.1257387537822,-5.,98.7851225125855));
#43751=CARTESIAN_POINT('Origin',(-58.1257387537822,-5.,-51.5400639196098));
#43752=CARTESIAN_POINT('',(-58.1257387537822,45.,98.7851225125855));
#43753=CARTESIAN_POINT('Origin',(0.,45.,23.6225292964879));
#43754=CARTESIAN_POINT('',(0.,7.50000243576834,7.49999756423168));
#43755=CARTESIAN_POINT('',(0.,7.49999782838924,67.5000021716107));
#43756=CARTESIAN_POINT('',(3.70814490224802E-12,-39.5,67.5000021716097));
#43757=CARTESIAN_POINT('',(0.,-39.5,7.49999756423169));
#43758=CARTESIAN_POINT('',(3.70814490224802E-12,39.5,67.5000021716097));
#43759=CARTESIAN_POINT('',(0.,39.5,7.49999756423169));
#43760=CARTESIAN_POINT('',(0.,0.,0.));
#43761=CARTESIAN_POINT('',(0.,0.,0.));
#43762=UNCERTAINTY_MEASURE_WITH_UNIT(LENGTH_MEASURE(0.01),#43782,
'DISTANCE_ACCURACY_VALUE',
'Maximum model space distance between geometric entities at asserted c
onnectivities');
#43763=UNCERTAINTY_MEASURE_WITH_UNIT(LENGTH_MEASURE(0.01),#43782,
'DISTANCE_ACCURACY_VALUE',
'Maximum model space distance between geometric entities at asserted c
onnectivities');
#43764=UNCERTAINTY_MEASURE_WITH_UNIT(LENGTH_MEASURE(0.01),#43782,
'DISTANCE_ACCURACY_VALUE',
'Maximum model space distance between geometric entities at asserted c
onnectivities');
#43765=UNCERTAINTY_MEASURE_WITH_UNIT(LENGTH_MEASURE(0.01),#43782,
'DISTANCE_ACCURACY_VALUE',
'Maximum model space distance between geometric entities at asserted c
onnectivities');
#43766=UNCERTAINTY_MEASURE_WITH_UNIT(LENGTH_MEASURE(0.01),#43782,
'DISTANCE_ACCURACY_VALUE',
'Maximum model space distance between geometric entities at asserted c
onnectivities');
#43767=UNCERTAINTY_MEASURE_WITH_UNIT(LENGTH_MEASURE(0.01),#43782,
'DISTANCE_ACCURACY_VALUE',
'Maximum model space distance between geometric entities at asserted c
onnectivities');
#43768=UNCERTAINTY_MEASURE_WITH_UNIT(LENGTH_MEASURE(0.01),#43782,
'DISTANCE_ACCURACY_VALUE',
'Maximum model space distance between geometric entities at asserted c
onnectivities');
#43769=UNCERTAINTY_MEASURE_WITH_UNIT(LENGTH_MEASURE(0.01),#43782,
'DISTANCE_ACCURACY_VALUE',
'Maximum model space distance between geometric entities at asserted c
onnectivities');
#43770=UNCERTAINTY_MEASURE_WITH_UNIT(LENGTH_MEASURE(0.01),#43782,
'DISTANCE_ACCURACY_VALUE',
'Maximum model space distance between geometric entities at asserted c
onnectivities');
#43771=UNCERTAINTY_MEASURE_WITH_UNIT(LENGTH_MEASURE(0.01),#43782,
'DISTANCE_ACCURACY_VALUE',
'Maximum model space distance between geometric entities at asserted c
onnectivities');
#43772=(
GEOMETRIC_REPRESENTATION_CONTEXT(3)
GLOBAL_UNCERTAINTY_ASSIGNED_CONTEXT((#43762))
GLOBAL_UNIT_ASSIGNED_CONTEXT((#43782,#43784,#43785))
REPRESENTATION_CONTEXT('','3D')
);
#43773=(
GEOMETRIC_REPRESENTATION_CONTEXT(3)
GLOBAL_UNCERTAINTY_ASSIGNED_CONTEXT((#43763))
GLOBAL_UNIT_ASSIGNED_CONTEXT((#43782,#43784,#43785))
REPRESENTATION_CONTEXT('','3D')
);
#43774=(
GEOMETRIC_REPRESENTATION_CONTEXT(3)
GLOBAL_UNCERTAINTY_ASSIGNED_CONTEXT((#43764))
GLOBAL_UNIT_ASSIGNED_CONTEXT((#43782,#43784,#43785))
REPRESENTATION_CONTEXT('','3D')
);
#43775=(
GEOMETRIC_REPRESENTATION_CONTEXT(3)
GLOBAL_UNCERTAINTY_ASSIGNED_CONTEXT((#43765))
GLOBAL_UNIT_ASSIGNED_CONTEXT((#43782,#43784,#43785))
REPRESENTATION_CONTEXT('','3D')
);
#43776=(
GEOMETRIC_REPRESENTATION_CONTEXT(3)
GLOBAL_UNCERTAINTY_ASSIGNED_CONTEXT((#43766))
GLOBAL_UNIT_ASSIGNED_CONTEXT((#43782,#43784,#43785))
REPRESENTATION_CONTEXT('','3D')
);
#43777=(
GEOMETRIC_REPRESENTATION_CONTEXT(3)
GLOBAL_UNCERTAINTY_ASSIGNED_CONTEXT((#43767))
GLOBAL_UNIT_ASSIGNED_CONTEXT((#43782,#43784,#43785))
REPRESENTATION_CONTEXT('','3D')
);
#43778=(
GEOMETRIC_REPRESENTATION_CONTEXT(3)
GLOBAL_UNCERTAINTY_ASSIGNED_CONTEXT((#43768))
GLOBAL_UNIT_ASSIGNED_CONTEXT((#43782,#43784,#43785))
REPRESENTATION_CONTEXT('','3D')
);
#43779=(
GEOMETRIC_REPRESENTATION_CONTEXT(3)
GLOBAL_UNCERTAINTY_ASSIGNED_CONTEXT((#43769))
GLOBAL_UNIT_ASSIGNED_CONTEXT((#43782,#43784,#43785))
REPRESENTATION_CONTEXT('','3D')
);
#43780=(
GEOMETRIC_REPRESENTATION_CONTEXT(3)
GLOBAL_UNCERTAINTY_ASSIGNED_CONTEXT((#43770))
GLOBAL_UNIT_ASSIGNED_CONTEXT((#43782,#43784,#43785))
REPRESENTATION_CONTEXT('','3D')
);
#43781=(
GEOMETRIC_REPRESENTATION_CONTEXT(3)
GLOBAL_UNCERTAINTY_ASSIGNED_CONTEXT((#43771))
GLOBAL_UNIT_ASSIGNED_CONTEXT((#43782,#43784,#43785))
REPRESENTATION_CONTEXT('','3D')
);
#43782=(
LENGTH_UNIT()
NAMED_UNIT(*)
SI_UNIT(.MILLI.,.METRE.)
);
#43783=(
LENGTH_UNIT()
NAMED_UNIT(*)
SI_UNIT($,.METRE.)
);
#43784=(
NAMED_UNIT(*)
PLANE_ANGLE_UNIT()
SI_UNIT($,.RADIAN.)
);
#43785=(
NAMED_UNIT(*)
SI_UNIT($,.STERADIAN.)
SOLID_ANGLE_UNIT()
);
#43786=SHAPE_DEFINITION_REPRESENTATION(#43795,#43812);
#43787=SHAPE_DEFINITION_REPRESENTATION(#43796,#43813);
#43788=SHAPE_DEFINITION_REPRESENTATION(#43797,#43814);
#43789=SHAPE_DEFINITION_REPRESENTATION(#43798,#43815);
#43790=SHAPE_DEFINITION_REPRESENTATION(#43799,#43816);
#43791=SHAPE_DEFINITION_REPRESENTATION(#43800,#43817);
#43792=SHAPE_DEFINITION_REPRESENTATION(#43801,#43818);
#43793=SHAPE_DEFINITION_REPRESENTATION(#43802,#43819);
#43794=SHAPE_DEFINITION_REPRESENTATION(#43803,#43820);
#43795=PRODUCT_DEFINITION_SHAPE('',$,#43822);
#43796=PRODUCT_DEFINITION_SHAPE('',$,#43823);
#43797=PRODUCT_DEFINITION_SHAPE('',$,#43824);
#43798=PRODUCT_DEFINITION_SHAPE('',$,#43825);
#43799=PRODUCT_DEFINITION_SHAPE('',$,#43826);
#43800=PRODUCT_DEFINITION_SHAPE('',$,#43827);
#43801=PRODUCT_DEFINITION_SHAPE('',$,#43828);
#43802=PRODUCT_DEFINITION_SHAPE('',$,#43829);
#43803=PRODUCT_DEFINITION_SHAPE('',$,#43830);
#43804=PRODUCT_DEFINITION_SHAPE($,$,#35);
#43805=PRODUCT_DEFINITION_SHAPE($,$,#36);
#43806=PRODUCT_DEFINITION_SHAPE($,$,#37);
#43807=PRODUCT_DEFINITION_SHAPE($,$,#38);
#43808=PRODUCT_DEFINITION_SHAPE($,$,#39);
#43809=PRODUCT_DEFINITION_SHAPE($,$,#40);
#43810=PRODUCT_DEFINITION_SHAPE($,$,#41);
#43811=PRODUCT_DEFINITION_SHAPE($,$,#42);
#43812=SHAPE_REPRESENTATION('',(#13184,#14905,#14906,#14907,#14908,#14909,
#14910,#14911,#14912),#43772);
#43813=SHAPE_REPRESENTATION('',(#13185),#43773);
#43814=SHAPE_REPRESENTATION('',(#13476),#43774);
#43815=SHAPE_REPRESENTATION('',(#13627),#43775);
#43816=SHAPE_REPRESENTATION('',(#13940),#43776);
#43817=SHAPE_REPRESENTATION('',(#14253),#43777);
#43818=SHAPE_REPRESENTATION('',(#14566),#43778);
#43819=SHAPE_REPRESENTATION('',(#14879),#43779);
#43820=SHAPE_REPRESENTATION('',(#14892),#43780);
#43821=PRODUCT_DEFINITION_CONTEXT('part definition',#43850,'design');
#43822=PRODUCT_DEFINITION('BR-258','BR-258',#43831,#43821);
#43823=PRODUCT_DEFINITION('Spur Gear 20 teeth','Spur Gear 20 teeth',#43832,
#43821);
#43824=PRODUCT_DEFINITION('Spur Gear 10 teeth','Spur Gear 10 teeth',#43833,
#43821);
#43825=PRODUCT_DEFINITION('5972K117_Steel Ball Bearing','Bearing_01',#43834,
#43821);
#43826=PRODUCT_DEFINITION('5972K117_Steel Ball Bearing_1','Bearing_02',
#43835,#43821);
#43827=PRODUCT_DEFINITION('5972K117_Steel Ball Bearing_2','Bearing_03',
#43836,#43821);
#43828=PRODUCT_DEFINITION('5972K117_Steel Ball Bearing_3','Bearing_04',
#43837,#43821);
#43829=PRODUCT_DEFINITION('Wall_02','Wall_02',#43838,#43821);
#43830=PRODUCT_DEFINITION('Wall_01','Wall_01',#43839,#43821);
#43831=PRODUCT_DEFINITION_FORMATION('',$,#43852);
#43832=PRODUCT_DEFINITION_FORMATION('',$,#43853);
#43833=PRODUCT_DEFINITION_FORMATION('',$,#43854);
#43834=PRODUCT_DEFINITION_FORMATION('',$,#43855);
#43835=PRODUCT_DEFINITION_FORMATION('',$,#43856);
#43836=PRODUCT_DEFINITION_FORMATION('',$,#43857);
#43837=PRODUCT_DEFINITION_FORMATION('',$,#43858);
#43838=PRODUCT_DEFINITION_FORMATION('',$,#43859);
#43839=PRODUCT_DEFINITION_FORMATION('',$,#43860);
#43840=PRODUCT_RELATED_PRODUCT_CATEGORY('BR-258','BR-258',(#43852));
#43841=PRODUCT_RELATED_PRODUCT_CATEGORY('Spur Gear 20 teeth',
'Spur Gear 20 teeth',(#43853));
#43842=PRODUCT_RELATED_PRODUCT_CATEGORY('Spur Gear 10 teeth',
'Spur Gear 10 teeth',(#43854));
#43843=PRODUCT_RELATED_PRODUCT_CATEGORY('Bearing_01','Bearing_01',(#43855));
#43844=PRODUCT_RELATED_PRODUCT_CATEGORY('Bearing_02','Bearing_02',(#43856));
#43845=PRODUCT_RELATED_PRODUCT_CATEGORY('Bearing_03','Bearing_03',(#43857));
#43846=PRODUCT_RELATED_PRODUCT_CATEGORY('Bearing_04','Bearing_04',(#43858));
#43847=PRODUCT_RELATED_PRODUCT_CATEGORY('Wall_02','Wall_02',(#43859));
#43848=PRODUCT_RELATED_PRODUCT_CATEGORY('Wall_01','Wall_01',(#43860));
#43849=APPLICATION_PROTOCOL_DEFINITION('international standard',
'automotive_design',2009,#43850);
#43850=APPLICATION_CONTEXT(
'Core Data for Automotive Mechanical Design Process');
#43851=PRODUCT_CONTEXT('part definition',#43850,'mechanical');
#43852=PRODUCT('BR-258','BR-258',$,(#43851));
#43853=PRODUCT('Spur Gear 20 teeth','Spur Gear 20 teeth',
'Spur Gear; Module: 4.0; Num Teeth: 20; Pressure Angle: 20.0; Backlash
: 0.00 mm',(#43851));
#43854=PRODUCT('Spur Gear 10 teeth','Spur Gear 10 teeth',
'Spur Gear; Module: 4.0; Num Teeth: 10; Pressure Angle: 20.0; Backlash
: 0.00 mm',(#43851));
#43855=PRODUCT('5972K117_Steel Ball Bearing','Bearing_01',$,(#43851));
#43856=PRODUCT('5972K117_Steel Ball Bearing_1','Bearing_02',$,(#43851));
#43857=PRODUCT('5972K117_Steel Ball Bearing_2','Bearing_03',$,(#43851));
#43858=PRODUCT('5972K117_Steel Ball Bearing_3','Bearing_04',$,(#43851));
#43859=PRODUCT('Wall_02','Wall_02',$,(#43851));
#43860=PRODUCT('Wall_01','Wall_01',$,(#43851));
#43861=PRESENTATION_STYLE_ASSIGNMENT((#43864));
#43862=PRESENTATION_STYLE_ASSIGNMENT((#43865));
#43863=PRESENTATION_STYLE_ASSIGNMENT((#43866));
#43864=SURFACE_STYLE_USAGE(.BOTH.,#43867);
#43865=SURFACE_STYLE_USAGE(.BOTH.,#43868);
#43866=SURFACE_STYLE_USAGE(.BOTH.,#43869);
#43867=SURFACE_SIDE_STYLE('',(#43870));
#43868=SURFACE_SIDE_STYLE('',(#43871));
#43869=SURFACE_SIDE_STYLE('',(#43872));
#43870=SURFACE_STYLE_FILL_AREA(#43873);
#43871=SURFACE_STYLE_FILL_AREA(#43874);
#43872=SURFACE_STYLE_FILL_AREA(#43875);
#43873=FILL_AREA_STYLE('Steel - Satin',(#43876));
#43874=FILL_AREA_STYLE('Opaque(203,203,203)',(#43877));
#43875=FILL_AREA_STYLE('Opaque(160,160,160)',(#43878));
#43876=FILL_AREA_STYLE_COLOUR('Steel - Satin',#43879);
#43877=FILL_AREA_STYLE_COLOUR('Opaque(203,203,203)',#43880);
#43878=FILL_AREA_STYLE_COLOUR('Opaque(160,160,160)',#43881);
#43879=COLOUR_RGB('Steel - Satin', 0.09019608, 0.27058824, 0.51372549);
#43880=COLOUR_RGB('Opaque(203,203,203)', 0.09019608, 0.27058824, 0.51372549);
#43881=COLOUR_RGB('Opaque(160,160,160)', 0.31764706, 0.68627451, 0.89019608);
ENDSEC;
END-ISO-10303-21;
